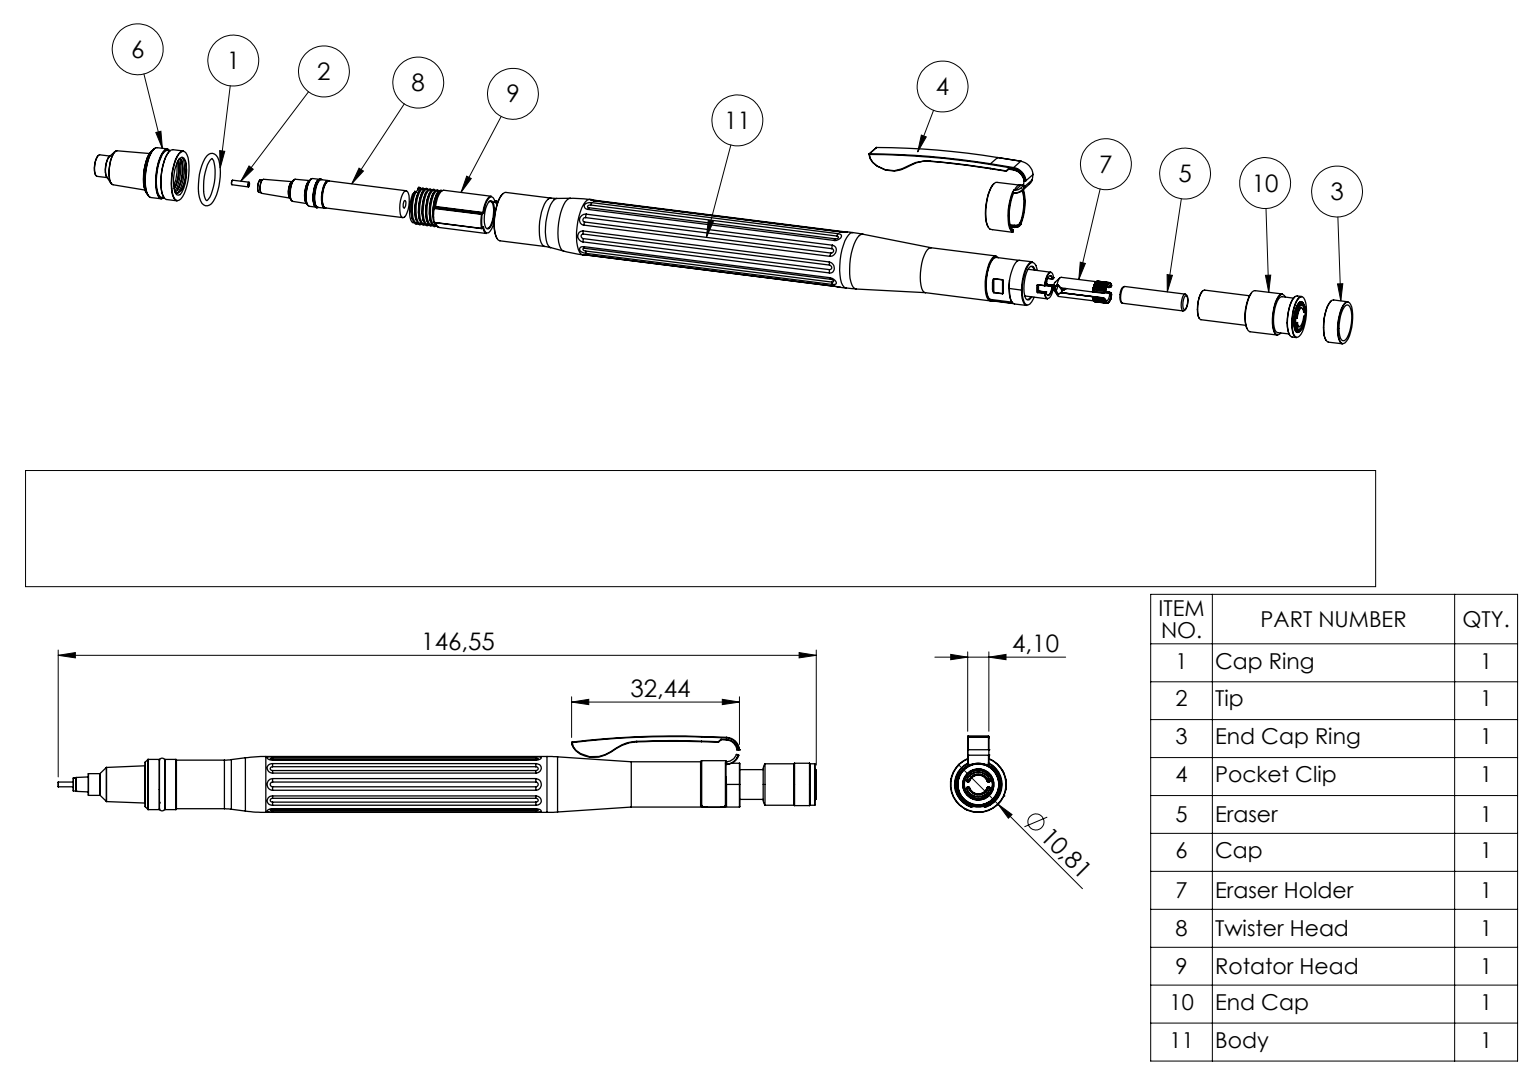
ISO-10303-21;
HEADER;
FILE_DESCRIPTION (('STEP AP214'),
    '1' );
FILE_NAME ('MAS-683',
    '2026-10-06T14:00:01',
    ( '' ),
    ( '' ),
    'SwSTEP 2.0',
    'SolidWorks 2020',
    '' );
FILE_SCHEMA (( 'AUTOMOTIVE_DESIGN' ));
ENDSEC;

DATA;
#1 = ORIENTED_EDGE ( 'NONE', *, *, #26816, .F. ) ;
#2 = CARTESIAN_POINT ( 'NONE',  ( 51.90000000000001279, -4.227689052994015206, -1.125730994152046804 ) ) ;
#3 = CARTESIAN_POINT ( 'NONE',  ( 15.76675455518197388, -3.095036031508637375, 4.435288302043580266 ) ) ;
#4 = CARTESIAN_POINT ( 'NONE',  ( 48.30000000000001847, 0.7900853852131533017, -4.025789903357282817 ) ) ;
#5 = ADVANCED_FACE ( 'NONE', ( #27029 ), #12933, .F. ) ;
#6 = FACE_OUTER_BOUND ( 'NONE', #21820, .T. ) ;
#7 = EDGE_CURVE ( 'NONE', #13124, #5233, #22627, .T. ) ;
#8 = CARTESIAN_POINT ( 'NONE',  ( -62.06147329307218286, -2.678446930503585843, 0.2197408810668839418 ) ) ;
#9 = AXIS2_PLACEMENT_3D ( 'NONE', #6479, #25787, #7416 ) ;
#10 = AXIS2_PLACEMENT_3D ( 'NONE', #12076, #19216, #28858 ) ;
#13 = EDGE_CURVE ( 'NONE', #19424, #10038, #3404, .T. ) ;
#12 = FACE_OUTER_BOUND ( 'NONE', #24808, .T. ) ;
#11 = PLANE ( 'NONE',  #16571 ) ;
#14 = B_SPLINE_CURVE_WITH_KNOTS ( 'NONE', 3,
 ( #5240, #644, #10304, #19973, #29610, #17605, #27249, #12178, #23901, #9510 ),
 .UNSPECIFIED., .F., .F.,
 ( 4, 2, 2, 2, 4 ),
 ( 0.000000000000000000, 0.0003925703575136129699, 0.0007851407150272259397, 0.001177711072540838910, 0.001570281430054451879 ),
 .UNSPECIFIED. ) ;
#15 = CARTESIAN_POINT ( 'NONE',  ( 61.23770293223015670, -0.8897917884444476178, 1.791164585743103999 ) ) ;
#17 = DIRECTION ( 'NONE',  ( 1.000000000000000000, 2.586136946169074517E-16, -0.000000000000000000 ) ) ;
#16 = CARTESIAN_POINT ( 'NONE',  ( -56.67499999999996874, 3.131991715727200307E-15, -1.107867533772800737E-16 ) ) ;
#18 = ORIENTED_EDGE ( 'NONE', *, *, #4179, .T. ) ;
#19 = CARTESIAN_POINT ( 'NONE',  ( 58.72419296898095809, -1.822284191842195256, 0.4419487341019822102 ) ) ;
#20 = FACE_OUTER_BOUND ( 'NONE', #25184, .T. ) ;
#22 = CARTESIAN_POINT ( 'NONE',  ( -35.98994760229849987, 4.804073784580248585, 2.042134692980175803 ) ) ;
#21 = DIRECTION ( 'NONE',  ( 0.000000000000000000, -1.000000000000000000, 0.000000000000000000 ) ) ;
#23 = LINE ( 'NONE', #15037, #26178 ) ;
#24 = ORIENTED_EDGE ( 'NONE', *, *, #28945, .F. ) ;
#25 = ORIENTED_EDGE ( 'NONE', *, *, #30906, .F. ) ;
#26 = FACE_OUTER_BOUND ( 'NONE', #14344, .T. ) ;
#27 = AXIS2_PLACEMENT_3D ( 'NONE', #565, #25255, #22895 ) ;
#28 = ORIENTED_EDGE ( 'NONE', *, *, #15447, .F. ) ;
#29 = CARTESIAN_POINT ( 'NONE',  ( 56.95000000000001705, 0.000000000000000000, 0.000000000000000000 ) ) ;
#30 = CARTESIAN_POINT ( 'NONE',  ( -35.85663232820584057, -3.426725943139554698, -3.937891353488750301 ) ) ;
#31 = ORIENTED_EDGE ( 'NONE', *, *, #27047, .T. ) ;
#32 = CARTESIAN_POINT ( 'NONE',  ( -59.59999999999998721, -2.157671697750204842, 1.538490443495526216 ) ) ;
#33 = ORIENTED_EDGE ( 'NONE', *, *, #2651, .T. ) ;
#34 = CARTESIAN_POINT ( 'NONE',  ( -60.95655989232410121, 1.962990915244748891, -3.400000000000207301 ) ) ;
#35 = ORIENTED_EDGE ( 'NONE', *, *, #5756, .F. ) ;
#36 = VERTEX_POINT ( 'NONE', #5192 ) ;
#37 = PRODUCT_DEFINITION_SHAPE ( 'NONE', 'NONE',  #1193 ) ;
#38 = ORIENTED_EDGE ( 'NONE', *, *, #18350, .T. ) ;
#39 = CIRCLE ( 'NONE', #6115, 0.4576450603546999840 ) ;
#40 = CARTESIAN_POINT ( 'NONE',  ( -59.74999999999995737, 2.023778652682510945E-14, -3.400000000000212186 ) ) ;
#41 = CARTESIAN_POINT ( 'NONE',  ( 53.71392934491857574, 7.814769211952036443, -2.050000000000187228 ) ) ;
#42 = CARTESIAN_POINT ( 'NONE',  ( 60.81599023037216512, -0.4999999999993630651, -1.863080903343643291 ) ) ;
#43 = CARTESIAN_POINT ( 'NONE',  ( -54.49999999999997868, -1.550000000000000044, 3.332135201338624508 ) ) ;
#44 = CARTESIAN_POINT ( 'NONE',  ( -58.09585481156723574, -1.184343223768586473, -3.558065644182725418 ) ) ;
#45 = EDGE_CURVE ( 'NONE', #27818, #13704, #24501, .T. ) ;
#47 = CARTESIAN_POINT ( 'NONE',  ( -35.85663232820581925, -0.4576450603547171925, -5.200000000000000178 ) ) ;
#46 = CARTESIAN_POINT ( 'NONE',  ( -59.69999999999997442, -3.399999999999991473, -2.235080921937235780E-13 ) ) ;
#48 =( NAMED_UNIT ( * ) PLANE_ANGLE_UNIT ( ) SI_UNIT ( $, .RADIAN. ) );
#49 = FACE_OUTER_BOUND ( 'NONE', #3992, .T. ) ;
#51 = DIRECTION ( 'NONE',  ( 0.000000000000000000, 1.224646799147353454E-16, 1.000000000000000000 ) ) ;
#50 = CARTESIAN_POINT ( 'NONE',  ( 54.42253022455169997, -6.265509898922181047E-05, -4.373069084971676013 ) ) ;
#52 = ORIENTED_EDGE ( 'NONE', *, *, #16574, .F. ) ;
#53 = DIRECTION ( 'NONE',  ( -1.000000000000000000, -0.000000000000000000, 3.491481338843133355E-15 ) ) ;
#54 = CARTESIAN_POINT ( 'NONE',  ( -36.00197790576391554, -4.683225679163350641, -2.703237727951247393 ) ) ;
#55 = AXIS2_PLACEMENT_3D ( 'NONE', #1109, #22822, #12810 ) ;
#57 = CARTESIAN_POINT ( 'NONE',  ( 54.19028661868582475, 6.697846887293304796, 2.049999999999810640 ) ) ;
#56 = CARTESIAN_POINT ( 'NONE',  ( 48.48092587705050960, -1.391939743175890420, 3.849999999996903899 ) ) ;
#58 = CARTESIAN_POINT ( 'NONE',  ( 47.10000000920868501, -4.079797993893489405, 2.128382101831542528 ) ) ;
#59 = ORIENTED_EDGE ( 'NONE', *, *, #31217, .T. ) ;
#60 = DIRECTION ( 'NONE',  ( 1.000000000000000000, 1.047444401652940007E-14, -0.000000000000000000 ) ) ;
#61 = AXIS2_PLACEMENT_3D ( 'NONE', #970, #25337, #5708 ) ;
#62 = EDGE_CURVE ( 'NONE', #4204, #12232, #6428, .T. ) ;
#63 = ORIENTED_EDGE ( 'NONE', *, *, #635, .F. ) ;
#64 = CARTESIAN_POINT ( 'NONE',  ( 51.80000000000002558, -3.933368109459642437, 2.186004417992994497 ) ) ;
#65 = CARTESIAN_POINT ( 'NONE',  ( -57.19702994616204705, 4.156921938165313080, -1.880369327726949834E-13 ) ) ;
#66 = VERTEX_POINT ( 'NONE', #447 ) ;
#67 = VERTEX_POINT ( 'NONE', #29413 ) ;
#68 = DIRECTION ( 'NONE',  ( 0.000000000000000000, -1.000000000000000000, 0.000000000000000000 ) ) ;
#69 = EDGE_LOOP ( 'NONE', ( #13659, #24370, #7129, #8608 ) ) ;
#70 = CARTESIAN_POINT ( 'NONE',  ( 48.45334018241207730, -1.329038565861417220, 3.861394075523871816 ) ) ;
#71 = CARTESIAN_POINT ( 'NONE',  ( -55.63452994616205416, 3.117691453623979481, 1.799999999999814415 ) ) ;
#72 = EDGE_LOOP ( 'NONE', ( #23840, #15915, #20433, #20236, #22335, #16297, #17891, #10389 ) ) ;
#73 = CARTESIAN_POINT ( 'NONE',  ( 63.50000000000004263, 0.7500000000000000000, 1.988246715072691018 ) ) ;
#74 = DIRECTION ( 'NONE',  ( -1.000000000000000000, -3.053848253006669023E-16, 2.042510438544995415E-16 ) ) ;
#75 = CARTESIAN_POINT ( 'NONE',  ( 29.99460041311888148, 6.535150002936795488, 2.049999999999441158 ) ) ;
#76 = VERTEX_POINT ( 'NONE', #8197 ) ;
#77 = CIRCLE ( 'NONE', #6150, 4.800000000000000711 ) ;
#78 = CARTESIAN_POINT ( 'NONE',  ( 56.95000000000001705, 0.6999999999999999556, -2.452039967047845437 ) ) ;
#79 = CARTESIAN_POINT ( 'NONE',  ( -54.49999516060625382, -1.549196738101655590, 4.063926895246979143 ) ) ;
#80 = DIRECTION ( 'NONE',  ( -1.000000000000000000, 0.000000000000000000, 1.047444401652940007E-14 ) ) ;
#81 = CARTESIAN_POINT ( 'NONE',  ( -59.60604010435355349, 3.187076279294280390, -1.184290838417780600 ) ) ;
#82 = CARTESIAN_POINT ( 'NONE',  ( 57.03951379057714632, 0.7794871794871794934, 1.732743413496389939 ) ) ;
#83 = EDGE_CURVE ( 'NONE', #616, #4702, #25049, .T. ) ;
#84 = B_SPLINE_CURVE_WITH_KNOTS ( 'NONE', 3,
 ( #27085, #16988, #10017, #5408 ),
 .UNSPECIFIED., .F., .F.,
 ( 4, 4 ),
 ( 0.000000000000000000, 2.862003379465075675E-05 ),
 .UNSPECIFIED. ) ;
#86 = CARTESIAN_POINT ( 'NONE',  ( -59.59999999999997300, -2.337126060168364994, -1.249136413240117038 ) ) ;
#85 =( NAMED_UNIT ( * ) SI_UNIT ( $, .STERADIAN. ) SOLID_ANGLE_UNIT ( ) );
#87 = FACE_OUTER_BOUND ( 'NONE', #20854, .T. ) ;
#88 = CARTESIAN_POINT ( 'NONE',  ( 51.80000000000001847, -3.726179070414208372, 1.041421356237310025 ) ) ;
#89 = AXIS2_PLACEMENT_3D ( 'NONE', #15577, #7805, #3067 ) ;
#90 = CARTESIAN_POINT ( 'NONE',  ( 61.24891880570161362, -0.9671362613607715764, -1.669082548205986116 ) ) ;
#91 = VERTEX_POINT ( 'NONE', #17714 ) ;
#92 = ORIENTED_EDGE ( 'NONE', *, *, #412, .F. ) ;
#93 = VECTOR ( 'NONE', #18197, 1000.000000000000000 ) ;
#94 = ADVANCED_FACE ( 'NONE', ( #17865 ), #19516, .T. ) ;
#95 = DIRECTION ( 'NONE',  ( 0.000000000000000000, -0.9996898646859343485, -0.02490330187381123786 ) ) ;
#96 = ORIENTED_EDGE ( 'NONE', *, *, #12745, .F. ) ;
#97 = CYLINDRICAL_SURFACE ( 'NONE', #25500, 1.000000000000000000 ) ;
#98 = CARTESIAN_POINT ( 'NONE',  ( -55.79792740578360366, 3.330682475591789871, 0.6830477631804102723 ) ) ;
#100 = PLANE ( 'NONE',  #28662 ) ;
#99 = CARTESIAN_POINT ( 'NONE',  ( 16.08093158123428523, 5.047763082740414298, 1.943828653492576608 ) ) ;
#101 = ORIENTED_EDGE ( 'NONE', *, *, #4763, .T. ) ;
#102 = ORIENTED_EDGE ( 'NONE', *, *, #5168, .T. ) ;
#103 = DIRECTION ( 'NONE',  ( 0.000000000000000000, 0.000000000000000000, -1.000000000000000000 ) ) ;
#104 = EDGE_LOOP ( 'NONE', ( #2125, #11645, #5974, #22411, #4642 ) ) ;
#105 = CYLINDRICAL_SURFACE ( 'NONE', #5460, 4.099999999999992539 ) ;
#106 =( BOUNDED_CURVE ( )  B_SPLINE_CURVE ( 2, ( #27982, #6938, #12441, #31145, #14352, #9477, #26546, #29083, #5166 ),
 .UNSPECIFIED., .F., .T. ) 
 B_SPLINE_CURVE_WITH_KNOTS ( ( 3, 2, 2, 2, 3 ),
 ( 0.5833333333333333703, 0.5925925925925925597, 0.6111111111111111605, 0.6296296296296296502, 0.6388888888888889506 ),
 .UNSPECIFIED. ) 
 CURVE ( )  GEOMETRIC_REPRESENTATION_ITEM ( )  RATIONAL_B_SPLINE_CURVE ( ( 0.9330127018922194093, 0.9330127018922197424, 1.000000000000000000, 0.8660254037844387076, 1.000000000000000000, 0.8660254037844387076, 1.000000000000000000, 0.9330127018922189652, 0.9330127018922194093 ) ) 
 REPRESENTATION_ITEM ( '' )  );
#107 = VERTEX_POINT ( 'NONE', #27203 ) ;
#108 = CARTESIAN_POINT ( 'NONE',  ( -36.40878371307408656, 5.360483378448119396, 0.7132926830813313135 ) ) ;
#109 = EDGE_LOOP ( 'NONE', ( #31265, #1632, #31131, #2632 ) ) ;
#110 = FACE_OUTER_BOUND ( 'NONE', #15279, .T. ) ;
#111 = EDGE_CURVE ( 'NONE', #4199, #30552, #22537, .T. ) ;
#112 = DIRECTION ( 'NONE',  ( 0.000000000000000000, 0.000000000000000000, -1.000000000000000000 ) ) ;
#113 = DIRECTION ( 'NONE',  ( -1.000000000000000000, -2.586136946169074517E-16, 0.000000000000000000 ) ) ;
#115 = CIRCLE ( 'NONE', #28430, 0.1000000000000002554 ) ;
#114 = CARTESIAN_POINT ( 'NONE',  ( -56.89405989232413674, -3.920666489018330156E-15, 3.399999999999796962 ) ) ;
#116 = CARTESIAN_POINT ( 'NONE',  ( 52.18319145150645255, 8.687974897284844289, -2.050000000000181455 ) ) ;
#117 = ADVANCED_FACE ( 'NONE', ( #25134 ), #3461, .F. ) ;
#118 = CARTESIAN_POINT ( 'NONE',  ( 58.65817410504259044, 0.5270377936603326541, 1.799623063671935475 ) ) ;
#119 = EDGE_CURVE ( 'NONE', #27144, #25407, #10724, .T. ) ;
#120 = CARTESIAN_POINT ( 'NONE',  ( 50.41422517315185559, 1.132063507975340277, -3.941224428058361262 ) ) ;
#121 = ADVANCED_FACE ( 'NONE', ( #2812 ), #19777, .T. ) ;
#122 = DIRECTION ( 'NONE',  ( 3.002035892788117459E-16, -0.9996898646859343485, -0.02490330187381124480 ) ) ;
#123 = ORIENTED_EDGE ( 'NONE', *, *, #26906, .T. ) ;
#124 = PLANE ( 'NONE',  #26575 ) ;
#125 = VERTEX_POINT ( 'NONE', #18190 ) ;
#126 = CARTESIAN_POINT ( 'NONE',  ( 61.25000000000002132, 6.415596960124259844E-13, 3.111507638930570854E-58 ) ) ;
#128 = CARTESIAN_POINT ( 'NONE',  ( 53.73313364444125995, 5.556159244632989491, 1.667741514041239048 ) ) ;
#127 = CARTESIAN_POINT ( 'NONE',  ( -36.21152527658242803, -3.291455042465435632, -4.036171416105485577 ) ) ;
#129 = CARTESIAN_POINT ( 'NONE',  ( 53.99324657738113586, 6.679477176219531742, 1.975347020395713526 ) ) ;
#130 = ORIENTED_EDGE ( 'NONE', *, *, #8388, .T. ) ;
#131 = EDGE_CURVE ( 'NONE', #11967, #18572, #4827, .T. ) ;
#132 = CARTESIAN_POINT ( 'NONE',  ( -54.45981523601835761, 1.500740478982482973, 4.030402907299741599 ) ) ;
#133 = VERTEX_POINT ( 'NONE', #3916 ) ;
#134 = FACE_OUTER_BOUND ( 'NONE', #215, .T. ) ;
#135 = CARTESIAN_POINT ( 'NONE',  ( 48.39253357792949117, 1.341874354110782486, 3.874311046529112623 ) ) ;
#137 = CARTESIAN_POINT ( 'NONE',  ( 47.44814918337031884, -3.852602532216165887, -1.405026670785768816 ) ) ;
#136 = CARTESIAN_POINT ( 'NONE',  ( 58.75000000000003553, -1.895722432252946010, 0.6373668173470157239 ) ) ;
#138 = ORIENTED_EDGE ( 'NONE', *, *, #14220, .T. ) ;
#139 = DIRECTION ( 'NONE',  ( 0.000000000000000000, 0.000000000000000000, 1.000000000000000000 ) ) ;
#140 = CARTESIAN_POINT ( 'NONE',  ( 15.03925126672133139, -3.817150320980667200, 2.203324261490537062 ) ) ;
#142 = LINE ( 'NONE', #17098, #13523 ) ;
#141 = CARTESIAN_POINT ( 'NONE',  ( 33.47623932017462778, 1.123735532908285650, -5.289358697221546279 ) ) ;
#143 = ORIENTED_EDGE ( 'NONE', *, *, #13652, .F. ) ;
#144 = CARTESIAN_POINT ( 'NONE',  ( -59.81249999999997158, 4.108500314926511798, -1.367561758111406567 ) ) ;
#145 = CARTESIAN_POINT ( 'NONE',  ( 58.65000000000003411, -1.394635017527761311, -1.253243060177727131 ) ) ;
#146 = DIRECTION ( 'NONE',  ( 0.000000000000000000, 0.000000000000000000, -1.000000000000000000 ) ) ;
#147 = EDGE_CURVE ( 'NONE', #30927, #10142, #27583, .T. ) ;
#148 = CARTESIAN_POINT ( 'NONE',  ( -41.12388279035661753, -1.755788972190012401E-14, 0.000000000000000000 ) ) ;
#149 = ITEM_DEFINED_TRANSFORMATION ( 'NONE', 'NONE', #18702,  #9018 ) ;
#150 = CARTESIAN_POINT ( 'NONE',  ( -61.38060080783325390, -2.623833477274086334, -0.6199702340732970995 ) ) ;
#151 = DIRECTION ( 'NONE',  ( 1.000000000000000000, -1.219044193948983948E-29, 3.491481338843133355E-15 ) ) ;
#153 = CARTESIAN_POINT ( 'NONE',  ( 68.00000000000001421, -1.025519176787267142E-28, -7.122621931239990530E-13 ) ) ;
#152 = AXIS2_PLACEMENT_3D ( 'NONE', #25976, #4453, #2803 ) ;
#154 = ORIENTED_EDGE ( 'NONE', *, *, #27235, .T. ) ;
#155 = ADVANCED_FACE ( 'NONE', ( #20723 ), #5995, .F. ) ;
#156 = CARTESIAN_POINT ( 'NONE',  ( 51.70000000000002416, 4.174380580618757719, 1.932497546739255556 ) ) ;
#157 = ADVANCED_FACE ( 'NONE', ( #22927 ), #25441, .T. ) ;
#158 = DIRECTION ( 'NONE',  ( -1.000000000000000000, -3.053848253006669023E-16, 2.042510438544995415E-16 ) ) ;
#159 = EDGE_CURVE ( 'NONE', #28004, #13558, #14466, .T. ) ;
#160 = CARTESIAN_POINT ( 'NONE',  ( -54.49999999999996447, 1.400000000000023670, -3.959797974644871044 ) ) ;
#161 = CARTESIAN_POINT ( 'NONE',  ( -56.62499999999997158, 1.184343223768582254, 3.558065644182727638 ) ) ;
#163 = CARTESIAN_POINT ( 'NONE',  ( 22.04321716858594371, 7.679566743993215816, 1.424999999999923661 ) ) ;
#162 = CARTESIAN_POINT ( 'NONE',  ( 58.75000000000001421, 0.5933779550744251452, 1.867062706146590756 ) ) ;
#164 = ORIENTED_EDGE ( 'NONE', *, *, #3455, .T. ) ;
#165 = CARTESIAN_POINT ( 'NONE',  ( 58.75000018803721247, -1.882836145342761780, 0.4533061784681521322 ) ) ;
#166 = LINE ( 'NONE', #7453, #15603 ) ;
#167 = AXIS2_PLACEMENT_3D ( 'NONE', #14057, #2660, #14363 ) ;
#169 = DIRECTION ( 'NONE',  ( 0.000000000000000000, -0.9996898646859343485, -0.02490330187381124133 ) ) ;
#168 = CARTESIAN_POINT ( 'NONE',  ( 51.64333574538936489, -0.8318165372340011743, -1.569663068107119974 ) ) ;
#170 = FACE_OUTER_BOUND ( 'NONE', #26252, .T. ) ;
#171 = VERTEX_POINT ( 'NONE', #25293 ) ;
#172 = ORIENTED_EDGE ( 'NONE', *, *, #3641, .F. ) ;
#173 = CARTESIAN_POINT ( 'NONE',  ( 51.41326833096621129, -0.9846823677975790057, -1.426744987257088315 ) ) ;
#174 = ORIENTED_EDGE ( 'NONE', *, *, #24601, .T. ) ;
#175 = DIRECTION ( 'NONE',  ( -3.491481338843133355E-15, -3.491481338843133355E-15, 1.000000000000000000 ) ) ;
#176 = CARTESIAN_POINT ( 'NONE',  ( 47.00000000000002132, 2.428612866367529932E-14, -4.100000000000022737 ) ) ;
#177 = ORIENTED_EDGE ( 'NONE', *, *, #3546, .F. ) ;
#178 = ADVANCED_FACE ( 'NONE', ( #15936 ), #13241, .T. ) ;
#179 = CARTESIAN_POINT ( 'NONE',  ( -35.98952425903315344, -5.086913993735696415, -1.171642046065874743 ) ) ;
#180 = ORIENTED_EDGE ( 'NONE', *, *, #3282, .F. ) ;
#181 = CARTESIAN_POINT ( 'NONE',  ( 58.74999999999980815, -1.394635017527639409, -1.253243060177863466 ) ) ;
#182 = EDGE_CURVE ( 'NONE', #17885, #28405, #12945, .T. ) ;
#183 = ORIENTED_EDGE ( 'NONE', *, *, #7527, .F. ) ;
#184 = EDGE_LOOP ( 'NONE', ( #28553, #23035, #27159, #29370 ) ) ;
#185 = CARTESIAN_POINT ( 'NONE',  ( -59.88452994616203995, -3.117691453623976816, 1.799999999999775335 ) ) ;
#186 = CARTESIAN_POINT ( 'NONE',  ( 54.23679421920400756, 6.620234584472831862, -2.050000000000189004 ) ) ;
#187 = FACE_OUTER_BOUND ( 'NONE', #28111, .T. ) ;
#188 = ADVANCED_FACE ( 'NONE', ( #10875 ), #20563, .T. ) ;
#189 = DIRECTION ( 'NONE',  ( 0.000000000000000000, -0.2008964009354148594, 0.9796124928211140670 ) ) ;
#190 = CARTESIAN_POINT ( 'NONE',  ( -61.37597047653181903, -2.565398393854171122, -0.8228970461733545738 ) ) ;
#191 = CARTESIAN_POINT ( 'NONE',  ( 46.99980596162997415, -4.243812330823901746, 1.064491855880303151 ) ) ;
#192 = CARTESIAN_POINT ( 'NONE',  ( 48.40116939571129961, 0.8930800907916158771, -3.925677024646232027 ) ) ;
#194 = CARTESIAN_POINT ( 'NONE',  ( 34.55000000000001847, 3.184081677783118191E-16, -2.600000000000000089 ) ) ;
#193 = DIRECTION ( 'NONE',  ( 0.9994629430332292452, 0.03275911391080331414, 0.0008160631928537054542 ) ) ;
#195 = ORIENTED_EDGE ( 'NONE', *, *, #1967, .T. ) ;
#196 = DIRECTION ( 'NONE',  ( 3.491481338843133750E-15, 0.000000000000000000, 1.000000000000000000 ) ) ;
#197 = CARTESIAN_POINT ( 'NONE',  ( -54.49999999999997868, 8.366749974758489177E-15, -2.216533082070116467E-13 ) ) ;
#199 = CARTESIAN_POINT ( 'NONE',  ( 52.72006341977384380, 4.014035108600657153, -0.8473018902927296203 ) ) ;
#198 = DIRECTION ( 'NONE',  ( 0.000000000000000000, 0.4531102586347437455, 0.8914544820235946743 ) ) ;
#200 = CARTESIAN_POINT ( 'NONE',  ( 48.00000000000002842, -4.387164041431067751, 1.383037119376590462 ) ) ;
#201 = ORIENTED_EDGE ( 'NONE', *, *, #2247, .T. ) ;
#202 = DIRECTION ( 'NONE',  ( 0.000000000000000000, -1.000000000000000000, 0.000000000000000000 ) ) ;
#203 = VERTEX_POINT ( 'NONE', #8511 ) ;
#204 = AXIS2_PLACEMENT_3D ( 'NONE', #12059, #22191, #17129 ) ;
#205 = CARTESIAN_POINT ( 'NONE',  ( 29.29107486424064888, 6.659593085418571867, 1.424999999999898126 ) ) ;
#206 = EDGE_LOOP ( 'NONE', ( #13546, #11977, #21657, #23791 ) ) ;
#207 = VERTEX_POINT ( 'NONE', #28132 ) ;
#208 = EDGE_CURVE ( 'NONE', #30643, #11413, #10315, .T. ) ;
#209 = CARTESIAN_POINT ( 'NONE',  ( 15.41170998834797778, 5.326676561279727551, 0.9978806102897876951 ) ) ;
#210 = ORIENTED_EDGE ( 'NONE', *, *, #23024, .T. ) ;
#211 = EDGE_CURVE ( 'NONE', #19416, #22328, #13432, .T. ) ;
#212 = B_SPLINE_CURVE_WITH_KNOTS ( 'NONE', 3,
 ( #23853, #28760, #23704, #11809, #1994, #9613, #29059, #26699, #21656, #24001, #19271, #11968, #26052 ),
 .UNSPECIFIED., .F., .F.,
 ( 4, 3, 3, 3, 4 ),
 ( 0.000000000000000000, 3.429247765843156239E-05, 6.861252194981137440E-05, 0.0001025118211733701013, 0.0001105094600589245180 ),
 .UNSPECIFIED. ) ;
#213 = CARTESIAN_POINT ( 'NONE',  ( 48.48434962373865886, -1.386108502191528924, 3.851082811767820413 ) ) ;
#214 = CARTESIAN_POINT ( 'NONE',  ( -55.32202994616205416, -4.156921938165296204, -2.115361882398036228E-13 ) ) ;
#215 = EDGE_LOOP ( 'NONE', ( #11588, #9037, #5325, #4414 ) ) ;
#216 = CARTESIAN_POINT ( 'NONE',  ( 54.49969840703174384, -0.002993017367635220170, 4.282759600741086636 ) ) ;
#217 = ADVANCED_FACE ( 'NONE', ( #691 ), #11323, .F. ) ;
#218 = FACE_OUTER_BOUND ( 'NONE', #18883, .T. ) ;
#219 = CIRCLE ( 'NONE', #12340, 2.000000000000000000 ) ;
#220 = CARTESIAN_POINT ( 'NONE',  ( 27.52339381995009049, 5.460762561607864995, 2.049999999999904787 ) ) ;
#221 = ORIENTED_EDGE ( 'NONE', *, *, #12347, .T. ) ;
#222 = CARTESIAN_POINT ( 'NONE',  ( -54.99999999999997868, 2.944486372867092250, 1.699999999999816103 ) ) ;
#223 = PLANE ( 'NONE',  #2312 ) ;
#224 = CARTESIAN_POINT ( 'NONE',  ( 58.75000000000000000, 2.008165151418601191, 0.5380862305919300592 ) ) ;
#225 = CYLINDRICAL_SURFACE ( 'NONE', #7886, 1.000000000000000000 ) ;
#226 = PLANE ( 'NONE',  #873 ) ;
#227 = CIRCLE ( 'NONE', #16912, 5.147405183146873675 ) ;
#228 = EDGE_CURVE ( 'NONE', #8009, #12847, #30638, .T. ) ;
#229 = DIRECTION ( 'NONE',  ( -1.000000000000000000, 0.000000000000000000, 1.047444401652940007E-14 ) ) ;
#230 = VECTOR ( 'NONE', #19201, 1000.000000000000000 ) ;
#231 = CARTESIAN_POINT ( 'NONE',  ( -59.63746166535423043, 3.180335144039268869, -1.202432085119870431 ) ) ;
#232 = CARTESIAN_POINT ( 'NONE',  ( 58.66133336607628479, 1.875011749337246014, -0.03256983989501838900 ) ) ;
#233 = DIRECTION ( 'NONE',  ( 1.000000000000000000, 1.047444401652940007E-14, 0.000000000000000000 ) ) ;
#234 = ORIENTED_EDGE ( 'NONE', *, *, #24307, .F. ) ;
#235 = ORIENTED_EDGE ( 'NONE', *, *, #4200, .F. ) ;
#236 = VERTEX_POINT ( 'NONE', #8450 ) ;
#237 =( BOUNDED_SURFACE ( )  B_SPLINE_SURFACE ( 3, 2, ( 
 ( #18207, #22472, #769 ),
 ( #20118, #8066, #17731 ),
 ( #5683, #3307, #12957 ),
 ( #11840, #21216, #1694 ),
 ( #4235, #13877, #16129 ),
 ( #28318, #30847, #18668 ),
 ( #14053, #11689, #9166 ),
 ( #18827, #11541, #18508 ),
 ( #23571, #16434, #23884 ),
 ( #28471, #4086, #21370 ),
 ( #6773, #6625, #1872 ),
 ( #26091, #21047, #30996 ),
 ( #16288, #9487, #23735 ),
 ( #25616, #2026, #30687 ),
 ( #28630, #2175, #8818 ),
 ( #21517, #4405, #13726 ) ),
 .UNSPECIFIED., .F., .F., .F. ) 
 B_SPLINE_SURFACE_WITH_KNOTS ( ( 4, 2, 2, 2, 2, 2, 2, 4 ),
 ( 3, 3 ),
 ( 0.001780502285214259107, 0.002558945925323788048, 0.002753556835351170500, 0.002948167745378552952, 0.003337389565433317423, 0.003726611385488081893, 0.004115833205542846797, 0.004894276845652375738 ),
 ( 0.000000000000000000, 1.000000000000000000 ),
 .UNSPECIFIED. ) 
 GEOMETRIC_REPRESENTATION_ITEM ( )  RATIONAL_B_SPLINE_SURFACE ( (
 ( 1.000000000000000000, 0.9418517008537233837, 1.000000000000000000),
 ( 1.000000000000000000, 0.9417987965885065149, 1.000000000000000000),
 ( 1.000000000000000000, 0.9418198861734086158, 1.000000000000000000),
 ( 1.000000000000000000, 0.9434060303845573925, 1.000000000000000000),
 ( 1.000000000000000000, 0.9437939819948161224, 1.000000000000000000),
 ( 1.000000000000000000, 0.9445989566712799101, 1.000000000000000000),
 ( 1.000000000000000000, 0.9450169930049959754, 1.000000000000000000),
 ( 1.000000000000000000, 0.9461610507673308135, 1.000000000000000000),
 ( 1.000000000000000000, 0.9467217966427053932, 1.000000000000000000),
 ( 1.000000000000000000, 0.9467345476124492398, 1.000000000000000000),
 ( 1.000000000000000000, 0.9461964028052997078, 1.000000000000000000),
 ( 1.000000000000000000, 0.9446801822473757104, 1.000000000000000000),
 ( 1.000000000000000000, 0.9437582546536171790, 1.000000000000000000),
 ( 1.000000000000000000, 0.9418129560296412128, 1.000000000000000000),
 ( 1.000000000000000000, 0.9418016889776917866, 1.000000000000000000),
 ( 1.000000000000000000, 0.9418517008537223845, 1.000000000000000000) ) ) 
 REPRESENTATION_ITEM ( '' )  SURFACE ( )  );
#238 = FACE_OUTER_BOUND ( 'NONE', #13734, .T. ) ;
#239 = CARTESIAN_POINT ( 'NONE',  ( -54.86042740578361077, -0.7887156198831597465, 3.845940847736172952 ) ) ;
#241 = CARTESIAN_POINT ( 'NONE',  ( -67.99999999999995737, -0.5554785485864222050, 2.708628542650383331 ) ) ;
#240 = CARTESIAN_POINT ( 'NONE',  ( 16.10667815269232150, 5.098435263432238962, 1.807398698456221142 ) ) ;
#242 = ORIENTED_EDGE ( 'NONE', *, *, #16474, .T. ) ;
#243 = AXIS2_PLACEMENT_3D ( 'NONE', #15272, #24917, #10208 ) ;
#244 = ORIENTED_EDGE ( 'NONE', *, *, #10930, .T. ) ;
#245 = AXIS2_PLACEMENT_3D ( 'NONE', #26689, #7358, #17036 ) ;
#246 = CARTESIAN_POINT ( 'NONE',  ( -44.49999999999997868, -1.499999999999998668, 4.029888335921975262 ) ) ;
#247 = VERTEX_POINT ( 'NONE', #25065 ) ;
#248 = EDGE_CURVE ( 'NONE', #1696, #20370, #611, .T. ) ;
#249 = DIRECTION ( 'NONE',  ( 1.000000000000000000, 1.047444401652940007E-14, 0.000000000000000000 ) ) ;
#250 = ORIENTED_EDGE ( 'NONE', *, *, #30955, .F. ) ;
#251 = CARTESIAN_POINT ( 'NONE',  ( 31.90749320720395588, 7.645246318247174599, -2.050000000000176570 ) ) ;
#252 = ADVANCED_FACE ( 'NONE', ( #17489 ), #5461, .T. ) ;
#253 = ORIENTED_EDGE ( 'NONE', *, *, #12134, .F. ) ;
#254 = CIRCLE ( 'NONE', #19476, 1.260000000000000231 ) ;
#255 = DIRECTION ( 'NONE',  ( -1.000000000000000000, -0.000000000000000000, 3.491481338843133355E-15 ) ) ;
#256 = DIRECTION ( 'NONE',  ( -1.000000000000000000, -0.000000000000000000, -0.000000000000000000 ) ) ;
#257 = CARTESIAN_POINT ( 'NONE',  ( 16.07512358269907438, -5.233646053067085191, -1.367284724151294872 ) ) ;
#258 = CIRCLE ( 'NONE', #12381, 0.2999999999999999334 ) ;
#259 = CARTESIAN_POINT ( 'NONE',  ( -54.45655989232412963, -3.925981830489445379, -2.076939516179772989E-13 ) ) ;
#260 = CARTESIAN_POINT ( 'NONE',  ( 53.91678946233204073, 6.821600947619984368, -1.787725782035514355 ) ) ;
#261 = EDGE_CURVE ( 'NONE', #13894, #14026, #10669, .T. ) ;
#262 = PLANE ( 'NONE',  #2851 ) ;
#263 = CARTESIAN_POINT ( 'NONE',  ( -36.39645873810205501, -3.590618801409528160, -4.051716037497291367 ) ) ;
#264 = AXIS2_PLACEMENT_3D ( 'NONE', #11573, #21251, #6807 ) ;
#265 = FILL_AREA_STYLE_COLOUR ( '', #10390 ) ;
#266 = CIRCLE ( 'NONE', #22541, 1.000000000000000000 ) ;
#267 = FACE_OUTER_BOUND ( 'NONE', #20625, .T. ) ;
#268 = ORIENTED_EDGE ( 'NONE', *, *, #4535, .F. ) ;
#269 = CARTESIAN_POINT ( 'NONE',  ( 56.99370871690835116, -0.8156862421929632623, -2.468735699563065378 ) ) ;
#270 = CARTESIAN_POINT ( 'NONE',  ( 51.50435016707359637, -0.9265794315402092751, -1.339215852266876672 ) ) ;
#271 = CARTESIAN_POINT ( 'NONE',  ( 53.91582462592152325, 6.672259099522118930, 0.8960560279709253173 ) ) ;
#272 = VECTOR ( 'NONE', #16238, 1000.000000000000000 ) ;
#273 = EDGE_LOOP ( 'NONE', ( #11335, #9422, #18646, #936 ) ) ;
#274 = CARTESIAN_POINT ( 'NONE',  ( 36.55000000000001847, 0.000000000000000000, -1.899999999999999911 ) ) ;
#275 =( BOUNDED_SURFACE ( )  B_SPLINE_SURFACE ( 3, 2, ( 
 ( #24839, #13578, #27853 ),
 ( #16132, #30851, #18355 ),
 ( #9002, #13880, #21051 ),
 ( #20886, #11544, #16291 ),
 ( #27992, #25934, #28322 ),
 ( #8822, #3767, #18511 ),
 ( #25783, #1876, #23266 ),
 ( #13729, #20588, #1550 ),
 ( #30222, #8528, #28153 ),
 ( #11213, #23111, #18831 ) ),
 .UNSPECIFIED., .F., .F., .T. ) 
 B_SPLINE_SURFACE_WITH_KNOTS ( ( 4, 2, 2, 2, 4 ),
 ( 3, 3 ),
 ( 0.0001706658715693258458, 0.0002229276920778027425, 0.0002751895125862796393, 0.0003274513330947565631, 0.0003797131536032334869 ),
 ( 0.000000000000000000, 1.000000000000000000 ),
 .UNSPECIFIED. ) 
 GEOMETRIC_REPRESENTATION_ITEM ( )  RATIONAL_B_SPLINE_SURFACE ( (
 ( 1.000000000000000000, 0.7071067811865444641, 1.000000000000000000),
 ( 1.000000000000000000, 0.7375607040701035455, 1.000000000000000000),
 ( 1.000000000000000000, 0.7730431127426561355, 1.000000000000000000),
 ( 1.000000000000000000, 0.8321012486983990764, 1.000000000000000000),
 ( 1.000000000000000000, 0.8541932017405543531, 1.000000000000000000),
 ( 1.000000000000000000, 0.8545723906055556762, 1.000000000000000000),
 ( 1.000000000000000000, 0.8327032135045047134, 1.000000000000000000),
 ( 1.000000000000000000, 0.7734559727062164658, 1.000000000000000000),
 ( 1.000000000000000000, 0.7377766653995503354, 1.000000000000000000),
 ( 1.000000000000000000, 0.7071067811865452413, 1.000000000000000000) ) ) 
 REPRESENTATION_ITEM ( '' )  SURFACE ( )  );
#276 = ORIENTED_EDGE ( 'NONE', *, *, #13970, .F. ) ;
#277 = TOROIDAL_SURFACE ( 'NONE', #6855, 3.950000000000000178, 0.05000000000000000278 ) ;
#278 = CARTESIAN_POINT ( 'NONE',  ( 15.22780280894145832, 0.7747498539022198427, -5.363501450340349308 ) ) ;
#279 = CARTESIAN_POINT ( 'NONE',  ( -36.56390771145526486, -5.205077242910963520, 1.471673150993815238 ) ) ;
#281 = DIRECTION ( 'NONE',  ( 0.9993908270190958731, -0.03489949670249358621, 0.000000000000000000 ) ) ;
#280 = CARTESIAN_POINT ( 'NONE',  ( 48.50000000000002132, -1.426739617975173013, -3.843750000000023093 ) ) ;
#282 = ORIENTED_EDGE ( 'NONE', *, *, #8503, .F. ) ;
#283 = DIRECTION ( 'NONE',  ( 0.000000000000000000, 0.9985773570672645816, 0.05332224631949589871 ) ) ;
#284 = ADVANCED_FACE ( 'NONE', ( #30591 ), #18007, .F. ) ;
#286 = CARTESIAN_POINT ( 'NONE',  ( 50.25000000000002132, 5.263408118306026973E-13, 3.111507638930570854E-58 ) ) ;
#285 = CARTESIAN_POINT ( 'NONE',  ( 51.80000048712027905, 3.919471135816211316, 2.045252759501752227 ) ) ;
#287 = EDGE_LOOP ( 'NONE', ( #23710, #1168, #11704, #9445, #24779, #21712, #30444 ) ) ;
#288 = CARTESIAN_POINT ( 'NONE',  ( -57.93749999999997158, -4.108500314926507357, 1.367561758111406567 ) ) ;
#289 = FACE_OUTER_BOUND ( 'NONE', #17501, .T. ) ;
#290 = CARTESIAN_POINT ( 'NONE',  ( 57.04536243881683788, -0.7794871794871796045, 1.732743413496389939 ) ) ;
#291 = AXIS2_PLACEMENT_3D ( 'NONE', #19148, #17077, #12003 ) ;
#292 = DIRECTION ( 'NONE',  ( -1.000000000000000000, -0.000000000000000000, -0.000000000000000000 ) ) ;
#293 = AXIS2_PLACEMENT_3D ( 'NONE', #30543, #21080, #28187 ) ;
#294 = FACE_OUTER_BOUND ( 'NONE', #8468, .T. ) ;
#295 = CARTESIAN_POINT ( 'NONE',  ( 58.75000000000003553, -1.655311165516605509, -1.077297519404007753 ) ) ;
#296 =( GEOMETRIC_REPRESENTATION_CONTEXT ( 3 ) GLOBAL_UNCERTAINTY_ASSIGNED_CONTEXT ( ( #20279 ) ) GLOBAL_UNIT_ASSIGNED_CONTEXT ( ( #24942, #22905, #24798 ) ) REPRESENTATION_CONTEXT ( 'NONE', 'WORKASPACE' ) );
#297 = ORIENTED_EDGE ( 'NONE', *, *, #11149, .T. ) ;
#298 = AXIS2_PLACEMENT_3D ( 'NONE', #23512, #1809, #21167 ) ;
#299 = AXIS2_PLACEMENT_3D ( 'NONE', #16364, #4639, #26010 ) ;
#300 = DIRECTION ( 'NONE',  ( 0.000000000000000000, 1.224646799147353454E-16, 1.000000000000000000 ) ) ;
#301 = CARTESIAN_POINT ( 'NONE',  ( 51.90000000000001279, 1.734723475976807094E-15, 0.000000000000000000 ) ) ;
#302 = CIRCLE ( 'NONE', #5869, 2.625000000001610267 ) ;
#303 = CARTESIAN_POINT ( 'NONE',  ( -54.49999999999996447, -1.499999999999978684, -4.029888335922192866 ) ) ;
#304 = EDGE_CURVE ( 'NONE', #17048, #21964, #18751, .T. ) ;
#305 = CIRCLE ( 'NONE', #30133, 0.05000000000000014849 ) ;
#306 = DIRECTION ( 'NONE',  ( 1.000000000000000000, 3.053848253006669023E-16, -2.042510438544995415E-16 ) ) ;
#308 = CARTESIAN_POINT ( 'NONE',  ( 22.44093457455321783, 6.836382162713700694, 1.424999999999920997 ) ) ;
#307 = CARTESIAN_POINT ( 'NONE',  ( 51.25173832208872682, -3.873874536552759373, 1.343508358799209379 ) ) ;
#309 = ORIENTED_EDGE ( 'NONE', *, *, #15470, .F. ) ;
#310 = CARTESIAN_POINT ( 'NONE',  ( 58.72427158855736451, -1.798991944511769470, 0.5288318043114524913 ) ) ;
#311 = AXIS2_PLACEMENT_3D ( 'NONE', #27449, #5763, #15416 ) ;
#312 = ORIENTED_EDGE ( 'NONE', *, *, #11950, .F. ) ;
#313 = PRODUCT_DEFINITION_CONTEXT ( 'detailed design', #27985, 'design' ) ;
#314 = FACE_OUTER_BOUND ( 'NONE', #22953, .T. ) ;
#316 = CARTESIAN_POINT ( 'NONE',  ( 58.74472430272383150, -0.4999999999993849364, -1.853787220596752272 ) ) ;
#315 = CARTESIAN_POINT ( 'NONE',  ( 57.01990854087920013, 0.7399312420039723115, -2.427820937803477630 ) ) ;
#317 = DIRECTION ( 'NONE',  ( 1.000000000000000000, 3.053848253006669023E-16, -2.042510438544995415E-16 ) ) ;
#318 = AXIS2_PLACEMENT_3D ( 'NONE', #9279, #4194, #20999 ) ;
#319 = ORIENTED_EDGE ( 'NONE', *, *, #23903, .T. ) ;
#320 = VERTEX_POINT ( 'NONE', #1312 ) ;
#321 = CARTESIAN_POINT ( 'NONE',  ( 51.78416995154975666, -0.8999235898776958287, -1.360374659026170718 ) ) ;
#322 = AXIS2_PLACEMENT_3D ( 'NONE', #6296, #16124, #30840 ) ;
#323 = AXIS2_PLACEMENT_3D ( 'NONE', #26001, #1950, #28541 ) ;
#324 = EDGE_CURVE ( 'NONE', #29888, #4483, #21821, .T. ) ;
#325 = DIRECTION ( 'NONE',  ( -1.000000000000000000, -2.586136946169074517E-16, 0.000000000000000000 ) ) ;
#326 = ORIENTED_EDGE ( 'NONE', *, *, #1422, .T. ) ;
#327 = AXIS2_PLACEMENT_3D ( 'NONE', #3583, #20536, #15450 ) ;
#328 = CARTESIAN_POINT ( 'NONE',  ( 51.70000000000001705, -4.179189514726507682, 0.9999999999999997780 ) ) ;
#329 = EDGE_CURVE ( 'NONE', #6782, #11116, #30403, .T. ) ;
#330 = CARTESIAN_POINT ( 'NONE',  ( -55.11042740578361077, 3.725040285533371076, -1.239922660687676315 ) ) ;
#331 = EDGE_CURVE ( 'NONE', #21866, #1670, #17624, .T. ) ;
#332 = CARTESIAN_POINT ( 'NONE',  ( -36.92443669619682112, -5.094475812726876995, -1.819860688632578771 ) ) ;
#333 = VERTEX_POINT ( 'NONE', #21741 ) ;
#334 = DIRECTION ( 'NONE',  ( -3.208218335192195507E-15, 0.9428090415820656878, 0.3333333333333268200 ) ) ;
#335 = CIRCLE ( 'NONE', #10516, 1.875000000000001776 ) ;
#336 = AXIS2_PLACEMENT_3D ( 'NONE', #3654, #22838, #15841 ) ;
#337 = ORIENTED_EDGE ( 'NONE', *, *, #17482, .F. ) ;
#338 = AXIS2_PLACEMENT_3D ( 'NONE', #16361, #30597, #23665 ) ;
#339 = CARTESIAN_POINT ( 'NONE',  ( -58.44702994616205416, -2.078460969082657872, 3.599999999999784261 ) ) ;
#340 = CIRCLE ( 'NONE', #30668, 0.05000000000000007216 ) ;
#341 = CARTESIAN_POINT ( 'NONE',  ( 50.40811050917463376, 1.340787288841451819, 3.874691554877328414 ) ) ;
#342 = PLANE ( 'NONE',  #13632 ) ;
#343 = CARTESIAN_POINT ( 'NONE',  ( -54.47754877553799702, -1.508273929415538506, 3.305418158118663463 ) ) ;
#344 = FACE_OUTER_BOUND ( 'NONE', #13767, .T. ) ;
#345 = CIRCLE ( 'NONE', #29674, 0.1500000000000001887 ) ;
#346 = CARTESIAN_POINT ( 'NONE',  ( 58.66133336607573057, -1.802692578418147118, 0.5167488000325648478 ) ) ;
#347 =( GEOMETRIC_REPRESENTATION_CONTEXT ( 3 ) GLOBAL_UNCERTAINTY_ASSIGNED_CONTEXT ( ( #22477 ) ) GLOBAL_UNIT_ASSIGNED_CONTEXT ( ( #9070, #19057, #4625 ) ) REPRESENTATION_CONTEXT ( 'NONE', 'WORKASPACE' ) );
#349 = CARTESIAN_POINT ( 'NONE',  ( -36.43290890416756866, 0.4851603899458080682, -5.391500295856532787 ) ) ;
#348 = DIRECTION ( 'NONE',  ( -1.000000000000000000, -0.000000000000000000, 3.491481338843133355E-15 ) ) ;
#350 = EDGE_CURVE ( 'NONE', #30188, #2736, #13683, .T. ) ;
#351 = DIRECTION ( 'NONE',  ( 0.000000000000000000, -0.2008964009354143876, 0.9796124928211140670 ) ) ;
#352 = DIRECTION ( 'NONE',  ( -1.000000000000000000, -0.000000000000000000, 1.047444401652940007E-14 ) ) ;
#354 = CARTESIAN_POINT ( 'NONE',  ( 56.95000000000001705, -0.7137254901960784492, 2.500119182087999548 ) ) ;
#353 = CARTESIAN_POINT ( 'NONE',  ( 15.49702763512084047, 4.928592478219022688, -1.658905555082578864 ) ) ;
#355 = VERTEX_POINT ( 'NONE', #14878 ) ;
#356 = DIRECTION ( 'NONE',  ( 1.047444401652940007E-14, 0.000000000000000000, 1.000000000000000000 ) ) ;
#357 = EDGE_CURVE ( 'NONE', #13475, #23396, #17276, .T. ) ;
#358 = CARTESIAN_POINT ( 'NONE',  ( -60.49999999999995737, 1.963826825011730345E-15, 6.704595576490977020E-16 ) ) ;
#359 = CIRCLE ( 'NONE', #3392, 1.975000000000001865 ) ;
#361 = CARTESIAN_POINT ( 'NONE',  ( 52.91788431598524056, 4.099929541424792490, -0.1776868343159781760 ) ) ;
#360 = DIRECTION ( 'NONE',  ( 1.000000000000000000, 1.047444401652940007E-14, 0.000000000000000000 ) ) ;
#362 = CARTESIAN_POINT ( 'NONE',  ( 47.10000000000002984, -4.020776289669855785, 2.234582293948413678 ) ) ;
#363 = VERTEX_POINT ( 'NONE', #7618 ) ;
#364 = CARTESIAN_POINT ( 'NONE',  ( 33.47623932017462778, 1.734723475976807489E-15, 0.000000000000000000 ) ) ;
#365 = AXIS2_PLACEMENT_3D ( 'NONE', #25779, #23413, #7408 ) ;
#366 = ORIENTED_EDGE ( 'NONE', *, *, #22608, .F. ) ;
#367 = DIRECTION ( 'NONE',  ( 1.000000000000000000, 1.047444401652940007E-14, 0.000000000000000000 ) ) ;
#368 = EDGE_LOOP ( 'NONE', ( #14579, #11671, #14342, #26811 ) ) ;
#369 = ORIENTED_EDGE ( 'NONE', *, *, #19982, .T. ) ;
#370 = ADVANCED_FACE ( 'NONE', ( #29150 ), #19356, .F. ) ;
#371 = CARTESIAN_POINT ( 'NONE',  ( 15.56401610563845317, 5.370189181194952255, 0.6649548426264916268 ) ) ;
#372 = ORIENTED_EDGE ( 'NONE', *, *, #29152, .T. ) ;
#373 = CARTESIAN_POINT ( 'NONE',  ( 48.40000000000001990, -0.6304760106459033064, 3.950000000000022826 ) ) ;
#374 = CIRCLE ( 'NONE', #8458, 0.05000000000000012768 ) ;
#375 = CARTESIAN_POINT ( 'NONE',  ( -54.33155989232412253, -1.962990915244706924, -3.400000000000199751 ) ) ;
#376 = ORIENTED_EDGE ( 'NONE', *, *, #28015, .T. ) ;
#377 = CARTESIAN_POINT ( 'NONE',  ( 51.80000000000001847, 0.2793919678926817252, -0.9601771338026217073 ) ) ;
#378 = AXIS2_PLACEMENT_3D ( 'NONE', #1428, #11090, #30545 ) ;
#379 = AXIS2_PLACEMENT_3D ( 'NONE', #22161, #7586, #5825 ) ;
#380 = CARTESIAN_POINT ( 'NONE',  ( -35.85663232820584057, 1.793057972834822156, -4.026191436120376999 ) ) ;
#381 = CARTESIAN_POINT ( 'NONE',  ( 32.30803788440357494, 7.816246120667637243, 2.049999999999888356 ) ) ;
#382 = ORIENTED_EDGE ( 'NONE', *, *, #29422, .T. ) ;
#383 = CARTESIAN_POINT ( 'NONE',  ( 51.89360908398760586, 0.6611756245550776123, -1.497563819580874922 ) ) ;
#384 = CARTESIAN_POINT ( 'NONE',  ( -54.48779575765000516, -1.517266520141195896, 4.041867453639656382 ) ) ;
#385 = CARTESIAN_POINT ( 'NONE',  ( 58.72427158855720819, -0.9764256747734804120, -1.600821037878335185 ) ) ;
#386 = AXIS2_PLACEMENT_3D ( 'NONE', #15477, #25133, #23717 ) ;
#387 = CARTESIAN_POINT ( 'NONE',  ( -59.66183546925923764, -3.174920041538525251, -1.216504307364950854 ) ) ;
#388 = CARTESIAN_POINT ( 'NONE',  ( 51.18802626461298644, 0.9696678249730820154, 1.452003249885708946 ) ) ;
#389 = CIRCLE ( 'NONE', #18100, 0.1000000000000000749 ) ;
#390 = CIRCLE ( 'NONE', #15052, 160.1997717543138720 ) ;
#392 = CARTESIAN_POINT ( 'NONE',  ( 58.75000000000002842, -1.077297519403676906, 1.655311165517035166 ) ) ;
#391 =( NAMED_UNIT ( * ) PLANE_ANGLE_UNIT ( ) SI_UNIT ( $, .RADIAN. ) );
#393 = ADVANCED_FACE ( 'NONE', ( #19503 ), #26715, .T. ) ;
#394 = CARTESIAN_POINT ( 'NONE',  ( 51.17290532404582137, 0.9646187004851747293, 1.462925393634774363 ) ) ;
#395 = EDGE_CURVE ( 'NONE', #29448, #3131, #5108, .T. ) ;
#396 = DIRECTION ( 'NONE',  ( 0.000000000000000000, -1.000000000000000000, -3.491481338843133355E-15 ) ) ;
#397 = CIRCLE ( 'NONE', #4439, 0.1000000000000000472 ) ;
#398 = CARTESIAN_POINT ( 'NONE',  ( 61.24637336955063915, -0.9388313581414567954, -1.688008567904763835 ) ) ;
#399 = EDGE_CURVE ( 'NONE', #24313, #24734, #20298, .T. ) ;
#400 = ORIENTED_EDGE ( 'NONE', *, *, #15115, .F. ) ;
#401 = ORIENTED_EDGE ( 'NONE', *, *, #30815, .F. ) ;
#402 = EDGE_LOOP ( 'NONE', ( #25249, #26786, #6480, #5576 ) ) ;
#403 = DIRECTION ( 'NONE',  ( 2.614375865348240525E-16, -0.2008964009354147762, 0.9796124928211140670 ) ) ;
#404 = CARTESIAN_POINT ( 'NONE',  ( -59.98542740578359656, -3.725040285533365303, 1.239922660687675871 ) ) ;
#406 = DIRECTION ( 'NONE',  ( 1.000000000000000000, 1.047444401652940007E-14, 0.000000000000000000 ) ) ;
#405 = CARTESIAN_POINT ( 'NONE',  ( -54.56249999999997158, -1.962990915244707368, -3.400000000000200640 ) ) ;
#407 = CIRCLE ( 'NONE', #8905, 0.1000000000000003386 ) ;
#408 = ORIENTED_EDGE ( 'NONE', *, *, #18853, .F. ) ;
#409 = ORIENTED_EDGE ( 'NONE', *, *, #20294, .F. ) ;
#410 = CARTESIAN_POINT ( 'NONE',  ( -56.03335481156723574, -4.108500314926509134, 1.367561758111407455 ) ) ;
#411 = ORIENTED_EDGE ( 'NONE', *, *, #1166, .F. ) ;
#412 = EDGE_CURVE ( 'NONE', #3421, #11190, #26852, .T. ) ;
#413 = DIRECTION ( 'NONE',  ( -1.000000000000000000, -0.000000000000000000, 3.491481338843133355E-15 ) ) ;
#414 = CIRCLE ( 'NONE', #1347, 1.875000000000001776 ) ;
#415 = ORIENTED_EDGE ( 'NONE', *, *, #7693, .T. ) ;
#416 = CARTESIAN_POINT ( 'NONE',  ( 33.97298909694990243, 8.288184271123828495, -2.050000000000117506 ) ) ;
#417 = ORIENTED_EDGE ( 'NONE', *, *, #10614, .T. ) ;
#418 = CARTESIAN_POINT ( 'NONE',  ( -73.89999999999997726, 0.4598573377555273400, 0.01145551886195788835 ) ) ;
#419 = CARTESIAN_POINT ( 'NONE',  ( -44.59999999999998721, -1.557046979865776226, 3.273565289174722448 ) ) ;
#420 = CARTESIAN_POINT ( 'NONE',  ( 15.41217651307630376, -4.863043649742736285, -1.860644097022675414 ) ) ;
#421 = CARTESIAN_POINT ( 'NONE',  ( -60.13452994616204705, 3.117691453623979481, 1.799999999999798428 ) ) ;
#422 = CARTESIAN_POINT ( 'NONE',  ( 52.54946733419065197, 4.465216787881845839, -1.565330858589896845 ) ) ;
#423 = CARTESIAN_POINT ( 'NONE',  ( 51.45655683570189609, 0.9591657938401617622, -1.518428463906025705 ) ) ;
#424 = CARTESIAN_POINT ( 'NONE',  ( 50.36059168657180862, 1.279117291415143853, -3.870058441400159754 ) ) ;
#425 = AXIS2_PLACEMENT_3D ( 'NONE', #10899, #22657, #18053 ) ;
#426 = CARTESIAN_POINT ( 'NONE',  ( 15.18463186935387377, -4.683225679163126820, -2.703237727951754543 ) ) ;
#427 = EDGE_CURVE ( 'NONE', #3316, #29448, #13185, .T. ) ;
#428 = DIRECTION ( 'NONE',  ( -1.000000000000000000, -0.000000000000000000, 3.491481338843133750E-15 ) ) ;
#429 =( BOUNDED_CURVE ( )  B_SPLINE_CURVE ( 2, ( #24054, #26755, #4426, #29116, #12032, #9964, #7268, #5054, #28814 ),
 .UNSPECIFIED., .F., .T. ) 
 B_SPLINE_CURVE_WITH_KNOTS ( ( 3, 2, 2, 2, 3 ),
 ( 0.4722222222222222654, 0.4814814814814814548, 0.5000000000000000000, 0.5185185185185184897, 0.5277777777777777901 ),
 .UNSPECIFIED. ) 
 CURVE ( )  GEOMETRIC_REPRESENTATION_ITEM ( )  RATIONAL_B_SPLINE_CURVE ( ( 0.9330127018922194093, 0.9330127018922197424, 1.000000000000000000, 0.8660254037844387076, 1.000000000000000000, 0.8660254037844387076, 1.000000000000000000, 0.9330127018922194093, 0.9330127018922194093 ) ) 
 REPRESENTATION_ITEM ( '' )  );
#430 = ORIENTED_EDGE ( 'NONE', *, *, #6181, .F. ) ;
#431 = LINE ( 'NONE', #17079, #18420 ) ;
#432 = CARTESIAN_POINT ( 'NONE',  ( -36.68133364217528225, -3.736273719777210456, -3.909490113446789206 ) ) ;
#433 = CARTESIAN_POINT ( 'NONE',  ( 53.90733871594494531, 6.075395493854959028, -1.402257306246839752 ) ) ;
#434 = ORIENTED_EDGE ( 'NONE', *, *, #19502, .F. ) ;
#435 = CARTESIAN_POINT ( 'NONE',  ( -44.49999999999999289, 1.399999999999998135, 3.363870538531281262 ) ) ;
#436 = ORIENTED_EDGE ( 'NONE', *, *, #1318, .F. ) ;
#437 =( LENGTH_UNIT ( ) NAMED_UNIT ( * ) SI_UNIT ( .MILLI., .METRE. ) );
#438 = CARTESIAN_POINT ( 'NONE',  ( -36.11692583559979397, -4.683225668089311178, 2.703237747136467473 ) ) ;
#440 = CARTESIAN_POINT ( 'NONE',  ( 56.95000000000001705, 0.000000000000000000, 0.000000000000000000 ) ) ;
#439 = CARTESIAN_POINT ( 'NONE',  ( 69.20000000000005969, -0.7500000000000000000, 1.988246715072633508 ) ) ;
#441 = EDGE_LOOP ( 'NONE', ( #30062, #24496, #16415, #15926 ) ) ;
#442 = CARTESIAN_POINT ( 'NONE',  ( 58.75000000000001421, 0.5380862305905714793, 2.008165151419250449 ) ) ;
#443 = ADVANCED_FACE ( 'NONE', ( #24852 ), #20138, .T. ) ;
#444 = CARTESIAN_POINT ( 'NONE',  ( 50.50000000000002132, 0.6304760106459513791, 3.950000000000021938 ) ) ;
#446 = CARTESIAN_POINT ( 'NONE',  ( -54.44999999999997442, 0.000000000000000000, 4.349999999999997868 ) ) ;
#445 = DIRECTION ( 'NONE',  ( -1.000000000000000000, -1.047444401652940007E-14, -0.000000000000000000 ) ) ;
#447 = CARTESIAN_POINT ( 'NONE',  ( -74.39999999999997726, -0.4598573377555325026, -0.01145551886194846360 ) ) ;
#448 = CARTESIAN_POINT ( 'NONE',  ( -60.81249999999997158, -3.238593381231841040, -2.874284765127020247 ) ) ;
#449 = FACE_OUTER_BOUND ( 'NONE', #30131, .T. ) ;
#450 = CARTESIAN_POINT ( 'NONE',  ( -55.24999999999997868, 3.673546848079180638, 0.7533615035078062849 ) ) ;
#451 = PRESENTATION_LAYER_ASSIGNMENT (  '', '', ( #28252 ) ) ;
#452 = AXIS2_PLACEMENT_3D ( 'NONE', #22650, #10741, #10597 ) ;
#453 = DIRECTION ( 'NONE',  ( -2.095850865446309212E-30, -1.000000000000000000, -2.891205793294679411E-15 ) ) ;
#454 = DIRECTION ( 'NONE',  ( -1.000000000000000000, 0.000000000000000000, 1.047444401652940007E-14 ) ) ;
#455 = DIRECTION ( 'NONE',  ( -1.000000000000000000, -3.054025858079668409E-16, 2.042474015755241579E-16 ) ) ;
#456 = CARTESIAN_POINT ( 'NONE',  ( 51.84831113588977303, -0.6920605891655385866, -1.653603923793142361 ) ) ;
#457 = ORIENTED_EDGE ( 'NONE', *, *, #26462, .T. ) ;
#458 = CIRCLE ( 'NONE', #5023, 0.05000000000000012768 ) ;
#459 = DIRECTION ( 'NONE',  ( 1.000000000000000000, -1.219044193948983948E-29, 3.491481338843133355E-15 ) ) ;
#460 = EDGE_CURVE ( 'NONE', #25198, #24785, #24329, .T. ) ;
#461 = B_SPLINE_CURVE_WITH_KNOTS ( 'NONE', 3,
 ( #4222, #6930, #25918, #30983 ),
 .UNSPECIFIED., .F., .F.,
 ( 4, 4 ),
 ( 0.0002256372043837409917, 0.0002420867138521805458 ),
 .UNSPECIFIED. ) ;
#462 = CARTESIAN_POINT ( 'NONE',  ( -59.37009172985672478, 3.234433134214944161, -1.048065980887175952 ) ) ;
#463 = CARTESIAN_POINT ( 'NONE',  ( 65.04999999999996874, -1.025519176787267142E-28, -4.100000000000681766 ) ) ;
#464 = CARTESIAN_POINT ( 'NONE',  ( 23.09424125814508955, 6.161968159343407692, 1.424999999999919664 ) ) ;
#465 = EDGE_LOOP ( 'NONE', ( #3537, #28913, #30616, #5077 ) ) ;
#466 = CIRCLE ( 'NONE', #9064, 0.1499999999999998557 ) ;
#467 = DIRECTION ( 'NONE',  ( 1.000000000000000000, 3.385297212316258532E-16, -2.459562394685744279E-16 ) ) ;
#468 = VERTEX_POINT ( 'NONE', #17898 ) ;
#469 = DIRECTION ( 'NONE',  ( 0.000000000000000000, 0.000000000000000000, 1.000000000000000000 ) ) ;
#471 = CARTESIAN_POINT ( 'NONE',  ( 47.10000000000000853, -4.020776289669854009, -2.234582293948742748 ) ) ;
#470 = CARTESIAN_POINT ( 'NONE',  ( -54.46975615167505680, -2.293836137973780165, -2.770930891520435146 ) ) ;
#472 = DIRECTION ( 'NONE',  ( 0.6819983600624907050, -0.7313537016191778983, -2.168404344971033323E-15 ) ) ;
#473 = VERTEX_POINT ( 'NONE', #3169 ) ;
#474 = ORIENTED_EDGE ( 'NONE', *, *, #7320, .T. ) ;
#475 = DIRECTION ( 'NONE',  ( -1.000000000000000000, -0.000000000000000000, -0.000000000000000000 ) ) ;
#476 = EDGE_CURVE ( 'NONE', #20395, #3490, #29876, .T. ) ;
#477 = CARTESIAN_POINT ( 'NONE',  ( 58.75000000000002132, 6.153735859711025284E-13, 3.111507638930570854E-58 ) ) ;
#478 = ORIENTED_EDGE ( 'NONE', *, *, #27718, .F. ) ;
#479 = DIRECTION ( 'NONE',  ( 1.000000000000000000, -0.000000000000000000, -1.047444401652940007E-14 ) ) ;
#480 = CARTESIAN_POINT ( 'NONE',  ( 50.39883060428874728, 0.8930800907916158771, 3.925677024646232027 ) ) ;
#481 = CARTESIAN_POINT ( 'NONE',  ( -36.68133364217572989, -5.320649567603509489, -0.9667173501063568430 ) ) ;
#482 = ORIENTED_EDGE ( 'NONE', *, *, #30906, .T. ) ;
#483 =( NAMED_UNIT ( * ) PLANE_ANGLE_UNIT ( ) SI_UNIT ( $, .RADIAN. ) );
#484 = DIRECTION ( 'NONE',  ( 0.000000000000000000, -0.2008964009354147762, 0.9796124928211140670 ) ) ;
#485 = AXIS2_PLACEMENT_3D ( 'NONE', #31169, #14065, #21059 ) ;
#486 = APPLICATION_CONTEXT ( 'automotive_design' ) ;
#487 = EDGE_CURVE ( 'NONE', #25704, #26503, #27864, .T. ) ;
#488 = B_SPLINE_CURVE_WITH_KNOTS ( 'NONE', 3,
 ( #12965, #29908, #15508, #8530, #3628, #17581, #20429, #20126, #6019, #10443, #30224, #18216, #25166, #5538, #13122, #20591 ),
 .UNSPECIFIED., .F., .F.,
 ( 4, 3, 3, 3, 3, 4 ),
 ( -2.161317903555403524E-06, 0.000000000000000000, 3.447636036923519868E-05, 7.048537632665564262E-05, 0.0001024680845135426304, 0.0001336460163216753082 ),
 .UNSPECIFIED. ) ;
#489 = VERTEX_POINT ( 'NONE', #20441 ) ;
#490 = CIRCLE ( 'NONE', #22257, 2.000000000000000000 ) ;
#491 = TOROIDAL_SURFACE ( 'NONE', #10107, 2.674999999999998934, 0.05000000000000000278 ) ;
#492 = CARTESIAN_POINT ( 'NONE',  ( -58.50952994616205416, -4.643455692769885398E-15, 3.599999999999791367 ) ) ;
#493 = DIRECTION ( 'NONE',  ( 1.000000000000000000, 1.047444401652940007E-14, 0.000000000000000000 ) ) ;
#494 = CARTESIAN_POINT ( 'NONE',  ( 48.37881665787880081, -1.311095223031167656, -3.884869838566831657 ) ) ;
#495 = CARTESIAN_POINT ( 'NONE',  ( -59.69999999999998153, -2.279157448682842091, 1.538811659727345349 ) ) ;
#496 = CARTESIAN_POINT ( 'NONE',  ( 51.80019403837007275, -4.243812330823898193, -1.064491855880295157 ) ) ;
#497 = AXIS2_PLACEMENT_3D ( 'NONE', #10217, #15753, #20048 ) ;
#498 = CARTESIAN_POINT ( 'NONE',  ( -77.28999999999996362, -3.470778894058966809E-15, 5.300300110251643219E-15 ) ) ;
#500 = CARTESIAN_POINT ( 'NONE',  ( -61.38648119981476015, -2.567347173575106556, -0.8311979704516511136 ) ) ;
#499 = CARTESIAN_POINT ( 'NONE',  ( 47.10000000000002274, 2.428612866367529932E-14, -1.644487710595116631E-13 ) ) ;
#501 = EDGE_CURVE ( 'NONE', #21780, #20962, #6621, .T. ) ;
#502 = EDGE_CURVE ( 'NONE', #31046, #17227, #27711, .T. ) ;
#503 = CARTESIAN_POINT ( 'NONE',  ( -62.09267578295094125, -2.518691627519130449, 0.1783745650731504706 ) ) ;
#504 = CARTESIAN_POINT ( 'NONE',  ( 64.99999999999997158, -1.025519176787267142E-28, -3.500000000000680345 ) ) ;
#506 = DIRECTION ( 'NONE',  ( 0.000000000000000000, -0.3529411764705882026, -0.9356455129756979794 ) ) ;
#505 = CARTESIAN_POINT ( 'NONE',  ( 15.17256654081408307, 4.804073784580281448, -2.042134692980007937 ) ) ;
#507 = VERTEX_POINT ( 'NONE', #5861 ) ;
#508 = LINE ( 'NONE', #19531, #10386 ) ;
#509 = CARTESIAN_POINT ( 'NONE',  ( 47.19811728011942620, -4.191430714671217750, -1.624095931900840117 ) ) ;
#511 = CARTESIAN_POINT ( 'NONE',  ( 50.25000000000002842, -0.6373668173474561494, 1.895722432253304168 ) ) ;
#510 = CARTESIAN_POINT ( 'NONE',  ( 15.29449157529453984, 2.734387802834222558, -4.440904455451668120 ) ) ;
#512 = PLANE ( 'NONE',  #27168 ) ;
#513 = ORIENTED_EDGE ( 'NONE', *, *, #6499, .F. ) ;
#514 = CARTESIAN_POINT ( 'NONE',  ( -61.35318038805866081, -2.627373316876406850, 0.4646149771581839505 ) ) ;
#515 = EDGE_CURVE ( 'NONE', #6742, #24689, #10204, .T. ) ;
#516 = ORIENTED_EDGE ( 'NONE', *, *, #10698, .T. ) ;
#517 = CARTESIAN_POINT ( 'NONE',  ( -67.32861504302871936, -2.100022785575387463, -0.05231372570481371970 ) ) ;
#518 = VERTEX_POINT ( 'NONE', #3495 ) ;
#519 = ORIENTED_EDGE ( 'NONE', *, *, #15693, .T. ) ;
#520 = CARTESIAN_POINT ( 'NONE',  ( 15.03925126672132784, 5.377732432866634937, 0.5657657256216264141 ) ) ;
#521 = ORIENTED_EDGE ( 'NONE', *, *, #12297, .F. ) ;
#522 = SURFACE_STYLE_USAGE ( .BOTH. , #27114 ) ;
#523 = AXIS2_PLACEMENT_3D ( 'NONE', #6717, #4335, #11637 ) ;
#524 = DIRECTION ( 'NONE',  ( -4.117859380279907901E-15, -0.9495137264943731559, -0.3137254901960768172 ) ) ;
#525 = CARTESIAN_POINT ( 'NONE',  ( -58.94702994616203284, -2.078460969082631227, -3.600000000000215472 ) ) ;
#526 = ORIENTED_EDGE ( 'NONE', *, *, #3756, .F. ) ;
#527 = CARTESIAN_POINT ( 'NONE',  ( -56.49999999999997868, 2.944486372867090029, 1.699999999999814548 ) ) ;
#528 = DIRECTION ( 'NONE',  ( 0.000000000000000000, 0.000000000000000000, 1.000000000000000000 ) ) ;
#529 = EDGE_CURVE ( 'NONE', #10936, #30188, #15204, .T. ) ;
#530 = CARTESIAN_POINT ( 'NONE',  ( 22.41225425283438355, 6.886225701514022468, 2.050000000000119726 ) ) ;
#531 = ORIENTED_EDGE ( 'NONE', *, *, #17069, .T. ) ;
#532 = CARTESIAN_POINT ( 'NONE',  ( -44.59999999999999432, -1.400000000000006795, 3.959797974644484242 ) ) ;
#533 = EDGE_CURVE ( 'NONE', #27746, #12623, #23876, .T. ) ;
#534 = CARTESIAN_POINT ( 'NONE',  ( -54.49608498031047787, -1.530604779201329091, 4.051096982736678953 ) ) ;
#535 = CARTESIAN_POINT ( 'NONE',  ( 61.25000000000004263, -1.960427193528290424, -0.3958853607747112036 ) ) ;
#536 = DIRECTION ( 'NONE',  ( 0.000000000000000000, 0.000000000000000000, 1.000000000000000000 ) ) ;
#537 = DIRECTION ( 'NONE',  ( 0.000000000000000000, 0.000000000000000000, -1.000000000000000000 ) ) ;
#539 = DIRECTION ( 'NONE',  ( 1.000000000000000000, 0.000000000000000000, 0.000000000000000000 ) ) ;
#538 = FACE_OUTER_BOUND ( 'NONE', #16964, .T. ) ;
#540 = EDGE_CURVE ( 'NONE', #20985, #4962, #20292, .T. ) ;
#541 = EDGE_CURVE ( 'NONE', #13128, #21850, #16800, .T. ) ;
#542 = AXIS2_PLACEMENT_3D ( 'NONE', #25219, #6797, #30869 ) ;
#543 = DIRECTION ( 'NONE',  ( 1.000000000000000000, 1.047444401652940007E-14, 0.000000000000000000 ) ) ;
#544 = FACE_BOUND ( 'NONE', #24096, .T. ) ;
#545 = CARTESIAN_POINT ( 'NONE',  ( 58.72427158855708029, 1.293556822995456823, -1.357477749119827104 ) ) ;
#546 = FACE_OUTER_BOUND ( 'NONE', #69, .T. ) ;
#547 = ORIENTED_EDGE ( 'NONE', *, *, #28384, .F. ) ;
#548 = ORIENTED_EDGE ( 'NONE', *, *, #30878, .F. ) ;
#549 = SHAPE_REPRESENTATION ( 'Pocket Clip', ( #9018 ), #22713 ) ;
#550 = ORIENTED_EDGE ( 'NONE', *, *, #4785, .F. ) ;
#551 = DIRECTION ( 'NONE',  ( 1.000000000000000000, 3.054025858079668409E-16, -2.042474015755241579E-16 ) ) ;
#552 = CARTESIAN_POINT ( 'NONE',  ( -60.67292740578359656, -3.330682475591783653, -0.6830477631804101613 ) ) ;
#554 = FACE_OUTER_BOUND ( 'NONE', #22689, .T. ) ;
#553 = FACE_OUTER_BOUND ( 'NONE', #21182, .T. ) ;
#555 = EDGE_LOOP ( 'NONE', ( #4647, #4798, #8077, #13774 ) ) ;
#556 = VERTEX_POINT ( 'NONE', #12979 ) ;
#557 = CARTESIAN_POINT ( 'NONE',  ( 51.30885344615025190, -4.380199991373268986, -1.408811060053339226 ) ) ;
#558 = EDGE_LOOP ( 'NONE', ( #6600, #18904, #20461, #4910 ) ) ;
#559 = DIRECTION ( 'NONE',  ( 1.000000000000000000, -1.219044193948983948E-29, 3.491481338843133355E-15 ) ) ;
#560 = VERTEX_POINT ( 'NONE', #22668 ) ;
#561 = CARTESIAN_POINT ( 'NONE',  ( 26.91641317417821000, 5.349067879199080444, -2.050000000000093969 ) ) ;
#562 = ORIENTED_EDGE ( 'NONE', *, *, #8648, .F. ) ;
#563 = CARTESIAN_POINT ( 'NONE',  ( -58.43749999999997158, 0.7533615035078148336, -3.673546848079175309 ) ) ;
#564 = ADVANCED_FACE ( 'NONE', ( #964, #8232 ), #9016, .T. ) ;
#565 = CARTESIAN_POINT ( 'NONE',  ( -71.49999999999998579, -1.395601618875910821E-15, 2.917180974979867506E-15 ) ) ;
#566 = EDGE_CURVE ( 'NONE', #9993, #18673, #27716, .T. ) ;
#567 = CARTESIAN_POINT ( 'NONE',  ( 15.22780280894113325, -4.861582133260076155, -2.394243994562784916 ) ) ;
#568 = EDGE_CURVE ( 'NONE', #19552, #25905, #3138, .T. ) ;
#569 = CARTESIAN_POINT ( 'NONE',  ( -59.94702994616205416, -2.078460969082657872, 3.599999999999778932 ) ) ;
#570 = CARTESIAN_POINT ( 'NONE',  ( 54.21471704787896329, 5.862036637490151136, -2.050000000000189004 ) ) ;
#571 = CARTESIAN_POINT ( 'NONE',  ( 47.49336422635084887, -3.991980709735058142, -1.294710393269184134 ) ) ;
#572 = DIRECTION ( 'NONE',  ( 0.000000000000000000, -1.000000000000000000, -4.336808689942015369E-15 ) ) ;
#573 = CARTESIAN_POINT ( 'NONE',  ( -44.49999999999997868, -1.500000000000000000, 3.300094695611020867 ) ) ;
#574 = DIRECTION ( 'NONE',  ( 0.000000000000000000, -1.154631945610163433E-14, 1.000000000000000000 ) ) ;
#575 = DIRECTION ( 'NONE',  ( 1.000000000000000000, 1.047444401652940007E-14, 0.000000000000000000 ) ) ;
#576 = CARTESIAN_POINT ( 'NONE',  ( -59.67987798884427519, 2.349476376206463879, -1.226921160904890451 ) ) ;
#577 = CIRCLE ( 'NONE', #19806, 3.624999999999996447 ) ;
#578 = DIRECTION ( 'NONE',  ( 3.491481338843133355E-15, -0.000000000000000000, 1.000000000000000000 ) ) ;
#579 = ORIENTED_EDGE ( 'NONE', *, *, #7, .T. ) ;
#580 = CARTESIAN_POINT ( 'NONE',  ( -61.34999999999997300, -2.577403337407089712, -0.5873456857003641618 ) ) ;
#581 = CARTESIAN_POINT ( 'NONE',  ( -36.30347965937272647, -3.148602930107041065, -4.139959549308994902 ) ) ;
#582 = CARTESIAN_POINT ( 'NONE',  ( 54.19695643086576808, 6.698469119960920537, 2.049999999999810640 ) ) ;
#583 = EDGE_LOOP ( 'NONE', ( #2042, #21747, #12985, #11896, #10364, #14795, #4740, #15981, #29108, #15326 ) ) ;
#584 = CARTESIAN_POINT ( 'NONE',  ( 65.00000000000001421, -1.025519176787267142E-28, -6.808388610744108654E-13 ) ) ;
#585 = VERTEX_POINT ( 'NONE', #11859 ) ;
#586 = CARTESIAN_POINT ( 'NONE',  ( 52.61915120152465875, 4.492597126270361230, 1.565330858589529806 ) ) ;
#587 = CARTESIAN_POINT ( 'NONE',  ( -54.97085481156724285, 2.489203624310592833, -2.804704140674919799 ) ) ;
#589 = CARTESIAN_POINT ( 'NONE',  ( 51.23644008536124517, -1.080112125195908490, -1.214076932077872817 ) ) ;
#588 = CARTESIAN_POINT ( 'NONE',  ( 51.25960411873057154, -4.349885043120370831, 1.496908008647323207 ) ) ;
#590 = VERTEX_POINT ( 'NONE', #30867 ) ;
#591 = LINE ( 'NONE', #5506, #15902 ) ;
#592 = DIRECTION ( 'NONE',  ( 1.000000000000000000, -0.000000000000000000, -1.047444401652940007E-14 ) ) ;
#593 = CIRCLE ( 'NONE', #14742, 0.09999999999999990841 ) ;
#595 = CARTESIAN_POINT ( 'NONE',  ( 58.75000000000002132, 6.153735859711025284E-13, 3.111507638930570854E-58 ) ) ;
#594 = CARTESIAN_POINT ( 'NONE',  ( 52.84329436925435886, 4.147588588921422570, 2.046816584343155387 ) ) ;
#596 = VERTEX_POINT ( 'NONE', #23754 ) ;
#597 = CARTESIAN_POINT ( 'NONE',  ( -57.81249999999997158, -3.238593381231840596, -2.874284765127020691 ) ) ;
#598 = CARTESIAN_POINT ( 'NONE',  ( 56.95000000000001705, -0.6820512820512819596, 1.773360101234998210 ) ) ;
#599 = ADVANCED_FACE ( 'NONE', ( #18369 ), #26110, .T. ) ;
#600 = CARTESIAN_POINT ( 'NONE',  ( 58.50000000000001421, 0.000000000000000000, 0.000000000000000000 ) ) ;
#601 = AXIS2_PLACEMENT_3D ( 'NONE', #25474, #29769, #15523 ) ;
#602 = EDGE_CURVE ( 'NONE', #9917, #10580, #19823, .T. ) ;
#603 = CIRCLE ( 'NONE', #61, 4.700000000000000178 ) ;
#604 = LINE ( 'NONE', #19783, #5091 ) ;
#605 = CARTESIAN_POINT ( 'NONE',  ( 48.40000000000001990, 2.428612866367529932E-14, 0.000000000000000000 ) ) ;
#606 = CARTESIAN_POINT ( 'NONE',  ( 52.06628335902946247, -0.5434431642975662280, -1.718465885608440713 ) ) ;
#607 = ORIENTED_EDGE ( 'NONE', *, *, #22678, .F. ) ;
#608 = CARTESIAN_POINT ( 'NONE',  ( 16.07279755198631932, 2.910597594660116805, 4.559461819278099348 ) ) ;
#609 = DIRECTION ( 'NONE',  ( 1.000000000000000000, 0.000000000000000000, -3.491481338843133750E-15 ) ) ;
#610 = EDGE_CURVE ( 'NONE', #737, #19244, #24862, .T. ) ;
#611 = B_SPLINE_CURVE_WITH_KNOTS ( 'NONE', 3,
 ( #22873, #22726, #25234, #10817, #1022, #20026, #10673, #13190, #29668, #29978, #1162, #27768, #14940, #12569, #5615, #22258, #19870, #29499, #7815 ),
 .UNSPECIFIED., .F., .F.,
 ( 4, 3, 3, 3, 3, 3, 4 ),
 ( 0.000000000000000000, 1.485152479261659526E-05, 2.963899638137937738E-05, 4.531421101975830796E-05, 6.339282692920775891E-05, 8.412900350910317146E-05, 8.561427748423838346E-05 ),
 .UNSPECIFIED. ) ;
#612 = LINE ( 'NONE', #20579, #31143 ) ;
#613 = CARTESIAN_POINT ( 'NONE',  ( -36.38012252111234091, 4.735538777079434603, -2.618062770414225859 ) ) ;
#614 = CARTESIAN_POINT ( 'NONE',  ( -57.77499999999997016, 2.796048871338436190E-15, 1.138853883557972617E-16 ) ) ;
#615 = CARTESIAN_POINT ( 'NONE',  ( 25.07992259980452943, 5.430687345545501366, 2.049999999999912781 ) ) ;
#616 = VERTEX_POINT ( 'NONE', #13744 ) ;
#617 = FACE_OUTER_BOUND ( 'NONE', #26372, .T. ) ;
#618 = VERTEX_POINT ( 'NONE', #31015 ) ;
#619 = UNCERTAINTY_MEASURE_WITH_UNIT (LENGTH_MEASURE( 1.000000000000000082E-05 ), #17870, 'distance_accuracy_value', 'NONE');
#620 = CARTESIAN_POINT ( 'NONE',  ( 58.75000000000002132, 6.153735859711025284E-13, 3.111507638930570854E-58 ) ) ;
#621 = PRODUCT_RELATED_PRODUCT_CATEGORY ( 'part', '', ( #20207 ) ) ;
#623 = DIRECTION ( 'NONE',  ( -1.000000000000000000, -2.586136946169074517E-16, 0.000000000000000000 ) ) ;
#622 = DIRECTION ( 'NONE',  ( 0.000000000000000000, 0.2745098039215694841, -0.9615843008030765526 ) ) ;
#624 = VERTEX_POINT ( 'NONE', #28172 ) ;
#625 = ORIENTED_EDGE ( 'NONE', *, *, #7840, .T. ) ;
#626 = CARTESIAN_POINT ( 'NONE',  ( -73.89999999999997726, 0.03361945752964275169, -1.349581317326006946 ) ) ;
#627 = CYLINDRICAL_SURFACE ( 'NONE', #1476, 2.000000000000000000 ) ;
#628 = ORIENTED_EDGE ( 'NONE', *, *, #25092, .T. ) ;
#630 = LINE ( 'NONE', #9997, #12984 ) ;
#629 = CARTESIAN_POINT ( 'NONE',  ( -59.07202994616203995, -4.156921938165296204, -2.246292432604653256E-13 ) ) ;
#631 = DIRECTION ( 'NONE',  ( 0.000000000000000000, 0.000000000000000000, 1.000000000000000000 ) ) ;
#632 = AXIS2_PLACEMENT_3D ( 'NONE', #9663, #16780, #24048 ) ;
#633 = CARTESIAN_POINT ( 'NONE',  ( -36.56390771145526486, -5.076023720898236391, -1.868859051106839475 ) ) ;
#634 = PRODUCT_CONTEXT ( 'NONE', #15616, 'mechanical' ) ;
#635 = EDGE_CURVE ( 'NONE', #25117, #29888, #25505, .T. ) ;
#636 = CARTESIAN_POINT ( 'NONE',  ( -61.34999999999997300, -2.603451079269508917, 0.4582852780074869736 ) ) ;
#637 = SHAPE_REPRESENTATION_RELATIONSHIP ( 'NONE' , 'NONE' ,  #27890, #14241 ) ;
#638 = B_SPLINE_CURVE_WITH_KNOTS ( 'NONE', 3,
 ( #156, #24228, #5203, #14564 ),
 .UNSPECIFIED., .F., .F.,
 ( 4, 4 ),
 ( 0.000000000000000000, 0.0001000467755295619533 ),
 .UNSPECIFIED. ) ;
#639 = ORIENTED_EDGE ( 'NONE', *, *, #7228, .F. ) ;
#640 = CARTESIAN_POINT ( 'NONE',  ( -59.07202994616203995, -4.156921938165296204, -2.246292432604653256E-13 ) ) ;
#641 = DIRECTION ( 'NONE',  ( 0.000000000000000000, 1.000000000000000000, 0.000000000000000000 ) ) ;
#642 = CARTESIAN_POINT ( 'NONE',  ( -56.58155989232411542, -1.962990915244702483, -3.400000000000209077 ) ) ;
#643 = CARTESIAN_POINT ( 'NONE',  ( 15.45522337368519850, -0.1928884786867813006, 5.200000000471195705 ) ) ;
#644 = CARTESIAN_POINT ( 'NONE',  ( 50.93273774044249791, -4.031600731908414836, 1.173113608511496153 ) ) ;
#645 = CARTESIAN_POINT ( 'NONE',  ( -56.89405989232413674, -6.418945959278930492E-15, 3.399999999999796962 ) ) ;
#646 = EDGE_CURVE ( 'NONE', #4290, #26664, #11219, .T. ) ;
#648 = CARTESIAN_POINT ( 'NONE',  ( -61.34999999999997300, -2.533482711517546893, -0.7936709607354018869 ) ) ;
#647 = CARTESIAN_POINT ( 'NONE',  ( 23.27131915274573615, 6.595123925190214287, -1.425000000000080869 ) ) ;
#649 = CIRCLE ( 'NONE', #30477, 4.300000000000019362 ) ;
#650 = DIRECTION ( 'NONE',  ( 0.000000000000000000, -0.000000000000000000, -1.000000000000000000 ) ) ;
#651 = CARTESIAN_POINT ( 'NONE',  ( 15.97944027357901753, -3.614202567155989421, 4.024415706308047014 ) ) ;
#653 = FACE_OUTER_BOUND ( 'NONE', #21981, .T. ) ;
#652 = CARTESIAN_POINT ( 'NONE',  ( 15.76675455518219238, 5.110933801299809787, -1.769007076671054390 ) ) ;
#654 = EDGE_LOOP ( 'NONE', ( #9080, #23435, #20814, #9552 ) ) ;
#655 = CARTESIAN_POINT ( 'NONE',  ( 50.42106458229518751, -0.9199776782966014865, -3.998258245321812510 ) ) ;
#656 = CARTESIAN_POINT ( 'NONE',  ( -35.85663232820583346, -4.683225679163351529, -2.703237727951242952 ) ) ;
#658 = CARTESIAN_POINT ( 'NONE',  ( 51.70000000000001705, 3.851905453475298113, -1.404572667215154835 ) ) ;
#657 = CARTESIAN_POINT ( 'NONE',  ( 15.44631504820162426, 2.881190829692330979, -4.334245811858005837 ) ) ;
#659 = CARTESIAN_POINT ( 'NONE',  ( 47.86824454757851299, -4.417905783403702991, 1.285520530454691057 ) ) ;
#660 = ORIENTED_EDGE ( 'NONE', *, *, #4616, .F. ) ;
#661 = CARTESIAN_POINT ( 'NONE',  ( -61.39708522154533199, -2.653109165506343903, 0.5005920380465845865 ) ) ;
#662 = DIRECTION ( 'NONE',  ( -1.000000000000000000, 0.000000000000000000, 1.047444401652940007E-14 ) ) ;
#663 = ORIENTED_EDGE ( 'NONE', *, *, #21235, .F. ) ;
#664 = DIRECTION ( 'NONE',  ( 1.000000000000000000, -1.219044193948983948E-29, 3.491481338843133355E-15 ) ) ;
#665 = ORIENTED_EDGE ( 'NONE', *, *, #19945, .T. ) ;
#666 = ORIENTED_EDGE ( 'NONE', *, *, #5798, .T. ) ;
#667 = CARTESIAN_POINT ( 'NONE',  ( 67.95000000000005969, -1.025519176787267142E-28, 4.049999999999288391 ) ) ;
#668 = ORIENTED_EDGE ( 'NONE', *, *, #22922, .F. ) ;
#669 = CARTESIAN_POINT ( 'NONE',  ( 34.41826917700200994, 8.206708519135760938, 1.949999999999880274 ) ) ;
#670 = EDGE_CURVE ( 'NONE', #23530, #30383, #28927, .T. ) ;
#671 = CARTESIAN_POINT ( 'NONE',  ( -59.69702994616202574, -2.078460969082631227, -3.600000000000218137 ) ) ;
#672 = ORIENTED_EDGE ( 'NONE', *, *, #29291, .F. ) ;
#673 = DIRECTION ( 'NONE',  ( 1.000000000000000000, 0.000000000000000000, -3.491481338843133355E-15 ) ) ;
#674 = ORIENTED_EDGE ( 'NONE', *, *, #25991, .F. ) ;
#675 = VECTOR ( 'NONE', #28976, 1000.000000000000000 ) ;
#676 = DIRECTION ( 'NONE',  ( 3.491481338843133355E-15, 3.491481338843133355E-15, -1.000000000000000000 ) ) ;
#677 = EDGE_CURVE ( 'NONE', #30092, #3236, #13549, .T. ) ;
#678 = CIRCLE ( 'NONE', #10773, 1.850000000000000089 ) ;
#679 = DIRECTION ( 'NONE',  ( 1.000000000000000000, 0.000000000000000000, -1.047444401652940007E-14 ) ) ;
#680 = ORIENTED_EDGE ( 'NONE', *, *, #27825, .F. ) ;
#681 = PLANE ( 'NONE',  #3139 ) ;
#682 = DIRECTION ( 'NONE',  ( 3.491481338843133355E-15, 3.491481338843133355E-15, -1.000000000000000000 ) ) ;
#683 = CARTESIAN_POINT ( 'NONE',  ( -54.39999999999996305, 1.500000000000021538, -3.363870538531680054 ) ) ;
#684 = FACE_OUTER_BOUND ( 'NONE', #441, .T. ) ;
#685 = CARTESIAN_POINT ( 'NONE',  ( -67.32861504302871936, -4.287230892216076523E-16, 3.265676834553754426E-15 ) ) ;
#686 = EDGE_CURVE ( 'NONE', #24297, #29070, #5670, .T. ) ;
#688 = CARTESIAN_POINT ( 'NONE',  ( 15.03925126672133139, -4.945493884734801782, 1.606888370749709027 ) ) ;
#687 = CARTESIAN_POINT ( 'NONE',  ( -36.48821680285185209, -3.495540671458102988, 4.131527132740904662 ) ) ;
#689 = CARTESIAN_POINT ( 'NONE',  ( 50.40000000000001990, 2.428612866367529932E-14, 0.000000000000000000 ) ) ;
#690 = DIRECTION ( 'NONE',  ( -1.000000000000000000, 0.000000000000000000, 1.047444401652940007E-14 ) ) ;
#691 = FACE_OUTER_BOUND ( 'NONE', #7612, .T. ) ;
#692 = CARTESIAN_POINT ( 'NONE',  ( -60.54999999999995453, 1.948556695721332102E-15, 6.806719277278738347E-16 ) ) ;
#693 = AXIS2_PLACEMENT_3D ( 'NONE', #28518, #6823, #16487 ) ;
#694 = EDGE_LOOP ( 'NONE', ( #11145, #17669, #9882, #6922 ) ) ;
#695 = CARTESIAN_POINT ( 'NONE',  ( 52.20711756518983293, 0.5000000000005468959, 1.807104036850122109 ) ) ;
#696 = ADVANCED_FACE ( 'NONE', ( #29416 ), #18309, .T. ) ;
#697 = ORIENTED_EDGE ( 'NONE', *, *, #22187, .T. ) ;
#698 = ORIENTED_EDGE ( 'NONE', *, *, #22851, .F. ) ;
#699 = CARTESIAN_POINT ( 'NONE',  ( -54.44999999999997442, 1.499999999999999556, -4.029888335921975262 ) ) ;
#700 = CARTESIAN_POINT ( 'NONE',  ( -60.79792740578359656, -2.256877952708263635, 2.542931754211925188 ) ) ;
#702 = CARTESIAN_POINT ( 'NONE',  ( -61.38483210406819524, -2.605333280927485173, 0.7010916910920483858 ) ) ;
#701 = CARTESIAN_POINT ( 'NONE',  ( 15.59140265158955074, 4.755985070912251977, 2.573747172434746933 ) ) ;
#703 = ORIENTED_EDGE ( 'NONE', *, *, #18963, .T. ) ;
#704 = VERTEX_POINT ( 'NONE', #19468 ) ;
#705 = CARTESIAN_POINT ( 'NONE',  ( 53.91566580141704890, 6.672244292255800069, -1.816235364411796116 ) ) ;
#706 = ORIENTED_EDGE ( 'NONE', *, *, #12889, .T. ) ;
#707 = DIRECTION ( 'NONE',  ( 3.002035892788117952E-16, -0.9996898646859344595, -0.02490330187381124133 ) ) ;
#708 = EDGE_CURVE ( 'NONE', #25469, #23625, #14965, .T. ) ;
#709 = VERTEX_POINT ( 'NONE', #15006 ) ;
#710 = CARTESIAN_POINT ( 'NONE',  ( 25.99900894223747017, 5.212247164669804533, -2.050000000000091305 ) ) ;
#711 = EDGE_CURVE ( 'NONE', #13242, #19150, #227, .T. ) ;
#712 = DIRECTION ( 'NONE',  ( 1.000000000000000000, -0.000000000000000000, -3.491481338843133355E-15 ) ) ;
#713 = EDGE_CURVE ( 'NONE', #19668, #15709, #16819, .T. ) ;
#714 = CARTESIAN_POINT ( 'NONE',  ( 47.53097527630302466, -3.881932310064107217, 1.329369065054880394 ) ) ;
#715 = CARTESIAN_POINT ( 'NONE',  ( 15.44259799936802047, -4.878092280899799071, -1.814329181850236727 ) ) ;
#717 = CARTESIAN_POINT ( 'NONE',  ( -60.20655989232410832, 1.962990915244748891, -3.400000000000205969 ) ) ;
#716 = AXIS2_PLACEMENT_3D ( 'NONE', #28481, #23120, #1884 ) ;
#718 = CARTESIAN_POINT ( 'NONE',  ( 54.12895949791516159, 5.523355893849346110, -2.050000000000188560 ) ) ;
#719 = B_SPLINE_CURVE_WITH_KNOTS ( 'NONE', 3,
 ( #22326, #2999, #17256, #24068, #2383, #12047, #21722, #16951, #26898, #14858, #7446, #7736, #15 ),
 .UNSPECIFIED., .F., .F.,
 ( 4, 3, 3, 3, 4 ),
 ( 0.000000000000000000, 4.969793434219683530E-05, 9.932084631989379544E-05, 0.0001499488332825447262, 0.0001857305951747128983 ),
 .UNSPECIFIED. ) ;
#720 = CARTESIAN_POINT ( 'NONE',  ( 47.38545878925128818, -3.877603133524967660, -1.337216932410631554 ) ) ;
#721 = DIRECTION ( 'NONE',  ( 0.000000000000000000, -1.000000000000000000, -3.491481338843137694E-15 ) ) ;
#722 = DIRECTION ( 'NONE',  ( -1.000000000000000000, -0.000000000000000000, -0.000000000000000000 ) ) ;
#723 = LINE ( 'NONE', #10382, #22147 ) ;
#724 = AXIS2_PLACEMENT_3D ( 'NONE', #17106, #455, #19785 ) ;
#725 = CARTESIAN_POINT ( 'NONE',  ( -59.13207863537445519, -2.357771006092566513, 1.210922106982256663 ) ) ;
#726 = LINE ( 'NONE', #12044, #17578 ) ;
#727 =( BOUNDED_SURFACE ( )  B_SPLINE_SURFACE ( 3, 2, ( 
 ( #12834, #20466, #5581 ),
 ( #10487, #25026, #12537 ),
 ( #20162, #17300, #5726 ),
 ( #27562, #24567, #15231 ),
 ( #22842, #24876, #22516 ),
 ( #10317, #17450, #27263 ),
 ( #26944, #29627, #819 ),
 ( #5891, #1131, #29792 ),
 ( #7953, #13008, #10783 ),
 ( #3357, #17618, #24731 ),
 ( #2886, #5252, #13156 ),
 ( #3192, #8255, #657 ),
 ( #8106, #3044, #22692 ),
 ( #5419, #22223, #510 ),
 ( #12687, #17775, #987 ),
 ( #10167, #27416, #17922 ) ),
 .UNSPECIFIED., .F., .F., .F. ) 
 B_SPLINE_SURFACE_WITH_KNOTS ( ( 4, 2, 2, 2, 2, 2, 2, 4 ),
 ( 3, 3 ),
 ( 0.001780502285214198826, 0.002558945925323778507, 0.002753556835351173536, 0.002948167745378568131, 0.003337389565433357755, 0.003726611385488147379, 0.004115833205542937002, 0.004894276845652516250 ),
 ( 0.000000000000000000, 1.000000000000000000 ),
 .UNSPECIFIED. ) 
 GEOMETRIC_REPRESENTATION_ITEM ( )  RATIONAL_B_SPLINE_SURFACE ( (
 ( 1.000000000000000000, 0.9418517008537241608, 1.000000000000000000),
 ( 1.000000000000000000, 0.9417987965884988544, 1.000000000000000000),
 ( 1.000000000000000000, 0.9418198861734230487, 1.000000000000000000),
 ( 1.000000000000000000, 0.9434060303845539508, 1.000000000000000000),
 ( 1.000000000000000000, 0.9437939819948095721, 1.000000000000000000),
 ( 1.000000000000000000, 0.9445989566712880148, 1.000000000000000000),
 ( 1.000000000000000000, 0.9450169930049983069, 1.000000000000000000),
 ( 1.000000000000000000, 0.9461610507673332560, 1.000000000000000000),
 ( 1.000000000000000000, 0.9467217966427213804, 1.000000000000000000),
 ( 1.000000000000000000, 0.9467345476124363612, 1.000000000000000000),
 ( 1.000000000000000000, 0.9461964028052722853, 1.000000000000000000),
 ( 1.000000000000000000, 0.9446801822474062416, 1.000000000000000000),
 ( 1.000000000000000000, 0.9437582546536901207, 1.000000000000000000),
 ( 1.000000000000000000, 0.9418129560294949965, 1.000000000000000000),
 ( 1.000000000000000000, 0.9418016889778024758, 1.000000000000000000),
 ( 1.000000000000000000, 0.9418517008537236057, 1.000000000000000000) ) ) 
 REPRESENTATION_ITEM ( '' )  SURFACE ( )  );
#728 = CARTESIAN_POINT ( 'NONE',  ( 50.87477060347373481, 8.633605004118187765, -2.050000000000176570 ) ) ;
#729 = ORIENTED_EDGE ( 'NONE', *, *, #12353, .T. ) ;
#730 = VECTOR ( 'NONE', #6705, 1000.000000000000000 ) ;
#731 = ADVANCED_FACE ( 'NONE', ( #7124 ), #21860, .F. ) ;
#732 = CARTESIAN_POINT ( 'NONE',  ( -59.29999999999995453, 0.8061685447651361081, 3.512174729956796249 ) ) ;
#733 = CARTESIAN_POINT ( 'NONE',  ( -36.26369610968621515, -2.881190829692320321, -4.334245811858070674 ) ) ;
#734 = CARTESIAN_POINT ( 'NONE',  ( 54.37322678328315106, 5.989334493575450225, 2.026383240762962057 ) ) ;
#735 = ORIENTED_EDGE ( 'NONE', *, *, #357, .T. ) ;
#736 = DIRECTION ( 'NONE',  ( 0.000000000000000000, -0.9119702176296791141, -0.4102564102564098536 ) ) ;
#737 = VERTEX_POINT ( 'NONE', #5196 ) ;
#738 = EDGE_CURVE ( 'NONE', #5843, #8754, #4762, .T. ) ;
#739 = CARTESIAN_POINT ( 'NONE',  ( 15.30042582489635095, -1.123735543663344938, -5.289358694936611371 ) ) ;
#740 = AXIS2_PLACEMENT_3D ( 'NONE', #8039, #24813, #27350 ) ;
#741 = CARTESIAN_POINT ( 'NONE',  ( -55.09585481156724285, -1.184343223768585807, -3.558065644182726306 ) ) ;
#743 = CARTESIAN_POINT ( 'NONE',  ( 51.58885679141839375, -3.753732476607584800, -1.652583012570544074 ) ) ;
#742 = CARTESIAN_POINT ( 'NONE',  ( 51.59056972799722018, -4.226153977860459321, 1.819915812912550335 ) ) ;
#744 = EDGE_LOOP ( 'NONE', ( #9293, #4130, #2550, #9244, #30717, #18089, #30568, #28296 ) ) ;
#745 = DIRECTION ( 'NONE',  ( 0.000000000000000000, 0.000000000000000000, -1.000000000000000000 ) ) ;
#746 = DIRECTION ( 'NONE',  ( 0.000000000000000000, 0.000000000000000000, -1.000000000000000000 ) ) ;
#747 = ORIENTED_EDGE ( 'NONE', *, *, #9238, .F. ) ;
#749 = DIRECTION ( 'NONE',  ( -1.000000000000000000, -2.586136946169074517E-16, 0.000000000000000000 ) ) ;
#748 = CARTESIAN_POINT ( 'NONE',  ( 52.07305031865988809, 3.932152079777906817, 2.045338552409953881 ) ) ;
#750 = AXIS2_PLACEMENT_3D ( 'NONE', #11893, #21738, #11742 ) ;
#751 = CARTESIAN_POINT ( 'NONE',  ( -44.49999999999997868, 0.000000000000000000, 0.000000000000000000 ) ) ;
#752 = ORIENTED_EDGE ( 'NONE', *, *, #11276, .F. ) ;
#753 = CARTESIAN_POINT ( 'NONE',  ( -58.56249999999997158, -3.238593381231840596, -2.874284765127020691 ) ) ;
#754 = CARTESIAN_POINT ( 'NONE',  ( 56.97512559646294505, -0.7466375667864569854, 1.747149777169433094 ) ) ;
#755 = CARTESIAN_POINT ( 'NONE',  ( 58.74999981404332061, 1.649595783783479375, -1.050697058760609037 ) ) ;
#756 = DIRECTION ( 'NONE',  ( -0.000000000000000000, -0.000000000000000000, 1.000000000000000000 ) ) ;
#757 = CARTESIAN_POINT ( 'NONE',  ( 68.00000000000001421, 1.401298464324817071E-42, -7.122621931239992550E-13 ) ) ;
#758 = CARTESIAN_POINT ( 'NONE',  ( -55.19702994616203284, -2.078460969082631227, -3.600000000000202593 ) ) ;
#759 = CARTESIAN_POINT ( 'NONE',  ( 15.59055531549694074, 0.9785522574022036402, 5.318456145981286909 ) ) ;
#761 = ORIENTED_EDGE ( 'NONE', *, *, #2889, .F. ) ;
#760 = AXIS2_PLACEMENT_3D ( 'NONE', #23917, #2210, #11875 ) ;
#762 = CARTESIAN_POINT ( 'NONE',  ( -61.34999999999997300, -2.456456838093036055, -0.5843327841101846332 ) ) ;
#763 = VECTOR ( 'NONE', #13667, 1000.000000000000114 ) ;
#764 = CARTESIAN_POINT ( 'NONE',  ( 50.25000000000001421, 0.5380862305914526633, -2.008165151417984351 ) ) ;
#765 = AXIS2_PLACEMENT_3D ( 'NONE', #16455, #26113, #4724 ) ;
#766 = DIRECTION ( 'NONE',  ( 0.7071067811865440200, -0.7068874824028898995, -0.01760929362890773994 ) ) ;
#767 = EDGE_CURVE ( 'NONE', #15338, #3096, #24468, .T. ) ;
#768 = CARTESIAN_POINT ( 'NONE',  ( -35.85663232820582635, 4.861582140531628404, -2.394243978978282783 ) ) ;
#769 = CARTESIAN_POINT ( 'NONE',  ( -35.85663232820581925, 0.4576450603546987073, 5.200000000000000178 ) ) ;
#770 = CARTESIAN_POINT ( 'NONE',  ( 48.44629147628577215, 1.309359793766484925, -3.864871860988134955 ) ) ;
#771 = EDGE_CURVE ( 'NONE', #11615, #8275, #12629, .T. ) ;
#772 = ORIENTED_EDGE ( 'NONE', *, *, #1502, .T. ) ;
#773 = DIRECTION ( 'NONE',  ( 0.000000000000000000, 0.000000000000000000, 1.000000000000000000 ) ) ;
#774 = ORIENTED_EDGE ( 'NONE', *, *, #19717, .T. ) ;
#775 = EDGE_CURVE ( 'NONE', #13383, #3831, #22467, .T. ) ;
#776 = DIRECTION ( 'NONE',  ( 1.000000000000000000, -0.000000000000000000, -1.047444401652940007E-14 ) ) ;
#778 = DIRECTION ( 'NONE',  ( -1.000000000000000000, -0.000000000000000000, -0.000000000000000000 ) ) ;
#777 = CARTESIAN_POINT ( 'NONE',  ( 15.03925126672133139, -4.018128179617529661, -3.618665901676669350 ) ) ;
#779 = VERTEX_POINT ( 'NONE', #24051 ) ;
#780 = CIRCLE ( 'NONE', #17971, 0.2000000000000000944 ) ;
#781 = ORIENTED_EDGE ( 'NONE', *, *, #15945, .F. ) ;
#782 = FACE_OUTER_BOUND ( 'NONE', #5822, .T. ) ;
#783 = VECTOR ( 'NONE', #2254, 1000.000000000000000 ) ;
#784 = CARTESIAN_POINT ( 'NONE',  ( -61.39999999999998437, 1.381785979968628826E-15, 2.054751023403646402E-15 ) ) ;
#785 = ORIENTED_EDGE ( 'NONE', *, *, #10926, .F. ) ;
#787 = CARTESIAN_POINT ( 'NONE',  ( 51.79804399563283823, -4.143014423056512463, 1.077153443819862000 ) ) ;
#786 = CARTESIAN_POINT ( 'NONE',  ( -59.63452994616203284, 2.093608279459373297E-14, -3.600000000000211475 ) ) ;
#788 = CARTESIAN_POINT ( 'NONE',  ( -54.73542740578361077, -3.725040285533364859, 1.239922660687674760 ) ) ;
#789 = CIRCLE ( 'NONE', #15973, 4.200000000000016165 ) ;
#790 = DIRECTION ( 'NONE',  ( 1.000000000000000000, 3.053848253006669023E-16, -2.042510438544995415E-16 ) ) ;
#791 = DIRECTION ( 'NONE',  ( 1.000000000000000000, 0.000000000000000000, 0.000000000000000000 ) ) ;
#792 = CIRCLE ( 'NONE', #10394, 0.05000000000000012768 ) ;
#794 = EDGE_CURVE ( 'NONE', #2131, #1323, #2362, .T. ) ;
#793 = B_SPLINE_CURVE_WITH_KNOTS ( 'NONE', 3,
 ( #2578, #2877, #7631, #19681 ),
 .UNSPECIFIED., .F., .F.,
 ( 4, 4 ),
 ( 0.0001543670095910078732, 0.0003084486524517373977 ),
 .UNSPECIFIED. ) ;
#795 = CARTESIAN_POINT ( 'NONE',  ( -59.29999999999999005, -2.918520965380715371, 1.872283793155697706 ) ) ;
#796 = AXIS2_PLACEMENT_3D ( 'NONE', #14846, #19782, #453 ) ;
#797 = B_SPLINE_CURVE_WITH_KNOTS ( 'NONE', 3,
 ( #20697, #30322, #12903, #18305 ),
 .UNSPECIFIED., .F., .F.,
 ( 4, 4 ),
 ( 0.000000000000000000, 0.0003819718307412704175 ),
 .UNSPECIFIED. ) ;
#798 = ORIENTED_EDGE ( 'NONE', *, *, #29211, .T. ) ;
#799 = DIRECTION ( 'NONE',  ( 1.000000000000000000, 0.000000000000000000, -1.047444401652940007E-14 ) ) ;
#800 = CARTESIAN_POINT ( 'NONE',  ( 53.90177594311669651, 7.547472342232321552, -2.050000000000187672 ) ) ;
#801 = DIRECTION ( 'NONE',  ( 1.000000000000000000, -1.219044193948983948E-29, 3.491481338843133355E-15 ) ) ;
#802 = AXIS2_PLACEMENT_3D ( 'NONE', #29576, #17728, #17572 ) ;
#803 = CIRCLE ( 'NONE', #9900, 0.1500000000000001887 ) ;
#804 = CARTESIAN_POINT ( 'NONE',  ( -67.32861504302871936, 2.100022785575386575, 0.05231372570482049900 ) ) ;
#806 = DIRECTION ( 'NONE',  ( 0.000000000000000000, 0.000000000000000000, 1.000000000000000000 ) ) ;
#805 = DIRECTION ( 'NONE',  ( 0.000000000000000000, 1.000000000000000000, 0.000000000000000000 ) ) ;
#807 = AXIS2_PLACEMENT_3D ( 'NONE', #26000, #20498, #30125 ) ;
#808 = DIRECTION ( 'NONE',  ( 1.000000000000000000, -0.000000000000000000, -1.047444401652940007E-14 ) ) ;
#809 = CARTESIAN_POINT ( 'NONE',  ( 58.50000000000001421, -0.8156862745098042433, 2.468735688885369317 ) ) ;
#810 = CIRCLE ( 'NONE', #6376, 1.975000000000001865 ) ;
#812 = CARTESIAN_POINT ( 'NONE',  ( -35.85663232820584057, 3.426725943139577790, -3.937891353488711221 ) ) ;
#811 = CARTESIAN_POINT ( 'NONE',  ( 51.87765138016309407, 8.698644590117595499, 2.049999999999819522 ) ) ;
#813 = EDGE_CURVE ( 'NONE', #21791, #9481, #23476, .T. ) ;
#814 = ORIENTED_EDGE ( 'NONE', *, *, #5611, .F. ) ;
#815 = CIRCLE ( 'NONE', #18531, 0.2999999999999999334 ) ;
#816 = CARTESIAN_POINT ( 'NONE',  ( 58.45000000000001705, 0.8000000000000002665, 2.421260002560650104 ) ) ;
#817 = EDGE_CURVE ( 'NONE', #4631, #20056, #25479, .T. ) ;
#818 = CARTESIAN_POINT ( 'NONE',  ( 19.23646557533807666, -5.338914163118011480, 0.000000000000000000 ) ) ;
#820 = CARTESIAN_POINT ( 'NONE',  ( 15.03925126672132961, -0.4576450603546909912, -5.200000000000000178 ) ) ;
#819 = CARTESIAN_POINT ( 'NONE',  ( 15.45522337368517007, 3.212533369474642075, -4.093511368021645502 ) ) ;
#821 = DIRECTION ( 'NONE',  ( 0.000000000000000000, 0.2008964009354147762, -0.9796124928211140670 ) ) ;
#822 = ORIENTED_EDGE ( 'NONE', *, *, #25663, .T. ) ;
#823 = CARTESIAN_POINT ( 'NONE',  ( 51.25000000000000711, 1.487500000000537836, 3.111507638930570854E-58 ) ) ;
#824 = DIRECTION ( 'NONE',  ( -1.000000000000000000, 0.000000000000000000, 1.047444401652940007E-14 ) ) ;
#825 = TOROIDAL_SURFACE ( 'NONE', #18539, 4.275000000000000355, 0.1000000000000000056 ) ;
#826 = VERTEX_POINT ( 'NONE', #15796 ) ;
#827 = CYLINDRICAL_SURFACE ( 'NONE', #3289, 4.300000000000016698 ) ;
#828 = ORIENTED_EDGE ( 'NONE', *, *, #31168, .F. ) ;
#829 = ORIENTED_EDGE ( 'NONE', *, *, #540, .T. ) ;
#830 = AXIS2_PLACEMENT_3D ( 'NONE', #10089, #14821, #7562 ) ;
#831 = CARTESIAN_POINT ( 'NONE',  ( 16.10660252424456118, 5.053896291911992300, -1.944420249220595087 ) ) ;
#832 = FACE_OUTER_BOUND ( 'NONE', #30522, .T. ) ;
#833 = VERTEX_POINT ( 'NONE', #5999 ) ;
#834 = CARTESIAN_POINT ( 'NONE',  ( 26.52792526470753387, 5.214288841967440469, 1.949999999999907585 ) ) ;
#835 = ADVANCED_FACE ( 'NONE', ( #6144 ), #29926, .F. ) ;
#836 = CARTESIAN_POINT ( 'NONE',  ( -59.25952994616205416, -4.643455692769875931E-15, 3.599999999999788702 ) ) ;
#837 = EDGE_LOOP ( 'NONE', ( #6700, #8690, #2350, #12267, #14721 ) ) ;
#838 = CIRCLE ( 'NONE', #28645, 0.05000000000000002359 ) ;
#839 = DIRECTION ( 'NONE',  ( 0.000000000000000000, 0.000000000000000000, 1.000000000000000000 ) ) ;
#840 = ORIENTED_EDGE ( 'NONE', *, *, #14681, .F. ) ;
#841 = CYLINDRICAL_SURFACE ( 'NONE', #1547, 0.1000000000000000472 ) ;
#842 = AXIS2_PLACEMENT_3D ( 'NONE', #30434, #23332, #18747 ) ;
#843 = CARTESIAN_POINT ( 'NONE',  ( 23.07431837327364832, 6.199584068344338839, 2.049999999999582379 ) ) ;
#844 = ORIENTED_EDGE ( 'NONE', *, *, #5546, .F. ) ;
#845 = CIRCLE ( 'NONE', #15996, 4.500000000000037303 ) ;
#846 = CARTESIAN_POINT ( 'NONE',  ( -54.68749999999998579, -3.925981830489445379, -2.085002746943179415E-13 ) ) ;
#847 = CIRCLE ( 'NONE', #15519, 0.1499999999999999667 ) ;
#848 = CARTESIAN_POINT ( 'NONE',  ( 58.75000000000001421, 0.5811678240991637878, -1.782657835994492013 ) ) ;
#849 = CYLINDRICAL_SURFACE ( 'NONE', #29409, 0.1499999999999999667 ) ;
#850 = CARTESIAN_POINT ( 'NONE',  ( 57.02888841125436414, -0.7778303923484506388, -1.733491207451775207 ) ) ;
#851 = EDGE_CURVE ( 'NONE', #22580, #19955, #11332, .T. ) ;
#852 = DIRECTION ( 'NONE',  ( 1.000000000000000000, 1.047444401652940007E-14, 0.000000000000000000 ) ) ;
#854 = CYLINDRICAL_SURFACE ( 'NONE', #8814, 0.09999999999999886757 ) ;
#853 = CARTESIAN_POINT ( 'NONE',  ( 50.50000000000002132, 2.478823385132571406E-14, 4.100000000000022737 ) ) ;
#855 = TOROIDAL_SURFACE ( 'NONE', #7439, 14.70000000000000995, 10.00000000000000000 ) ;
#856 = CIRCLE ( 'NONE', #8940, 4.849999999999999645 ) ;
#857 = CARTESIAN_POINT ( 'NONE',  ( 50.30000000000001847, -1.426739617975173013, -3.843750000000023093 ) ) ;
#858 = DIRECTION ( 'NONE',  ( 0.000000000000000000, 0.000000000000000000, 1.000000000000000000 ) ) ;
#859 = EDGE_CURVE ( 'NONE', #27662, #23750, #12840, .T. ) ;
#860 = B_SPLINE_CURVE_WITH_KNOTS ( 'NONE', 3,
 ( #900, #8173, #17841, #27478, #25267, #5795, #1051, #10702, #11800, #2291 ),
 .UNSPECIFIED., .F., .F.,
 ( 4, 3, 3, 4 ),
 ( 1.063942921725272085E-15, 0.0001291030634103491155, 0.0002330573485935334081, 0.0003370282537953245587 ),
 .UNSPECIFIED. ) ;
#861 = CARTESIAN_POINT ( 'NONE',  ( 58.75000000000000711, 1.469015551797813846, -1.320082690053157037 ) ) ;
#863 = CARTESIAN_POINT ( 'NONE',  ( 54.16616206058712635, 6.839261630856932506, -2.050000000000188560 ) ) ;
#862 = AXIS2_PLACEMENT_3D ( 'NONE', #23773, #6339, #16472 ) ;
#864 = EDGE_CURVE ( 'NONE', #2131, #12851, #29047, .T. ) ;
#865 = VERTEX_POINT ( 'NONE', #10878 ) ;
#866 = ADVANCED_FACE ( 'NONE', ( #1077 ), #1719, .T. ) ;
#867 = CARTESIAN_POINT ( 'NONE',  ( -54.49999999999997868, 1.549999999999999600, -4.064480286580312907 ) ) ;
#868 = CLOSED_SHELL ( 'NONE', ( #3607, #31285, #19814, #2896, #11313, #1933, #16606, #2566, #11194, #9119, #8437, #4942, #20881, #10226, #9824, #19849, #13450, #13335, #9869, #14567, #23249, #23818, #19671, #16010, #18689, #8050, #28313, #23742, #25301, #4603, #23913, #2405, #3250, #16375, #22683, #11024, #14689, #29311, #10151, #2320, #31083, #28868, #9802, #29845, #22522, #28501, #27572, #16956, #21743, #3102, #20819, #24145, #21081, #696, #22329, #7299, #2322, #17235, #15972, #26956, #25336, #8923, #24762, #17568 ) ) ;
#869 = CIRCLE ( 'NONE', #6936, 0.1500000000000001887 ) ;
#870 = ORIENTED_EDGE ( 'NONE', *, *, #20028, .T. ) ;
#871 = ORIENTED_EDGE ( 'NONE', *, *, #6348, .T. ) ;
#872 = CIRCLE ( 'NONE', #8460, 1.975000000000001865 ) ;
#873 = AXIS2_PLACEMENT_3D ( 'NONE', #4818, #30956, #16389 ) ;
#874 = CARTESIAN_POINT ( 'NONE',  ( -59.10095151589816709, 2.309095926083573502, 1.300228524717358836 ) ) ;
#875 = CARTESIAN_POINT ( 'NONE',  ( -59.04792740578360366, -1.073804522883517132, -3.225979517392335350 ) ) ;
#877 = LINE ( 'NONE', #29989, #14989 ) ;
#876 = CARTESIAN_POINT ( 'NONE',  ( -58.81249999999996447, 3.925981830489463142, -1.945260624050196617E-13 ) ) ;
#878 = ORIENTED_EDGE ( 'NONE', *, *, #12811, .F. ) ;
#879 = ORIENTED_EDGE ( 'NONE', *, *, #28610, .F. ) ;
#880 = CARTESIAN_POINT ( 'NONE',  ( 53.90436476239020180, 5.768992244161037952, -1.948923759896386665 ) ) ;
#881 = ORIENTED_EDGE ( 'NONE', *, *, #9302, .T. ) ;
#882 = CARTESIAN_POINT ( 'NONE',  ( 51.59739104186226655, 1.010292945603182391, -1.272765950230260179 ) ) ;
#883 = ADVANCED_FACE ( 'NONE', ( #20259, #26238, #4545, #26073, #16117, #21027 ), #30830, .T. ) ;
#884 = ORIENTED_EDGE ( 'NONE', *, *, #22321, .T. ) ;
#885 = CARTESIAN_POINT ( 'NONE',  ( 30.73039769179424141, 7.037486595895787289, -2.049999999999975842 ) ) ;
#886 = AXIS2_PLACEMENT_3D ( 'NONE', #30658, #14191, #19131 ) ;
#887 = CARTESIAN_POINT ( 'NONE',  ( -59.06249999999995737, -1.962990915244687828, -3.400000000000226841 ) ) ;
#888 = ORIENTED_EDGE ( 'NONE', *, *, #6577, .T. ) ;
#889 = AXIS2_PLACEMENT_3D ( 'NONE', #16006, #20779, #20468 ) ;
#890 = CARTESIAN_POINT ( 'NONE',  ( 15.03925126672133139, -5.086913985776139846, -1.171642053949128126 ) ) ;
#891 = CARTESIAN_POINT ( 'NONE',  ( -57.08155989232412963, 3.925981830489463142, -1.884825173204143128E-13 ) ) ;
#892 = ADVANCED_FACE ( 'NONE', ( #25917 ), #30664, .F. ) ;
#893 = CARTESIAN_POINT ( 'NONE',  ( 47.02489528704867894, -3.758556366959797668, 1.867213167016393394 ) ) ;
#894 = CARTESIAN_POINT ( 'NONE',  ( 47.20291695880406735, -3.814011388176768769, -1.508225752246980633 ) ) ;
#895 = CIRCLE ( 'NONE', #25653, 0.7500000000000186517 ) ;
#896 = CARTESIAN_POINT ( 'NONE',  ( -59.19976204860608959, -2.440481952758566830, 1.249999143831215687 ) ) ;
#897 = AXIS2_PLACEMENT_3D ( 'NONE', #25108, #28108, #8177 ) ;
#899 = TOROIDAL_SURFACE ( 'NONE', #1389, 1.824999999999999956, 0.05000000000000000278 ) ;
#898 = FACE_OUTER_BOUND ( 'NONE', #17661, .T. ) ;
#901 = FACE_OUTER_BOUND ( 'NONE', #12065, .T. ) ;
#900 = CARTESIAN_POINT ( 'NONE',  ( -59.41132486539680713, 3.361433066165957051, 1.250136525132557574 ) ) ;
#902 = FACE_OUTER_BOUND ( 'NONE', #1457, .T. ) ;
#903 = CARTESIAN_POINT ( 'NONE',  ( -35.85663232820583346, -4.383220986679503994, -0.4611378927914501769 ) ) ;
#904 = ADVANCED_FACE ( 'NONE', ( #16596 ), #23720, .F. ) ;
#905 = CARTESIAN_POINT ( 'NONE',  ( 58.45000000000001705, 0.8000000000000000444, -2.421260002560649660 ) ) ;
#906 = ADVANCED_FACE ( 'NONE', ( #23399 ), #24657, .F. ) ;
#907 = ORIENTED_EDGE ( 'NONE', *, *, #18125, .T. ) ;
#908 = AXIS2_PLACEMENT_3D ( 'NONE', #25148, #17875, #20268 ) ;
#909 = EDGE_CURVE ( 'NONE', #14419, #20284, #9225, .T. ) ;
#910 = CIRCLE ( 'NONE', #6467, 30.00000000000000000 ) ;
#911 = CARTESIAN_POINT ( 'NONE',  ( 50.56925576102500486, 0.1015751161705248512, 0.8011113709441619601 ) ) ;
#912 = CARTESIAN_POINT ( 'NONE',  ( 54.18857573620737611, 5.673640356790727424, 2.049999999999811529 ) ) ;
#913 = EDGE_LOOP ( 'NONE', ( #29372, #10833, #15778, #13748, #18804, #24361, #21663, #28963, #6278, #30255, #1776, #13627, #28648, #7508, #21353, #15239 ) ) ;
#914 = DIRECTION ( 'NONE',  ( -1.000000000000000000, 0.000000000000000000, 1.047444401652940007E-14 ) ) ;
#915 = ORIENTED_EDGE ( 'NONE', *, *, #13224, .F. ) ;
#916 = CARTESIAN_POINT ( 'NONE',  ( -54.49999999999999289, 1.399999999999998135, 3.363870538531246179 ) ) ;
#917 = CARTESIAN_POINT ( 'NONE',  ( 58.75000000000001421, 0.5380862305905714793, 2.008165151419250449 ) ) ;
#919 = CARTESIAN_POINT ( 'NONE',  ( 58.65000000000001990, 6.143261415694495821E-13, 3.111507638930570854E-58 ) ) ;
#918 = FACE_OUTER_BOUND ( 'NONE', #25241, .T. ) ;
#920 = ORIENTED_EDGE ( 'NONE', *, *, #8697, .T. ) ;
#921 = CARTESIAN_POINT ( 'NONE',  ( -44.59999999999998721, 1.399999999999995914, 3.959797974644454488 ) ) ;
#922 = LINE ( 'NONE', #27667, #8950 ) ;
#923 = ADVANCED_FACE ( 'NONE', ( #2011 ), #8804, .F. ) ;
#924 = EDGE_LOOP ( 'NONE', ( #13849, #2269, #25709, #4752 ) ) ;
#926 = DIRECTION ( 'NONE',  ( 0.000000000000000000, 0.000000000000000000, 1.000000000000000000 ) ) ;
#925 = CARTESIAN_POINT ( 'NONE',  ( 58.65000000000001990, 6.143261415694495821E-13, 3.111507638930570854E-58 ) ) ;
#927 = CARTESIAN_POINT ( 'NONE',  ( 34.55000000000001847, 0.000000000000000000, -2.649999999999999911 ) ) ;
#928 = EDGE_LOOP ( 'NONE', ( #6714, #5334, #16373 ) ) ;
#929 = CARTESIAN_POINT ( 'NONE',  ( -69.18535533905931345, -0.4248245016402720786, 2.071532327734953327 ) ) ;
#930 = DIRECTION ( 'NONE',  ( 0.000000000000000000, -0.2008964009354147484, 0.9796124928211139560 ) ) ;
#931 = DIRECTION ( 'NONE',  ( 0.000000000000000000, 1.000000000000000000, 4.336808689942015369E-15 ) ) ;
#932 = PRESENTATION_STYLE_ASSIGNMENT (( #20729 ) ) ;
#933 = CARTESIAN_POINT ( 'NONE',  ( 51.70000000000001705, -4.179189514726506793, -1.000000000000000000 ) ) ;
#934 = CARTESIAN_POINT ( 'NONE',  ( 51.64281244548085681, -0.8321733326261643304, 1.569379851958366601 ) ) ;
#935 = EDGE_CURVE ( 'NONE', #17628, #18608, #7028, .T. ) ;
#936 = ORIENTED_EDGE ( 'NONE', *, *, #23568, .F. ) ;
#937 = TOROIDAL_SURFACE ( 'NONE', #5490, 3.950000000000000178, 0.05000000000000000278 ) ;
#938 =( BOUNDED_SURFACE ( )  B_SPLINE_SURFACE ( 3, 2, ( 
 ( #19024, #11734, #2554 ),
 ( #30892, #16809, #26139 ),
 ( #9821, #23778, #2069 ),
 ( #9208, #19488, #24077 ),
 ( #6815, #12054, #9683 ),
 ( #7455, #26771, #5074 ),
 ( #14726, #24387, #18869 ),
 ( #21408, #28682, #26299 ),
 ( #4600, #23927, #17739 ),
 ( #27380, #15509, #24528 ),
 ( #12649, #29433, #19952 ),
 ( #15193, #29585, #12336 ),
 ( #12966, #5373, #3313 ),
 ( #7745, #5690, #17411 ),
 ( #24842, #10282, #22184 ),
 ( #777, #24694, #20281 ) ),
 .UNSPECIFIED., .F., .F., .F. ) 
 B_SPLINE_SURFACE_WITH_KNOTS ( ( 4, 2, 2, 2, 2, 2, 2, 4 ),
 ( 3, 3 ),
 ( 0.001780502285214210318, 0.002558945925323797589, 0.002753556835351194353, 0.002948167745378591116, 0.003337389565433385077, 0.003726611385488179037, 0.004115833205542972564, 0.004894276845652559618 ),
 ( 0.000000000000000000, 1.000000000000000000 ),
 .UNSPECIFIED. ) 
 GEOMETRIC_REPRESENTATION_ITEM ( )  RATIONAL_B_SPLINE_SURFACE ( (
 ( 1.000000000000000000, 0.9418517008537219404, 1.000000000000000000),
 ( 1.000000000000000000, 0.9417987965885504797, 1.000000000000000000),
 ( 1.000000000000000000, 0.9418198861733489968, 1.000000000000000000),
 ( 1.000000000000000000, 0.9434060303845699380, 1.000000000000000000),
 ( 1.000000000000000000, 0.9437939819948041320, 1.000000000000000000),
 ( 1.000000000000000000, 0.9445989566712896801, 1.000000000000000000),
 ( 1.000000000000000000, 0.9450169930049926448, 1.000000000000000000),
 ( 1.000000000000000000, 0.9461610507673384740, 1.000000000000000000),
 ( 1.000000000000000000, 0.9467217966427268205, 1.000000000000000000),
 ( 1.000000000000000000, 0.9467345476124273684, 1.000000000000000000),
 ( 1.000000000000000000, 0.9461964028052701758, 1.000000000000000000),
 ( 1.000000000000000000, 0.9446801822474041321, 1.000000000000000000),
 ( 1.000000000000000000, 0.9437582546536517070, 1.000000000000000000),
 ( 1.000000000000000000, 0.9418129560295660507, 1.000000000000000000),
 ( 1.000000000000000000, 0.9418016889777457434, 1.000000000000000000),
 ( 1.000000000000000000, 0.9418517008537213853, 1.000000000000000000) ) ) 
 REPRESENTATION_ITEM ( '' )  SURFACE ( )  );
#939 = ADVANCED_FACE ( 'NONE', ( #28303 ), #31138, .F. ) ;
#940 = CARTESIAN_POINT ( 'NONE',  ( -62.06710100716626499, -2.504070139480777613, -0.3244344873171103316 ) ) ;
#941 = CARTESIAN_POINT ( 'NONE',  ( 58.45000000000001705, -0.8000000000000000444, -2.421260002560650104 ) ) ;
#942 = FACE_OUTER_BOUND ( 'NONE', #27423, .T. ) ;
#943 = EDGE_CURVE ( 'NONE', #26590, #11900, #22875, .T. ) ;
#944 = EDGE_CURVE ( 'NONE', #1060, #23376, #21759, .T. ) ;
#945 = CARTESIAN_POINT ( 'NONE',  ( -58.94702994616202574, -2.078460969082611243, -3.600000000000227018 ) ) ;
#946 = LINE ( 'NONE', #17881, #20702 ) ;
#947 = CARTESIAN_POINT ( 'NONE',  ( 30.91780351980854746, 7.261267790723114679, 2.049999999999891465 ) ) ;
#948 = ORIENTED_EDGE ( 'NONE', *, *, #23612, .F. ) ;
#949 = FACE_OUTER_BOUND ( 'NONE', #15304, .T. ) ;
#950 = VERTEX_POINT ( 'NONE', #419 ) ;
#951 = CARTESIAN_POINT ( 'NONE',  ( 51.12687253673781385, -0.9194130538815391551, 1.491219977510798600 ) ) ;
#953 = DIRECTION ( 'NONE',  ( -1.000000000000000000, -0.000000000000000000, 3.491481338843133355E-15 ) ) ;
#952 = CARTESIAN_POINT ( 'NONE',  ( -54.49305485193549003, -2.337873507123006345, -2.687031364304292680 ) ) ;
#954 = ORIENTED_EDGE ( 'NONE', *, *, #13577, .T. ) ;
#955 = ORIENTED_EDGE ( 'NONE', *, *, #22566, .T. ) ;
#956 = CARTESIAN_POINT ( 'NONE',  ( 58.50000000000001421, 0.8000000000000000444, -2.421260002560650104 ) ) ;
#957 = MECHANICAL_DESIGN_GEOMETRIC_PRESENTATION_REPRESENTATION (  '', ( #11070 ), #9033 ) ;
#958 = VECTOR ( 'NONE', #6160, 1000.000000000000000 ) ;
#959 = CARTESIAN_POINT ( 'NONE',  ( 29.69543387591359362, 6.938696499881336521, 1.424999999999895683 ) ) ;
#960 = ORIENTED_EDGE ( 'NONE', *, *, #7724, .T. ) ;
#962 = DIRECTION ( 'NONE',  ( 2.581436205204234006E-16, -0.9796124928211140670, -0.2008964009354148872 ) ) ;
#961 = CARTESIAN_POINT ( 'NONE',  ( -56.19702994616206837, -2.078460969082657872, 3.599999999999791811 ) ) ;
#963 = CARTESIAN_POINT ( 'NONE',  ( -56.86042740578360366, -2.936324665650200672, -2.606018187048497747 ) ) ;
#964 = FACE_BOUND ( 'NONE', #10267, .T. ) ;
#965 = DIRECTION ( 'NONE',  ( 0.000000000000000000, 0.000000000000000000, 1.000000000000000000 ) ) ;
#966 = CARTESIAN_POINT ( 'NONE',  ( -61.34999999999997300, -2.606726380931868370, 0.4585432435923214589 ) ) ;
#967 = EDGE_CURVE ( 'NONE', #12164, #18852, #27400, .T. ) ;
#968 = ORIENTED_EDGE ( 'NONE', *, *, #28279, .T. ) ;
#969 = EDGE_CURVE ( 'NONE', #29917, #14986, #115, .T. ) ;
#970 = CARTESIAN_POINT ( 'NONE',  ( -45.15971931043468146, 0.000000000000000000, 0.000000000000000000 ) ) ;
#971 = ADVANCED_FACE ( 'NONE', ( #9768 ), #9919, .T. ) ;
#972 = CARTESIAN_POINT ( 'NONE',  ( 52.88620718028469980, 4.625382794676526466, -1.578939844535521386 ) ) ;
#973 = LINE ( 'NONE', #29606, #20741 ) ;
#974 = CARTESIAN_POINT ( 'NONE',  ( 15.03925126672132961, 0.4576450603546987073, 5.200000000000000178 ) ) ;
#975 = PRESENTATION_LAYER_ASSIGNMENT (  '', '', ( #2521 ) ) ;
#976 = CARTESIAN_POINT ( 'NONE',  ( 57.05000000000001847, -0.7500000000000000000, -2.421260002560649660 ) ) ;
#978 = CARTESIAN_POINT ( 'NONE',  ( 58.74999999305998699, -1.869977652031123094, -0.4744892162740728669 ) ) ;
#977 = CARTESIAN_POINT ( 'NONE',  ( -56.68749999999996447, 1.962990915244759771, -3.400000000000186873 ) ) ;
#979 = DIRECTION ( 'NONE',  ( -2.581436205204234499E-16, 0.9796124928211140670, 0.2008964009354147762 ) ) ;
#980 = CARTESIAN_POINT ( 'NONE',  ( 52.86869685578782452, 4.158893372528646104, -2.046892089072104959 ) ) ;
#982 = CARTESIAN_POINT ( 'NONE',  ( -54.49999999999997868, 0.7936213912637685164, -3.348412945455685907 ) ) ;
#981 = CARTESIAN_POINT ( 'NONE',  ( -59.24236485150797904, -3.064388189877631063, 1.492323961017689493 ) ) ;
#983 = ORIENTED_EDGE ( 'NONE', *, *, #25197, .F. ) ;
#984 = CARTESIAN_POINT ( 'NONE',  ( 50.29999999999740368, -1.409901620923685206, -3.849999999997240518 ) ) ;
#985 = FACE_OUTER_BOUND ( 'NONE', #19485, .T. ) ;
#986 = AXIS2_PLACEMENT_3D ( 'NONE', #6730, #26038, #21171 ) ;
#988 = CARTESIAN_POINT ( 'NONE',  ( -59.60127941732039147, -2.337454683938988698, -1.248534441610049450 ) ) ;
#987 = CARTESIAN_POINT ( 'NONE',  ( 15.17256654081427492, 2.686240678227970413, -4.475885392925021300 ) ) ;
#989 = CARTESIAN_POINT ( 'NONE',  ( 58.75000000000000711, 1.039502773797200019, -1.800471618823823450 ) ) ;
#990 = EDGE_LOOP ( 'NONE', ( #18643, #27738, #24622, #5621, #14527, #4921 ) ) ;
#991 = CARTESIAN_POINT ( 'NONE',  ( 54.17703590114060574, 6.867671797591380134, 2.049999999999811084 ) ) ;
#992 = CARTESIAN_POINT ( 'NONE',  ( 47.10000000000002274, -4.179189514726507682, 0.9999999999999997780 ) ) ;
#993 = CIRCLE ( 'NONE', #14134, 0.1000000000000000611 ) ;
#994 = ORIENTED_EDGE ( 'NONE', *, *, #9268, .T. ) ;
#995 = CARTESIAN_POINT ( 'NONE',  ( -54.49999999999997868, 8.366749974758391359E-15, -1.938977325913827332E-13 ) ) ;
#996 = EDGE_LOOP ( 'NONE', ( #25581, #2177, #9610, #14667, #5663, #17467 ) ) ;
#997 = CARTESIAN_POINT ( 'NONE',  ( 58.75000000000000711, 1.039502773796331159, 1.800471618825331355 ) ) ;
#998 = CARTESIAN_POINT ( 'NONE',  ( 51.36308620441097617, 1.097739233406260118, -1.198394850649635357 ) ) ;
#999 = AXIS2_PLACEMENT_3D ( 'NONE', #17424, #965, #5390 ) ;
#1000 = ORIENTED_EDGE ( 'NONE', *, *, #568, .F. ) ;
#1001 = DIRECTION ( 'NONE',  ( 1.000000000000000000, 8.626663965456006092E-17, 1.494526870159786164E-16 ) ) ;
#1002 = CARTESIAN_POINT ( 'NONE',  ( -58.63452994616204705, 3.117691453623979481, 1.799999999999803757 ) ) ;
#1003 = CIRCLE ( 'NONE', #9086, 4.600000000000036948 ) ;
#1004 = ORIENTED_EDGE ( 'NONE', *, *, #24904, .T. ) ;
#1005 = DIRECTION ( 'NONE',  ( 0.000000000000000000, -0.2008964009354147484, 0.9796124928211139560 ) ) ;
#1006 = CARTESIAN_POINT ( 'NONE',  ( 23.93127868632236144, 5.811091648295740875, 2.049999999999915445 ) ) ;
#1007 = ORIENTED_EDGE ( 'NONE', *, *, #19113, .F. ) ;
#1008 = CIRCLE ( 'NONE', #25269, 0.05000000000000014155 ) ;
#1009 = ADVANCED_FACE ( 'NONE', ( #29077 ), #17212, .F. ) ;
#1010 = CARTESIAN_POINT ( 'NONE',  ( -58.87499999999996447, 2.944486372867106905, -1.700000000000196465 ) ) ;
#1011 = DIRECTION ( 'NONE',  ( -1.000000000000000000, 0.000000000000000000, 0.000000000000000000 ) ) ;
#1012 = DIRECTION ( 'NONE',  ( 0.000000000000000000, 0.000000000000000000, 1.000000000000000000 ) ) ;
#1013 = FACE_OUTER_BOUND ( 'NONE', #20174, .T. ) ;
#1014 = CARTESIAN_POINT ( 'NONE',  ( 50.25000000000000000, 1.800471618824854181, -1.039502773795712987 ) ) ;
#1016 = CARTESIAN_POINT ( 'NONE',  ( 51.25000000000001421, 5.368152558471320595E-13, 3.111507638930570854E-58 ) ) ;
#1015 = DIRECTION ( 'NONE',  ( 1.000000000000000000, 1.047444401652940007E-14, 0.000000000000000000 ) ) ;
#1017 = DIRECTION ( 'NONE',  ( 0.000000000000000000, -0.9996898646859344595, -0.02490330187381124133 ) ) ;
#1018 = DIRECTION ( 'NONE',  ( -0.5633368246414943714, -0.8262273428075581627, 0.000000000000000000 ) ) ;
#1019 = DIRECTION ( 'NONE',  ( 1.000000000000000000, 4.939082069373669245E-17, -1.520093157366878429E-16 ) ) ;
#1020 = CIRCLE ( 'NONE', #14671, 4.100000000000022737 ) ;
#1021 = EDGE_CURVE ( 'NONE', #10599, #1198, #21966, .T. ) ;
#1022 = CARTESIAN_POINT ( 'NONE',  ( -54.46926330052497178, 1.503605180550108944, -3.302415457191590242 ) ) ;
#1023 = CARTESIAN_POINT ( 'NONE',  ( 52.14998464476281725, 8.689016205149746597, -2.050000000000180567 ) ) ;
#1024 = AXIS2_PLACEMENT_3D ( 'NONE', #23682, #18298, #6253 ) ;
#1025 = ORIENTED_EDGE ( 'NONE', *, *, #13535, .T. ) ;
#1026 = CARTESIAN_POINT ( 'NONE',  ( 53.61896909490565832, 5.359691232772922476, 1.649479992712508336 ) ) ;
#1027 = CIRCLE ( 'NONE', #6586, 0.2999999999999999334 ) ;
#1028 = ORIENTED_EDGE ( 'NONE', *, *, #14158, .T. ) ;
#1029 = ORIENTED_EDGE ( 'NONE', *, *, #3047, .F. ) ;
#1030 = CARTESIAN_POINT ( 'NONE',  ( 61.00000000000002132, 6.389410850082937196E-13, 3.111507638930570854E-58 ) ) ;
#1031 = CARTESIAN_POINT ( 'NONE',  ( -57.29792740578360366, 3.330682475591789871, 0.6830477631804107164 ) ) ;
#1033 = CARTESIAN_POINT ( 'NONE',  ( 47.49423211416725366, -4.280519502657941899, 1.378181460053769625 ) ) ;
#1032 = CARTESIAN_POINT ( 'NONE',  ( -57.62499999999996447, -2.944486372867076707, -1.700000000000215117 ) ) ;
#1034 = ORIENTED_EDGE ( 'NONE', *, *, #1460, .T. ) ;
#1035 = ORIENTED_EDGE ( 'NONE', *, *, #13354, .T. ) ;
#1036 = CARTESIAN_POINT ( 'NONE',  ( 50.80000000000001137, -4.387164041431065087, -1.383037119376935298 ) ) ;
#1037 = VERTEX_POINT ( 'NONE', #24332 ) ;
#1038 = CARTESIAN_POINT ( 'NONE',  ( 51.74168341169266938, 3.850633047928920139, -1.433002550189482083 ) ) ;
#1039 = EDGE_LOOP ( 'NONE', ( #4960, #20256, #26777, #6675, #14995 ) ) ;
#1040 = DIRECTION ( 'NONE',  ( -1.000000000000000000, 1.219044193948983948E-29, -3.491481338843133355E-15 ) ) ;
#1041 = DIRECTION ( 'NONE',  ( 0.000000000000000000, -1.000000000000000000, -5.267838178243386187E-15 ) ) ;
#1042 = DIRECTION ( 'NONE',  ( -2.581436205204234499E-16, 0.9796124928211140670, 0.2008964009354147762 ) ) ;
#1043 = EDGE_CURVE ( 'NONE', #13704, #26101, #4146, .T. ) ;
#1044 = CARTESIAN_POINT ( 'NONE',  ( 47.07331232995326786, -4.179189507151050087, -1.000000000000000000 ) ) ;
#1045 = CARTESIAN_POINT ( 'NONE',  ( -57.95655989232411542, 1.962990915244748891, -3.400000000000197087 ) ) ;
#1046 = CARTESIAN_POINT ( 'NONE',  ( 22.04321716858593661, 7.679566743993218481, -1.550000000000076206 ) ) ;
#1047 = CARTESIAN_POINT ( 'NONE',  ( 47.00300903693474908, -3.614067288483654661, -1.940243272268905361 ) ) ;
#1048 = AXIS2_PLACEMENT_3D ( 'NONE', #10585, #8052, #2989 ) ;
#1049 = CARTESIAN_POINT ( 'NONE',  ( 48.47377487419020525, 1.373801017329653762, 3.853344662332955473 ) ) ;
#1050 = DIRECTION ( 'NONE',  ( 1.000000000000000000, 1.047444401652940007E-14, 0.000000000000000000 ) ) ;
#1052 = CARTESIAN_POINT ( 'NONE',  ( 50.91890276716776498, -4.387164036186654847, 1.383037136012494672 ) ) ;
#1051 = CARTESIAN_POINT ( 'NONE',  ( -59.48031779539610397, 3.173620585043683384, 1.369635785239876169 ) ) ;
#1053 = CARTESIAN_POINT ( 'NONE',  ( -54.39999999999996305, -1.599999999999981215, -3.363870538531692045 ) ) ;
#1054 = CARTESIAN_POINT ( 'NONE',  ( 51.25000000000001421, 5.368152558471320595E-13, 3.111507638930570854E-58 ) ) ;
#1055 = ADVANCED_FACE ( 'NONE', ( #26855 ), #20353, .F. ) ;
#1056 = CARTESIAN_POINT ( 'NONE',  ( 51.80000000000001137, 6.475000000000062705, -1.950000000000180256 ) ) ;
#1057 = ORIENTED_EDGE ( 'NONE', *, *, #12567, .T. ) ;
#1058 = CARTESIAN_POINT ( 'NONE',  ( 58.65000000000000568, 1.571497941946485177, 1.022750809562084306 ) ) ;
#1059 = CARTESIAN_POINT ( 'NONE',  ( 54.30613021257498474, 6.708647431342469325, 2.049999999999810196 ) ) ;
#1060 = VERTEX_POINT ( 'NONE', #31298 ) ;
#1061 = FACE_OUTER_BOUND ( 'NONE', #19043, .T. ) ;
#1062 = ORIENTED_EDGE ( 'NONE', *, *, #27891, .F. ) ;
#1063 = CARTESIAN_POINT ( 'NONE',  ( 58.75000000000000711, 1.932246131438033920, -0.4087173687832938995 ) ) ;
#1064 = CARTESIAN_POINT ( 'NONE',  ( 65.00000000000005684, 4.286263797014729811E-16, 3.499999999999318767 ) ) ;
#1065 = AXIS2_PLACEMENT_3D ( 'NONE', #15106, #7993, #24766 ) ;
#1067 = DIRECTION ( 'NONE',  ( 0.000000000000000000, 0.000000000000000000, 1.000000000000000000 ) ) ;
#1066 = DIRECTION ( 'NONE',  ( -1.018631342913014973E-14, 1.000000000000000000, 0.000000000000000000 ) ) ;
#1068 = ORIENTED_EDGE ( 'NONE', *, *, #20852, .T. ) ;
#1069 = CARTESIAN_POINT ( 'NONE',  ( -64.28602961791190751, 5.004363292900432036E-16, 2.644225585457161048E-15 ) ) ;
#1070 = CARTESIAN_POINT ( 'NONE',  ( -57.22499999999997300, 2.964020293532818446E-15, 1.549317489258324336E-18 ) ) ;
#1072 = CARTESIAN_POINT ( 'NONE',  ( 51.31572262954152563, 0.7526089581382734428, -1.996089927833914146 ) ) ;
#1071 = FACE_OUTER_BOUND ( 'NONE', #23504, .T. ) ;
#1073 = DIRECTION ( 'NONE',  ( 0.000000000000000000, -1.000000000000000000, -1.532429380227459806E-15 ) ) ;
#1074 = VERTEX_POINT ( 'NONE', #7387 ) ;
#1075 = DIRECTION ( 'NONE',  ( -0.8262273428075537218, 0.5633368246415009217, 0.000000000000000000 ) ) ;
#1076 = CARTESIAN_POINT ( 'NONE',  ( -36.77443515226919857, 5.298557911012499844, -1.088945631943488701 ) ) ;
#1077 = FACE_OUTER_BOUND ( 'NONE', #10203, .T. ) ;
#1078 = EDGE_CURVE ( 'NONE', #25198, #6138, #25891, .T. ) ;
#1079 = FACE_OUTER_BOUND ( 'NONE', #31118, .T. ) ;
#1080 = EDGE_CURVE ( 'NONE', #7967, #2662, #20471, .T. ) ;
#1081 = CARTESIAN_POINT ( 'NONE',  ( 51.84831113588978724, -0.6920605891655307040, 1.653603923793091068 ) ) ;
#1082 = EDGE_CURVE ( 'NONE', #13576, #11503, #6680, .T. ) ;
#1083 = VERTEX_POINT ( 'NONE', #20221 ) ;
#1084 = STYLED_ITEM ( 'NONE', ( #12456 ), #4756 ) ;
#1085 = CARTESIAN_POINT ( 'NONE',  ( 15.61033468494287213, 2.777216423307958593, 4.646230875016923889 ) ) ;
#1086 = DIRECTION ( 'NONE',  ( 1.000000000000000000, 0.000000000000000000, 0.000000000000000000 ) ) ;
#1087 = EDGE_CURVE ( 'NONE', #6214, #21890, #26505, .T. ) ;
#1088 = CYLINDRICAL_SURFACE ( 'NONE', #11933, 0.7500000000000002220 ) ;
#1089 = DIRECTION ( 'NONE',  ( -0.9993908270190953180, 0.03489949670251091263, 4.336808689942080056E-15 ) ) ;
#1090 = CARTESIAN_POINT ( 'NONE',  ( -59.25952994616205416, -2.272369910876824241E-14, 3.599999999999788702 ) ) ;
#1091 = CARTESIAN_POINT ( 'NONE',  ( 58.75000000000002132, -0.4999999999991334154, 1.863080903344709549 ) ) ;
#1092 = CARTESIAN_POINT ( 'NONE',  ( 32.25145567989078188, 7.901888653700006593, 2.049999999999887468 ) ) ;
#1093 = VERTEX_POINT ( 'NONE', #17980 ) ;
#1094 = AXIS2_PLACEMENT_3D ( 'NONE', #17029, #80, #10049 ) ;
#1095 = CARTESIAN_POINT ( 'NONE',  ( -54.62499999999997158, -2.944486372867076707, -1.700000000000204903 ) ) ;
#1096 = ORIENTED_EDGE ( 'NONE', *, *, #14201, .T. ) ;
#1098 = CARTESIAN_POINT ( 'NONE',  ( 33.47623932017462778, -4.374999999999999112, 0.000000000000000000 ) ) ;
#1097 = CARTESIAN_POINT ( 'NONE',  ( 48.41523095594689607, 1.115727354199254950, 3.895947837398489266 ) ) ;
#1099 = EDGE_CURVE ( 'NONE', #23396, #4604, #14785, .T. ) ;
#1100 = EDGE_LOOP ( 'NONE', ( #28602, #8868, #21545 ) ) ;
#1101 = VERTEX_POINT ( 'NONE', #24789 ) ;
#1102 = CARTESIAN_POINT ( 'NONE',  ( 67.99999999999998579, 1.401298464324817071E-42, -2.375000000000710543 ) ) ;
#1103 = CIRCLE ( 'NONE', #12224, 0.05000000000000009298 ) ;
#1104 = CYLINDRICAL_SURFACE ( 'NONE', #22252, 2.700000000000000178 ) ;
#1105 = ORIENTED_EDGE ( 'NONE', *, *, #20548, .F. ) ;
#1107 = CARTESIAN_POINT ( 'NONE',  ( 58.74160516400056053, 1.017053542743361794, 1.575205926126844513 ) ) ;
#1106 = CARTESIAN_POINT ( 'NONE',  ( -58.57202994616204705, 2.078460969082646770, 3.599999999999799805 ) ) ;
#1108 = CARTESIAN_POINT ( 'NONE',  ( -57.04792740578359656, -2.256877952708263635, 2.542931754211924300 ) ) ;
#1109 = CARTESIAN_POINT ( 'NONE',  ( -73.90999999999998238, 1.259609229504275341, 0.03137816036100692790 ) ) ;
#1110 = EDGE_CURVE ( 'NONE', #3021, #6673, #8594, .T. ) ;
#1111 = FACE_OUTER_BOUND ( 'NONE', #18843, .T. ) ;
#1112 =( BOUNDED_CURVE ( )  B_SPLINE_CURVE ( 2, ( #81, #29045, #4984, #14637, #24302 ),
 .UNSPECIFIED., .F., .T. ) 
 B_SPLINE_CURVE_WITH_KNOTS ( ( 3, 2, 3 ),
 ( 0.7562128299816163191, 0.7592592592592593004, 0.7702506610550023947 ),
 .UNSPECIFIED. ) 
 CURVE ( )  GEOMETRIC_REPRESENTATION_ITEM ( )  RATIONAL_B_SPLINE_CURVE ( ( 0.9631718388946364229, 0.9779602168519400118, 1.000000000000000000, 0.9204812946589053801, 0.9353569697113883752 ) ) 
 REPRESENTATION_ITEM ( '' )  );
#1113 = EDGE_CURVE ( 'NONE', #9750, #11521, #19253, .T. ) ;
#1114 = ADVANCED_FACE ( 'NONE', ( #10373 ), #27630, .F. ) ;
#1115 = EDGE_LOOP ( 'NONE', ( #13305, #18253, #30377, #417 ) ) ;
#1116 = CARTESIAN_POINT ( 'NONE',  ( -61.07202994616202574, 2.078460969082674747, -3.600000000000208367 ) ) ;
#1117 = CARTESIAN_POINT ( 'NONE',  ( 51.38935952926939876, 3.882318105937780928, -2.050000000000178790 ) ) ;
#1118 = CARTESIAN_POINT ( 'NONE',  ( 48.40000000000002700, -0.6304760106459031954, -3.950000000000022826 ) ) ;
#1119 = AXIS2_PLACEMENT_3D ( 'NONE', #13564, #20726, #23248 ) ;
#1120 = CARTESIAN_POINT ( 'NONE',  ( 15.87128154250933321, 0.7269167730138683670, 5.359285300587708356 ) ) ;
#1121 = DIRECTION ( 'NONE',  ( 1.000000000000000000, 1.047444401652940007E-14, 0.000000000000000000 ) ) ;
#1123 = CARTESIAN_POINT ( 'NONE',  ( -36.04581030752770232, 0.7747498452705172678, -5.363501451416294863 ) ) ;
#1122 = CARTESIAN_POINT ( 'NONE',  ( 29.69543387591358652, 6.938696499881336521, -1.425000000000103517 ) ) ;
#1124 = CARTESIAN_POINT ( 'NONE',  ( 58.75000000000003553, -1.760622601995984304, -0.8948927608036236769 ) ) ;
#1125 = DIRECTION ( 'NONE',  ( 1.000000000000000000, 0.000000000000000000, 0.000000000000000000 ) ) ;
#1126 = LINE ( 'NONE', #8249, #22099 ) ;
#1127 = EDGE_LOOP ( 'NONE', ( #21119, #3709, #15108, #26941 ) ) ;
#1128 = CARTESIAN_POINT ( 'NONE',  ( -35.85663232820584057, -1.123735532908306523, -5.289358697221545391 ) ) ;
#1129 = CARTESIAN_POINT ( 'NONE',  ( -36.81959771849334828, 3.629052419422239328, -4.014440194077178781 ) ) ;
#1130 = CIRCLE ( 'NONE', #30969, 0.09999999999999856226 ) ;
#1132 = CARTESIAN_POINT ( 'NONE',  ( -59.60063969940316042, -2.337287690019610231, -1.248834004845451373 ) ) ;
#1131 = CARTESIAN_POINT ( 'NONE',  ( 15.74504787372188730, 3.350344226587782082, -4.246692235171858343 ) ) ;
#1133 = LINE ( 'NONE', #10641, #23637 ) ;
#1134 = EDGE_CURVE ( 'NONE', #8004, #2659, #17833, .T. ) ;
#1135 = ORIENTED_EDGE ( 'NONE', *, *, #4031, .F. ) ;
#1136 = CARTESIAN_POINT ( 'NONE',  ( 54.18071634157382022, 6.868323337799980166, 2.049999999999812861 ) ) ;
#1137 = CARTESIAN_POINT ( 'NONE',  ( 47.05702803641548826, -4.175266387598157714, 1.009028806847064974 ) ) ;
#1138 = ORIENTED_EDGE ( 'NONE', *, *, #28214, .F. ) ;
#1139 = EDGE_CURVE ( 'NONE', #17756, #7548, #15178, .T. ) ;
#1140 = CARTESIAN_POINT ( 'NONE',  ( 47.04142135623732202, -3.767600426651517509, -1.000000000000000000 ) ) ;
#1141 = VERTEX_POINT ( 'NONE', #8013 ) ;
#1142 = DIRECTION ( 'NONE',  ( 1.000000000000000000, 2.586136946169074517E-16, -0.000000000000000000 ) ) ;
#1143 = CARTESIAN_POINT ( 'NONE',  ( 58.64999999999999858, 1.671477153795419390, -0.8495817349390374362 ) ) ;
#1144 = EDGE_LOOP ( 'NONE', ( #6591, #9871, #26617, #31163 ) ) ;
#1145 = CARTESIAN_POINT ( 'NONE',  ( 32.25672990471646528, 7.797045638327628758, 1.949999999999888267 ) ) ;
#1146 = CARTESIAN_POINT ( 'NONE',  ( -56.20655989232413674, 1.962990915244722245, 3.399999999999807621 ) ) ;
#1147 = ORIENTED_EDGE ( 'NONE', *, *, #8319, .F. ) ;
#1148 = CARTESIAN_POINT ( 'NONE',  ( 56.96065904101961763, 0.7273651001630837554, -1.755300599839360265 ) ) ;
#1149 = EDGE_LOOP ( 'NONE', ( #1743, #772, #703, #19736 ) ) ;
#1150 = EDGE_CURVE ( 'NONE', #24563, #7611, #31047, .T. ) ;
#1151 = CARTESIAN_POINT ( 'NONE',  ( -56.43749999999998579, 1.962990915244722689, 3.399999999999807621 ) ) ;
#1152 = CARTESIAN_POINT ( 'NONE',  ( 61.20598745287978915, 0.7563774268569909420, 1.657497327209963345 ) ) ;
#1153 = DIRECTION ( 'NONE',  ( 1.000000000000000000, 3.054025858079668409E-16, -2.042474015755241579E-16 ) ) ;
#1154 = AXIS2_PLACEMENT_3D ( 'NONE', #9213, #7572, #17089 ) ;
#1155 = CARTESIAN_POINT ( 'NONE',  ( 57.01898512823798626, -0.7746824256175574019, -1.734896867090173211 ) ) ;
#1156 = CARTESIAN_POINT ( 'NONE',  ( -67.99999999999997158, -0.3264566515200493790, 1.591870300834312690 ) ) ;
#1158 = CARTESIAN_POINT ( 'NONE',  ( -54.56249999999997868, 4.108500314926512686, -1.367561758111408121 ) ) ;
#1157 = CARTESIAN_POINT ( 'NONE',  ( -57.03335481156722864, 3.238593381231848145, 2.874284765127023356 ) ) ;
#1159 = DIRECTION ( 'NONE',  ( 0.000000000000000000, 1.000000000000000000, 3.491481338843130594E-15 ) ) ;
#1160 = DIRECTION ( 'NONE',  ( 0.000000000000000000, -0.2008964009354147484, 0.9796124928211139560 ) ) ;
#1161 = CARTESIAN_POINT ( 'NONE',  ( -59.69999999999997442, 3.400000000000007905, -2.001823990013003858E-13 ) ) ;
#1162 = CARTESIAN_POINT ( 'NONE',  ( -54.49181037333889321, 1.522049374736507144, -3.314263409011526385 ) ) ;
#1163 = DIRECTION ( 'NONE',  ( 0.9480661539417378769, -0.3180732113053867383, -3.310155284476359054E-15 ) ) ;
#1164 = ORIENTED_EDGE ( 'NONE', *, *, #8587, .T. ) ;
#1165 = CARTESIAN_POINT ( 'NONE',  ( 51.98855675296391610, 0.7791495708613138671, -1.432971607104406520 ) ) ;
#1166 = EDGE_CURVE ( 'NONE', #10094, #30563, #15180, .T. ) ;
#1167 = ADVANCED_FACE ( 'NONE', ( #2948, #22279 ), #15613, .T. ) ;
#1168 = ORIENTED_EDGE ( 'NONE', *, *, #3930, .F. ) ;
#1169 = ORIENTED_EDGE ( 'NONE', *, *, #28931, .F. ) ;
#1170 = EDGE_CURVE ( 'NONE', #7259, #9698, #12636, .T. ) ;
#1171 = CARTESIAN_POINT ( 'NONE',  ( -59.09999999999998010, 2.308634493194285486, 1.301040651491358169 ) ) ;
#1172 = CIRCLE ( 'NONE', #8246, 2.700000000000000178 ) ;
#1173 = CARTESIAN_POINT ( 'NONE',  ( 68.00000000000000000, -0.6617647058823529216, -1.754335336830145975 ) ) ;
#1175 = CARTESIAN_POINT ( 'NONE',  ( -61.39062294604998016, -2.605675279217121165, 0.7053491114958538866 ) ) ;
#1174 = CARTESIAN_POINT ( 'NONE',  ( -57.68749999999996447, -3.925981830489445379, -2.189747187108473037E-13 ) ) ;
#1176 = EDGE_LOOP ( 'NONE', ( #16382, #26534, #25910, #24778 ) ) ;
#1177 = EDGE_LOOP ( 'NONE', ( #22526, #8657, #22619, #30488 ) ) ;
#1178 = CARTESIAN_POINT ( 'NONE',  ( -44.59999999999998010, 8.366749974758271452E-15, -1.593320673368357319E-13 ) ) ;
#1179 = ORIENTED_EDGE ( 'NONE', *, *, #26385, .F. ) ;
#1180 = FACE_OUTER_BOUND ( 'NONE', #3898, .T. ) ;
#1181 = ORIENTED_EDGE ( 'NONE', *, *, #20952, .T. ) ;
#1182 = FACE_OUTER_BOUND ( 'NONE', #8330, .T. ) ;
#1183 = DIRECTION ( 'NONE',  ( -1.000000000000000000, 0.000000000000000000, 3.491481338843133750E-15 ) ) ;
#1184 = ADVANCED_FACE ( 'NONE', ( #30156 ), #18158, .F. ) ;
#1185 = DIRECTION ( 'NONE',  ( 1.000000000000000000, 2.586136946169074517E-16, -0.000000000000000000 ) ) ;
#1186 = CARTESIAN_POINT ( 'NONE',  ( -59.26905989232412253, 2.944486372867092250, 1.699999999999800782 ) ) ;
#1187 = DIRECTION ( 'NONE',  ( 0.000000000000000000, -1.000000000000000000, -4.336808689942015369E-15 ) ) ;
#1188 = CARTESIAN_POINT ( 'NONE',  ( -54.44999999999997442, 0.000000000000000000, 4.650000000000000355 ) ) ;
#1189 = DIRECTION ( 'NONE',  ( -1.000000000000000000, 1.219044193948983948E-29, -3.491481338843133355E-15 ) ) ;
#1190 = CARTESIAN_POINT ( 'NONE',  ( 58.45000000000001705, -0.8000000000000000444, 1.778341924377873751 ) ) ;
#1192 = FACE_OUTER_BOUND ( 'NONE', #13084, .T. ) ;
#1191 = DIRECTION ( 'NONE',  ( 0.000000000000000000, -1.000000000000000000, 0.000000000000000000 ) ) ;
#1193 = PRODUCT_DEFINITION ( 'UNKNOWN', '', #11600, #13260 ) ;
#1194 = AXIS2_PLACEMENT_3D ( 'NONE', #4886, #26749, #24363 ) ;
#1195 = DIRECTION ( 'NONE',  ( -1.000000000000000000, -3.054025858079668409E-16, 2.042474015755241579E-16 ) ) ;
#1196 = DIRECTION ( 'NONE',  ( 1.000000000000000000, 1.047444401652940007E-14, 0.000000000000000000 ) ) ;
#1197 = PLANE ( 'NONE',  #14485 ) ;
#1198 = VERTEX_POINT ( 'NONE', #9264 ) ;
#1199 = CARTESIAN_POINT ( 'NONE',  ( 54.16745733320535550, 5.680725514543202515, 2.049999999999808420 ) ) ;
#1200 = EDGE_LOOP ( 'NONE', ( #2742, #18519, #13836, #1367 ) ) ;
#1201 = ADVANCED_FACE ( 'NONE', ( #11638 ), #13817, .T. ) ;
#1202 = CARTESIAN_POINT ( 'NONE',  ( -59.58155989232410832, -1.962990915244687384, -3.400000000000229061 ) ) ;
#1203 = ORIENTED_EDGE ( 'NONE', *, *, #21381, .T. ) ;
#1204 = CARTESIAN_POINT ( 'NONE',  ( 51.46757676178953034, 4.376162276235350035, 1.549999999999820410 ) ) ;
#1205 = CARTESIAN_POINT ( 'NONE',  ( -54.90835481156723574, 4.108500314926515351, -1.367561758111408565 ) ) ;
#1207 = CARTESIAN_POINT ( 'NONE',  ( 51.79700381482543747, -3.613796805335215190, -1.940711795749421986 ) ) ;
#1206 = FACE_BOUND ( 'NONE', #14694, .T. ) ;
#1208 = ORIENTED_EDGE ( 'NONE', *, *, #19680, .T. ) ;
#1209 = DIRECTION ( 'NONE',  ( -2.581436205204234499E-16, 0.9796124928211140670, 0.2008964009354147762 ) ) ;
#1210 = CARTESIAN_POINT ( 'NONE',  ( 57.01262970566578758, -0.7335977677777304473, -1.792760110902297921 ) ) ;
#1211 = DIRECTION ( 'NONE',  ( 0.000000000000000000, 0.000000000000000000, -1.000000000000000000 ) ) ;
#1212 = DIRECTION ( 'NONE',  ( 1.000000000000000000, 2.586136946169074517E-16, -0.000000000000000000 ) ) ;
#1213 = ORIENTED_EDGE ( 'NONE', *, *, #1304, .T. ) ;
#1214 = AXIS2_PLACEMENT_3D ( 'NONE', #1245, #29438, #7751 ) ;
#1215 = CARTESIAN_POINT ( 'NONE',  ( -36.31414349454750123, 4.927920137446164972, -1.660974799722044093 ) ) ;
#1216 = CARTESIAN_POINT ( 'NONE',  ( 58.73371041428912065, 1.662559130999850865, -0.8671977075788435130 ) ) ;
#1217 = ADVANCED_FACE ( 'NONE', ( #3874 ), #26027, .F. ) ;
#1218 = CARTESIAN_POINT ( 'NONE',  ( -36.14490256869205353, -3.997744010329726816, 3.641645661657106903 ) ) ;
#1219 = DIRECTION ( 'NONE',  ( 0.000000000000000000, -1.000000000000000000, -1.532429380227459806E-15 ) ) ;
#1220 = PRODUCT_DEFINITION_SHAPE ( 'NONE', 'NONE',  #31331 ) ;
#1221 = DIRECTION ( 'NONE',  ( 0.000000000000000000, -1.000000000000000000, 0.000000000000000000 ) ) ;
#1222 = CIRCLE ( 'NONE', #28022, 4.000000000000022204 ) ;
#1224 = EDGE_LOOP ( 'NONE', ( #5036, #21057, #27990, #17078 ) ) ;
#1223 = AXIS2_PLACEMENT_3D ( 'NONE', #16763, #29089, #9936 ) ;
#1225 = CARTESIAN_POINT ( 'NONE',  ( 15.94709373951304698, 2.670851142931325306, 4.702170608191319268 ) ) ;
#1226 = ADVANCED_FACE ( 'NONE', ( #16230 ), #21317, .T. ) ;
#1227 = CARTESIAN_POINT ( 'NONE',  ( -54.49999999999997868, 0.2900967345938421649, -3.387601494358211340 ) ) ;
#1228 = FACE_OUTER_BOUND ( 'NONE', #23026, .T. ) ;
#1229 = AXIS2_PLACEMENT_3D ( 'NONE', #9760, #16741, #26063 ) ;
#1230 = CARTESIAN_POINT ( 'NONE',  ( -35.85663232820579793, 4.683225679163358635, -2.703237727951174119 ) ) ;
#1231 = CARTESIAN_POINT ( 'NONE',  ( 47.00000000000001421, -3.933368109459638884, -2.186004417993339111 ) ) ;
#1232 = CARTESIAN_POINT ( 'NONE',  ( 26.60100329382704487, 5.318777344783313765, 2.049999999999906564 ) ) ;
#1233 = ORIENTED_EDGE ( 'NONE', *, *, #11080, .T. ) ;
#1234 = ADVANCED_FACE ( 'NONE', ( #1498, #8931 ), #11007, .F. ) ;
#1235 = B_SPLINE_CURVE_WITH_KNOTS ( 'NONE', 3,
 ( #13102, #18341, #1218, #3609, #27837, #5829, #29892, #25767, #8204, #1386, #13391, #10879, #23090, #13717, #20411, #20568 ),
 .UNSPECIFIED., .F., .F.,
 ( 4, 2, 2, 2, 2, 2, 2, 4 ),
 ( 0.000000000000000000, 0.0004351083927046433489, 0.0008702167854092866979, 0.001740433570818574263, 0.002175541963523217829, 0.002610650356227860527, 0.003045758748932504093, 0.003480867141637147659 ),
 .UNSPECIFIED. ) ;
#1236 = FACE_OUTER_BOUND ( 'NONE', #6825, .T. ) ;
#1237 = ORIENTED_EDGE ( 'NONE', *, *, #12586, .T. ) ;
#1239 = VECTOR ( 'NONE', #17750, 1000.000000000000000 ) ;
#1238 = PRODUCT_DEFINITION_CONTEXT ( 'detailed design', #4728, 'design' ) ;
#1240 = CARTESIAN_POINT ( 'NONE',  ( 50.42181344116571751, -1.309616516426922006, 3.885368734293527471 ) ) ;
#1242 = DIRECTION ( 'NONE',  ( -0.9993908270190957621, 0.03489949670250098307, 3.491481338843133355E-15 ) ) ;
#1241 = CARTESIAN_POINT ( 'NONE',  ( 48.41306782696076993, 1.296871156637316114, 3.889656364559859192 ) ) ;
#1243 = EDGE_LOOP ( 'NONE', ( #30408, #28047, #15789, #9686 ) ) ;
#1244 = EDGE_LOOP ( 'NONE', ( #29227, #20470, #20678, #22948 ) ) ;
#1245 = CARTESIAN_POINT ( 'NONE',  ( 57.05000000000001847, 0.8000000000000001554, 1.778341924377873973 ) ) ;
#1246 = PLANE ( 'NONE',  #19210 ) ;
#1248 = CARTESIAN_POINT ( 'NONE',  ( -55.53335481156722864, 3.238593381231848145, 2.874284765127022467 ) ) ;
#1247 = CARTESIAN_POINT ( 'NONE',  ( 50.93264724376069097, -4.319730106884872356, -1.256953381662414770 ) ) ;
#1249 =( BOUNDED_CURVE ( )  B_SPLINE_CURVE ( 3, ( #3855, #13504, #1165, #10822 ),
 .UNSPECIFIED., .F., .T. ) 
 B_SPLINE_CURVE_WITH_KNOTS ( ( 4, 4 ),
 ( 4.041453792691655167, 4.300872134317202722 ),
 .UNSPECIFIED. ) 
 CURVE ( )  GEOMETRIC_REPRESENTATION_ITEM ( )  RATIONAL_B_SPLINE_CURVE ( ( 1.000000000000000000, 0.9943997021150918769, 0.9943997021150918769, 1.000000000000000000 ) ) 
 REPRESENTATION_ITEM ( '' )  );
#1250 = CARTESIAN_POINT ( 'NONE',  ( -56.42292740578360366, 1.073804522883522239, 3.225979517392336238 ) ) ;
#1251 = CIRCLE ( 'NONE', #7827, 0.05000000000000143219 ) ;
#1252 = CARTESIAN_POINT ( 'NONE',  ( -54.39999999999999147, -1.600000000000004530, 3.363870538531237742 ) ) ;
#1253 = EDGE_CURVE ( 'NONE', #13929, #13516, #22274, .T. ) ;
#1254 = CARTESIAN_POINT ( 'NONE',  ( 68.05000000000006821, 4.898587196589419731E-16, 3.999999999999287237 ) ) ;
#1255 = CIRCLE ( 'NONE', #22008, 0.1000000000000000472 ) ;
#1256 = VERTEX_POINT ( 'NONE', #25406 ) ;
#1257 = CARTESIAN_POINT ( 'NONE',  ( 47.00195600436720866, -4.143014423056512463, -1.077153443819862222 ) ) ;
#1258 = CARTESIAN_POINT ( 'NONE',  ( 51.75611399313424243, 4.330462468336024884, -1.550000000000180123 ) ) ;
#1259 = CARTESIAN_POINT ( 'NONE',  ( 58.45000000000001705, 0.7500000000000000000, 1.778341924377873751 ) ) ;
#1260 = CARTESIAN_POINT ( 'NONE',  ( 15.44631504820158874, 0.2166734227622383879, 5.199999998325004924 ) ) ;
#1261 = EDGE_CURVE ( 'NONE', #7998, #29251, #5577, .T. ) ;
#1262 = DIRECTION ( 'NONE',  ( 0.000000000000000000, 0.9996898646859343485, 0.02490330187381130031 ) ) ;
#1264 = DIRECTION ( 'NONE',  ( 1.000000000000000000, -1.219044193948983948E-29, 3.491481338843133355E-15 ) ) ;
#1263 = CARTESIAN_POINT ( 'NONE',  ( 22.72662675107778796, 7.272876594663846284, -1.425000000000078870 ) ) ;
#1265 = CARTESIAN_POINT ( 'NONE',  ( 52.99757510872610311, 4.225639836365437496, -2.047297191224516144 ) ) ;
#1267 = CARTESIAN_POINT ( 'NONE',  ( -54.49999999999996447, 3.524671047264929857, -0.9892662586404576963 ) ) ;
#1266 = CARTESIAN_POINT ( 'NONE',  ( 58.64999999999999147, 1.827485639843792864, -0.4207625006677218060 ) ) ;
#1268 = AXIS2_PLACEMENT_3D ( 'NONE', #6662, #6195, #11578 ) ;
#1269 = ORIENTED_EDGE ( 'NONE', *, *, #8234, .T. ) ;
#1270 = EDGE_CURVE ( 'NONE', #13515, #9408, #13646, .T. ) ;
#1271 = CARTESIAN_POINT ( 'NONE',  ( -62.06272861537543406, -2.661683864372939468, -0.3480657431877479668 ) ) ;
#1272 = EDGE_CURVE ( 'NONE', #16489, #14828, #18956, .T. ) ;
#1273 = DIRECTION ( 'NONE',  ( 0.000000000000000000, 0.000000000000000000, 1.000000000000000000 ) ) ;
#1275 = CARTESIAN_POINT ( 'NONE',  ( -59.64819772016205235, -2.360117159334204739, -1.232121303804351919 ) ) ;
#1274 = DIRECTION ( 'NONE',  ( -1.000000000000000000, 1.219044193948983948E-29, -3.491481338843133355E-15 ) ) ;
#1277 = EDGE_CURVE ( 'NONE', #13977, #31086, #23503, .T. ) ;
#1276 = CARTESIAN_POINT ( 'NONE',  ( 61.25000000000000711, 1.499837071477986505, 1.323060376182421782 ) ) ;
#1278 = EDGE_LOOP ( 'NONE', ( #7304, #6677, #15002, #25727 ) ) ;
#1279 = CARTESIAN_POINT ( 'NONE',  ( 51.65293807187810415, 3.825852911387368493, 2.049999999999816414 ) ) ;
#1280 = CARTESIAN_POINT ( 'NONE',  ( -60.64999999999998437, -2.458515422985869670, -1.116110171506649040 ) ) ;
#1281 = AXIS2_PLACEMENT_3D ( 'NONE', #11954, #1983, #11794 ) ;
#1282 =( BOUNDED_SURFACE ( )  B_SPLINE_SURFACE ( 3, 2, ( 
 ( #8208, #18200, #22466 ),
 ( #20109, #29743, #12950 ),
 ( #27367, #5676, #20577 ),
 ( #27684, #15329, #13108 ),
 ( #13250, #1085, #8356 ),
 ( #1225, #5355, #15018 ),
 ( #22640, #27510, #24976 ),
 ( #608, #10734, #24681 ),
 ( #7890, #10269, #20417 ),
 ( #18036, #6005, #30209 ),
 ( #3616, #19938, #29569 ),
 ( #5525, #15179, #3147 ),
 ( #24831, #12787, #27842 ),
 ( #15946, #20732, #11529 ),
 ( #3926, #13721, #13571 ),
 ( #25773, #23099, #30676 ) ),
 .UNSPECIFIED., .F., .F., .F. ) 
 B_SPLINE_SURFACE_WITH_KNOTS ( ( 4, 2, 2, 2, 2, 2, 2, 4 ),
 ( 3, 3 ),
 ( 0.001780502285214191020, 0.002558945925323769834, 0.002753556835351164429, 0.002948167745378559024, 0.003337389565433348214, 0.003726611385488137838, 0.004115833205542927462, 0.004894276845652505842 ),
 ( 0.000000000000000000, 1.000000000000000000 ),
 .UNSPECIFIED. ) 
 GEOMETRIC_REPRESENTATION_ITEM ( )  RATIONAL_B_SPLINE_SURFACE ( (
 ( 1.000000000000000000, 0.9418517008537246049, 1.000000000000000000),
 ( 1.000000000000000000, 0.9417987965884757617, 1.000000000000000000),
 ( 1.000000000000000000, 0.9418198861734519145, 1.000000000000000000),
 ( 1.000000000000000000, 0.9434060303845467343, 1.000000000000000000),
 ( 1.000000000000000000, 0.9437939819948202302, 1.000000000000000000),
 ( 1.000000000000000000, 0.9445989566712769125, 1.000000000000000000),
 ( 1.000000000000000000, 0.9450169930049800993, 1.000000000000000000),
 ( 1.000000000000000000, 0.9461610507673693382, 1.000000000000000000),
 ( 1.000000000000000000, 0.9467217966427217135, 1.000000000000000000),
 ( 1.000000000000000000, 0.9467345476124366943, 1.000000000000000000),
 ( 1.000000000000000000, 0.9461964028052434195, 1.000000000000000000),
 ( 1.000000000000000000, 0.9446801822474353294, 1.000000000000000000),
 ( 1.000000000000000000, 0.9437582546536613659, 1.000000000000000000),
 ( 1.000000000000000000, 0.9418129560295538383, 1.000000000000000000),
 ( 1.000000000000000000, 0.9418016889777609535, 1.000000000000000000),
 ( 1.000000000000000000, 0.9418517008537241608, 1.000000000000000000) ) ) 
 REPRESENTATION_ITEM ( '' )  SURFACE ( )  );
#1283 = ORIENTED_EDGE ( 'NONE', *, *, #4003, .T. ) ;
#1284 = CIRCLE ( 'NONE', #13906, 4.300000000000019362 ) ;
#1285 = CARTESIAN_POINT ( 'NONE',  ( 47.10000000000002274, -3.826179070414207573, -1.000000000000000000 ) ) ;
#1286 = ORIENTED_EDGE ( 'NONE', *, *, #5679, .F. ) ;
#1287 = CARTESIAN_POINT ( 'NONE',  ( 15.18463186935387554, 4.018128179617989737, -3.618665901676263896 ) ) ;
#1288 = CARTESIAN_POINT ( 'NONE',  ( 51.23644008536124517, -1.080112125195908490, -1.214076932077872817 ) ) ;
#1289 = ORIENTED_EDGE ( 'NONE', *, *, #1134, .T. ) ;
#1290 = PRESENTATION_STYLE_ASSIGNMENT (( #20643 ) ) ;
#1291 = CARTESIAN_POINT ( 'NONE',  ( 22.57514569326381348, 6.661564121306509101, 1.949999999999920908 ) ) ;
#1292 = CARTESIAN_POINT ( 'NONE',  ( -59.33155989232412253, 3.925981830489463142, -1.963383503328113345E-13 ) ) ;
#1293 = ORIENTED_EDGE ( 'NONE', *, *, #6756, .F. ) ;
#1294 =( LENGTH_UNIT ( ) NAMED_UNIT ( * ) SI_UNIT ( .MILLI., .METRE. ) );
#1295 = ORIENTED_EDGE ( 'NONE', *, *, #23328, .F. ) ;
#1296 = AXIS2_PLACEMENT_3D ( 'NONE', #22942, #10594, #8211 ) ;
#1297 = VERTEX_POINT ( 'NONE', #9102 ) ;
#1298 = AXIS2_PLACEMENT_3D ( 'NONE', #4590, #28822, #21869 ) ;
#1299 = CARTESIAN_POINT ( 'NONE',  ( -55.49999999999997868, -2.944486372867089141, 1.699999999999791678 ) ) ;
#1300 = CARTESIAN_POINT ( 'NONE',  ( 58.75000002382379449, 0.5510104498278126650, -1.849358057801673505 ) ) ;
#1301 = CARTESIAN_POINT ( 'NONE',  ( 58.64999999999999147, 1.589751505945893095, 0.9947034709630272475 ) ) ;
#1302 = CARTESIAN_POINT ( 'NONE',  ( 56.95000000000001705, -0.6820512820512819596, -1.773360101234998210 ) ) ;
#1304 = EDGE_CURVE ( 'NONE', #2662, #9911, #23210, .T. ) ;
#1303 = AXIS2_PLACEMENT_3D ( 'NONE', #19478, #1396, #29899 ) ;
#1305 = DIRECTION ( 'NONE',  ( -0.000000000000000000, -5.942513678379226626E-16, -1.000000000000000000 ) ) ;
#1306 = EDGE_CURVE ( 'NONE', #30092, #16115, #28416, .T. ) ;
#1308 = FACE_OUTER_BOUND ( 'NONE', #31128, .T. ) ;
#1307 = CARTESIAN_POINT ( 'NONE',  ( -64.31974649313019654, 2.248654970328750835, 0.05601630617085266717 ) ) ;
#1309 = DIRECTION ( 'NONE',  ( 0.000000000000000000, 0.9996898646859344595, 0.02490330187381124133 ) ) ;
#1310 = FACE_OUTER_BOUND ( 'NONE', #11555, .T. ) ;
#1311 = CARTESIAN_POINT ( 'NONE',  ( -59.69464122902330416, 2.086944863889884871, 1.740854861534822273 ) ) ;
#1312 = CARTESIAN_POINT ( 'NONE',  ( 51.89161117884413699, 9.098400920926795976, -1.950000000000180256 ) ) ;
#1313 = CIRCLE ( 'NONE', #15983, 0.1000000000000000611 ) ;
#1314 = CARTESIAN_POINT ( 'NONE',  ( 48.48125827213484484, -1.426739617975169905, 3.843750000000023537 ) ) ;
#1315 = DIRECTION ( 'NONE',  ( 1.000000000000000000, 3.053848253006669023E-16, -2.042510438544995415E-16 ) ) ;
#1316 = ORIENTED_EDGE ( 'NONE', *, *, #1533, .F. ) ;
#1317 = DIRECTION ( 'NONE',  ( 0.000000000000000000, 0.2008964009354147484, -0.9796124928211139560 ) ) ;
#1318 = EDGE_CURVE ( 'NONE', #3662, #19841, #3554, .T. ) ;
#1319 = CIRCLE ( 'NONE', #830, 0.09999999999999986677 ) ;
#1320 = FACE_OUTER_BOUND ( 'NONE', #25481, .T. ) ;
#1321 = B_SPLINE_CURVE_WITH_KNOTS ( 'NONE', 3,
 ( #22697, #3197, #20473, #20634, #27889, #13161, #20322, #22847, #29952, #13300, #30264, #17780, #15236, #22372, #3664, #6059, #15711, #30094, #1280 ),
 .UNSPECIFIED., .F., .F.,
 ( 4, 3, 3, 3, 3, 3, 4 ),
 ( 0.000000000000000000, 1.471960608404959728E-05, 2.936908138775533325E-05, 4.497395798386097826E-05, 6.315917083330272743E-05, 8.519491945895639831E-05, 8.667572485204743640E-05 ),
 .UNSPECIFIED. ) ;
#1322 = VECTOR ( 'NONE', #690, 1000.000000000000000 ) ;
#1323 = VERTEX_POINT ( 'NONE', #6412 ) ;
#1324 = CARTESIAN_POINT ( 'NONE',  ( -59.19999999999997442, 4.156921938165309527, 1.250136525132554910 ) ) ;
#1325 = CARTESIAN_POINT ( 'NONE',  ( -67.92156587216960872, -6.098012745906804249E-16, 3.386787660360170602E-15 ) ) ;
#1327 = CARTESIAN_POINT ( 'NONE',  ( 51.80000000000001847, -3.726179070414207040, -1.041421356237309581 ) ) ;
#1326 = CARTESIAN_POINT ( 'NONE',  ( -58.37499999999996447, -2.944486372867076707, -1.700000000000217781 ) ) ;
#1328 = ORIENTED_EDGE ( 'NONE', *, *, #18494, .T. ) ;
#1329 = CIRCLE ( 'NONE', #6904, 3.399999999999999911 ) ;
#1330 = ORIENTED_EDGE ( 'NONE', *, *, #14511, .F. ) ;
#1331 = CARTESIAN_POINT ( 'NONE',  ( 58.50000000000001421, 0.8000000000000000444, -1.778341924377873751 ) ) ;
#1332 = ORIENTED_EDGE ( 'NONE', *, *, #26822, .F. ) ;
#1333 = AXIS2_PLACEMENT_3D ( 'NONE', #25103, #29529, #2954 ) ;
#1335 = DIRECTION ( 'NONE',  ( 0.000000000000000000, 0.000000000000000000, 1.000000000000000000 ) ) ;
#1334 = AXIS2_PLACEMENT_3D ( 'NONE', #23771, #1731, #18861 ) ;
#1336 = VERTEX_POINT ( 'NONE', #15758 ) ;
#1337 = CARTESIAN_POINT ( 'NONE',  ( 61.09423418603945777, 0.6373668173466511266, 1.895722432253563516 ) ) ;
#1338 = CARTESIAN_POINT ( 'NONE',  ( 51.80000000000002558, -4.003661535119149129, 1.269131321891737274 ) ) ;
#1339 = ORIENTED_EDGE ( 'NONE', *, *, #18345, .T. ) ;
#1340 = CARTESIAN_POINT ( 'NONE',  ( 60.67929986713514978, 1.401298464324817071E-42, -6.355819294205068152E-13 ) ) ;
#1341 = CARTESIAN_POINT ( 'NONE',  ( 51.89360908398611372, -0.6611756245528535025, -1.497563819582787614 ) ) ;
#1342 = CARTESIAN_POINT ( 'NONE',  ( -58.58155989232412253, 3.925981830489463142, -1.937197393286790192E-13 ) ) ;
#1343 = CARTESIAN_POINT ( 'NONE',  ( 47.76154518333414956, -3.901365292554825892, 1.261477279111806515 ) ) ;
#1344 = ADVANCED_FACE ( 'NONE', ( #13352 ), #18735, .T. ) ;
#1345 = AXIS2_PLACEMENT_3D ( 'NONE', #1733, #16321, #25967 ) ;
#1346 = CARTESIAN_POINT ( 'NONE',  ( 15.90468948301721674, 2.602043737612613317, 4.741394629686831230 ) ) ;
#1347 = AXIS2_PLACEMENT_3D ( 'NONE', #24122, #26652, #2730 ) ;
#1348 = EDGE_CURVE ( 'NONE', #31043, #14710, #13675, .T. ) ;
#1349 = CARTESIAN_POINT ( 'NONE',  ( 61.25000000000004263, -1.996089927834276301, 0.1250000000000018041 ) ) ;
#1350 = CIRCLE ( 'NONE', #6931, 1.000000000000000000 ) ;
#1351 = EDGE_CURVE ( 'NONE', #1564, #30058, #17023, .T. ) ;
#1352 = CARTESIAN_POINT ( 'NONE',  ( 58.65000090395038512, -0.5493607500713694192, 1.793027323413614038 ) ) ;
#1354 = CARTESIAN_POINT ( 'NONE',  ( 51.60802515543293367, -4.291220349889137253, 1.660930850246465695 ) ) ;
#1353 = CARTESIAN_POINT ( 'NONE',  ( 57.05000000000001847, -0.7500000000000000000, 2.421260002560649660 ) ) ;
#1355 = CIRCLE ( 'NONE', #16537, 4.099999999999992539 ) ;
#1356 = AXIS2_PLACEMENT_3D ( 'NONE', #5359, #7596, #14714 ) ;
#1357 = CARTESIAN_POINT ( 'NONE',  ( 51.87416143049283335, 8.598705507415685290, -2.050000000000180123 ) ) ;
#1358 = DIRECTION ( 'NONE',  ( 0.000000000000000000, 0.000000000000000000, -1.000000000000000000 ) ) ;
#1359 = AXIS2_PLACEMENT_3D ( 'NONE', #25228, #8134, #15260 ) ;
#1360 = DIRECTION ( 'NONE',  ( -3.489354422748178582E-15, 1.218509414717996338E-16, -1.000000000000000000 ) ) ;
#1361 = TOROIDAL_SURFACE ( 'NONE', #10968, 0.3000000000000000444, 0.05000000000000000278 ) ;
#1362 = ORIENTED_EDGE ( 'NONE', *, *, #12297, .T. ) ;
#1363 = CARTESIAN_POINT ( 'NONE',  ( -59.06249999999997158, 4.108500314926519792, -1.367561758111384140 ) ) ;
#1364 = EDGE_LOOP ( 'NONE', ( #23271, #3401, #8925, #4713 ) ) ;
#1365 = EDGE_CURVE ( 'NONE', #18736, #6720, #22787, .T. ) ;
#1366 = CARTESIAN_POINT ( 'NONE',  ( 51.35619921172967395, -3.851485842263135506, 1.408112718337741764 ) ) ;
#1367 = ORIENTED_EDGE ( 'NONE', *, *, #7484, .F. ) ;
#1368 = CARTESIAN_POINT ( 'NONE',  ( 51.38935952926941297, 3.882318105937780928, 2.049999999999820410 ) ) ;
#1369 = CARTESIAN_POINT ( 'NONE',  ( -58.84585481156723574, -1.184343223768586473, -3.558065644182725418 ) ) ;
#1371 = DIRECTION ( 'NONE',  ( 0.000000000000000000, 0.000000000000000000, -1.000000000000000000 ) ) ;
#1370 = CARTESIAN_POINT ( 'NONE',  ( 60.87284881435256523, -0.5000000998561487942, 1.554802432719775362 ) ) ;
#1372 = CIRCLE ( 'NONE', #30683, 0.1500000000000001887 ) ;
#1373 = ORIENTED_EDGE ( 'NONE', *, *, #24338, .T. ) ;
#1374 = CARTESIAN_POINT ( 'NONE',  ( 29.19131116422931527, 6.114831865242810416, -2.050000000000101963 ) ) ;
#1375 = AXIS2_PLACEMENT_3D ( 'NONE', #7074, #21188, #4680 ) ;
#1376 = DIRECTION ( 'NONE',  ( 1.000000000000000000, -1.219044193948983948E-29, 3.491481338843133355E-15 ) ) ;
#1377 = AXIS2_PLACEMENT_3D ( 'NONE', #1548, #23572, #11690 ) ;
#1378 = ORIENTED_EDGE ( 'NONE', *, *, #3383, .T. ) ;
#1380 = FACE_OUTER_BOUND ( 'NONE', #4096, .T. ) ;
#1379 = DIRECTION ( 'NONE',  ( 1.000000000000000000, 0.000000000000000000, 0.000000000000000000 ) ) ;
#1381 = DIRECTION ( 'NONE',  ( -1.000000000000000000, -3.054025858079668409E-16, 2.042474015755241579E-16 ) ) ;
#1382 = VERTEX_POINT ( 'NONE', #16713 ) ;
#1383 = CARTESIAN_POINT ( 'NONE',  ( -36.27260443516981780, 4.885888067249658739, -1.790336215468594894 ) ) ;
#1384 = CARTESIAN_POINT ( 'NONE',  ( 58.75000000000000000, 1.871971993775707555, -0.6020210199447628696 ) ) ;
#1385 = VECTOR ( 'NONE', #24043, 1000.000000000000000 ) ;
#1386 = CARTESIAN_POINT ( 'NONE',  ( -36.79682133506353381, -2.710596767400086371, 4.680923748383016836 ) ) ;
#1387 = DIRECTION ( 'NONE',  ( 0.9993908270190956511, -0.03489949670250089980, -3.469446951951485842E-15 ) ) ;
#1388 = VECTOR ( 'NONE', #20619, 1000.000000000000000 ) ;
#1389 = AXIS2_PLACEMENT_3D ( 'NONE', #19677, #29454, #22353 ) ;
#1390 = CARTESIAN_POINT ( 'NONE',  ( -59.19999999999996732, -3.264622394567714192, -0.9498634748674711359 ) ) ;
#1391 = B_SPLINE_CURVE_WITH_KNOTS ( 'NONE', 3,
 ( #3206, #10503, #669, #27577, #2902, #5597, #22237, #3533, #29478, #7793, #1145, #10330, #17463, #24747, #10797, #5435, #3058, #12700, #22380, #20001, #29643, #7969, #24890, #22531, #834, #18109, #9057, #3826, #25366, #3986, #6360, #30417, #18406, #1291, #1599, #25682, #28045, #1754, #20792, #13629 ),
 .UNSPECIFIED., .F., .F.,
 ( 4, 2, 2, 2, 2, 2, 2, 2, 2, 2, 2, 2, 2, 2, 2, 2, 2, 2, 2, 4 ),
 ( -6.000000000463940585E-08, 0.0002197707893516534494, 0.0004396015787033115299, 0.0008792631574066276908, 0.001758586314813259145, 0.002637909472219890274, 0.003077571050923215163, 0.003517232629626540052, 0.004396555787033208477, 0.005275878944439876470, 0.007034525259253204647, 0.007913848416659874374, 0.008793171574066544968, 0.009672494731473213828, 0.01055181788887988442, 0.01143114104628655328, 0.01231046420369322388, 0.01318978736109989273, 0.01362944893980322890, 0.01406911051850656159 ),
 .UNSPECIFIED. ) ;
#1392 = ADVANCED_FACE ( 'NONE', ( #28889 ), #8285, .T. ) ;
#1393 = CARTESIAN_POINT ( 'NONE',  ( 33.47623932017462778, 1.734723475976807094E-15, -4.375000000000000000 ) ) ;
#1394 = AXIS2_PLACEMENT_3D ( 'NONE', #286, #17550, #5511 ) ;
#1395 = CIRCLE ( 'NONE', #10003, 0.1500000000000001887 ) ;
#1396 = DIRECTION ( 'NONE',  ( 0.000000000000000000, -0.9119702176296791141, -0.4102564102564098536 ) ) ;
#1397 = CARTESIAN_POINT ( 'NONE',  ( 61.09423418603945777, 0.6373668173466511266, 1.895722432253563516 ) ) ;
#1398 = DIRECTION ( 'NONE',  ( 1.000000000000000000, 3.054025858079668409E-16, -2.042474015755241579E-16 ) ) ;
#1399 = CARTESIAN_POINT ( 'NONE',  ( 58.66118217212479635, -1.874997884618849753, 0.01689491344058241529 ) ) ;
#1400 = CARTESIAN_POINT ( 'NONE',  ( 48.29999997184167881, 0.7900353715961344614, -4.025797886239747214 ) ) ;
#1401 = ORIENTED_EDGE ( 'NONE', *, *, #26434, .T. ) ;
#1402 = EDGE_CURVE ( 'NONE', #22270, #22436, #30762, .T. ) ;
#1403 = DIRECTION ( 'NONE',  ( -1.000000000000000000, 0.000000000000000000, 3.491481338843133355E-15 ) ) ;
#1404 = ORIENTED_EDGE ( 'NONE', *, *, #14756, .T. ) ;
#1405 = CARTESIAN_POINT ( 'NONE',  ( 51.64837794009022076, -0.8283786772106969121, 1.688958810662479104 ) ) ;
#1407 = CARTESIAN_POINT ( 'NONE',  ( 58.65000000000001990, 6.143261415694495821E-13, 3.111507638930570854E-58 ) ) ;
#1406 = CARTESIAN_POINT ( 'NONE',  ( 48.43940831342823117, 1.279117291415143853, 3.870058441400159754 ) ) ;
#1408 = ORIENTED_EDGE ( 'NONE', *, *, #21117, .T. ) ;
#1409 = ORIENTED_EDGE ( 'NONE', *, *, #26244, .T. ) ;
#1410 = DIRECTION ( 'NONE',  ( -0.000000000000000000, -1.000000000000000000, 0.000000000000000000 ) ) ;
#1411 = CARTESIAN_POINT ( 'NONE',  ( 30.89639353480225026, 7.705332860780324644, 1.424999999999891687 ) ) ;
#1413 = DIRECTION ( 'NONE',  ( 1.000000000000000000, 0.000000000000000000, 0.000000000000000000 ) ) ;
#1412 = DIRECTION ( 'NONE',  ( -1.000000000000000000, -0.000000000000000000, 3.491481338843133355E-15 ) ) ;
#1414 = ORIENTED_EDGE ( 'NONE', *, *, #7933, .F. ) ;
#1415 = CARTESIAN_POINT ( 'NONE',  ( -56.17292740578360366, -3.330682475591782765, -0.6830477631804111605 ) ) ;
#1416 = DIRECTION ( 'NONE',  ( 0.000000000000000000, -0.4102564102564100201, -0.9119702176296790030 ) ) ;
#1417 = PRODUCT_CONTEXT ( 'NONE', #25911, 'mechanical' ) ;
#1418 = AXIS2_PLACEMENT_3D ( 'NONE', #9416, #25876, #21459 ) ;
#1419 = CARTESIAN_POINT ( 'NONE',  ( -59.35470925280786503, 2.309531243787677379, 1.299482330928217300 ) ) ;
#1420 = B_SPLINE_CURVE_WITH_KNOTS ( 'NONE', 3,
 ( #857, #29359, #15104, #27138, #24763, #12721, #5612, #25062, #3395, #13186, #22399, #20197 ),
 .UNSPECIFIED., .F., .F.,
 ( 4, 2, 2, 2, 2, 4 ),
 ( 0.000000000000000000, 5.522938194211729973E-05, 0.0001104587638842345995, 0.0002209175277684801765, 0.0004418350555369711949, 0.0008836701110739511719 ),
 .UNSPECIFIED. ) ;
#1421 = ORIENTED_EDGE ( 'NONE', *, *, #10213, .T. ) ;
#1422 = EDGE_CURVE ( 'NONE', #14417, #27508, #12555, .T. ) ;
#1423 = CARTESIAN_POINT ( 'NONE',  ( 47.08054495771335013, -4.178364716350985830, -1.001910748144235308 ) ) ;
#1424 = CARTESIAN_POINT ( 'NONE',  ( -36.23324115033477000, 3.272294129011982466, -4.050092634493898558 ) ) ;
#1425 = DIRECTION ( 'NONE',  ( 1.216509871872722247E-14, 3.491481338843133355E-15, -1.000000000000000000 ) ) ;
#1426 = PLANE ( 'NONE',  #20033 ) ;
#1427 = DIRECTION ( 'NONE',  ( -0.9993908270190957621, 0.03489949670250106634, 3.490838185622846777E-15 ) ) ;
#1429 = CARTESIAN_POINT ( 'NONE',  ( -36.11780688638202008, 1.123735543663980208, -5.289358694936469263 ) ) ;
#1428 = CARTESIAN_POINT ( 'NONE',  ( -57.72499999999997300, 2.811319000628834039E-15, 1.036730182770210180E-16 ) ) ;
#1430 = CIRCLE ( 'NONE', #23702, 0.09999999999999992228 ) ;
#1432 = CARTESIAN_POINT ( 'NONE',  ( -62.09999999999997300, -2.719773892260283876, -0.3638560033992588316 ) ) ;
#1431 = CARTESIAN_POINT ( 'NONE',  ( 58.65000000000001990, 6.143261415694495821E-13, 3.111507638930570854E-58 ) ) ;
#1433 = ORIENTED_EDGE ( 'NONE', *, *, #16160, .F. ) ;
#1434 = EDGE_CURVE ( 'NONE', #12273, #27518, #6793, .T. ) ;
#1435 = CARTESIAN_POINT ( 'NONE',  ( 61.25000000000003553, -0.9999999999993586242, -1.586072192556190252 ) ) ;
#1436 =( BOUNDED_SURFACE ( )  B_SPLINE_SURFACE ( 3, 2, ( 
 ( #15821, #3492, #3779 ),
 ( #13130, #1107, #22819 ),
 ( #21701, #26269, #23426 ),
 ( #18997, #4575, #30704 ),
 ( #12024, #14223, #21384 ),
 ( #26421, #16926, #31172 ),
 ( #9660, #23749, #4717 ),
 ( #14374, #23897, #30863 ),
 ( #21230, #14067, #31008 ),
 ( #19167, #7258, #2189 ) ),
 .UNSPECIFIED., .F., .F., .F. ) 
 B_SPLINE_SURFACE_WITH_KNOTS ( ( 4, 2, 2, 2, 4 ),
 ( 3, 3 ),
 ( 0.0001706658715694773631, 0.0002229276920777904640, 0.0002751895125861035648, 0.0003274513330944167199, 0.0003797131536027298208 ),
 ( 0.000000000000000000, 1.000000000000000000 ),
 .UNSPECIFIED. ) 
 GEOMETRIC_REPRESENTATION_ITEM ( )  RATIONAL_B_SPLINE_SURFACE ( (
 ( 1.000000000000000000, 0.7071067811865445751, 1.000000000000000000),
 ( 1.000000000000000000, 0.7375607040698810568, 1.000000000000000000),
 ( 1.000000000000000000, 0.7730431127426297122, 1.000000000000000000),
 ( 1.000000000000000000, 0.8321012486974134204, 1.000000000000000000),
 ( 1.000000000000000000, 0.8541932017392805943, 1.000000000000000000),
 ( 1.000000000000000000, 0.8545723906046818197, 1.000000000000000000),
 ( 1.000000000000000000, 0.8327032135036619431, 1.000000000000000000),
 ( 1.000000000000000000, 0.7734559727059460155, 1.000000000000000000),
 ( 1.000000000000000000, 0.7377766653993722556, 1.000000000000000000),
 ( 1.000000000000000000, 0.7071067811865451302, 1.000000000000000000) ) ) 
 REPRESENTATION_ITEM ( '' )  SURFACE ( )  );
#1437 = DIRECTION ( 'NONE',  ( 0.000000000000000000, 0.000000000000000000, -1.000000000000000000 ) ) ;
#1439 = CARTESIAN_POINT ( 'NONE',  ( -59.60191903105511813, -2.337626997591211619, -1.248237806062580058 ) ) ;
#1438 = DIRECTION ( 'NONE',  ( -3.489354422748178188E-15, 1.218509414717996091E-16, -1.000000000000000000 ) ) ;
#1440 = FACE_OUTER_BOUND ( 'NONE', #22331, .T. ) ;
#1441 = ORIENTED_EDGE ( 'NONE', *, *, #3910, .T. ) ;
#1442 = CARTESIAN_POINT ( 'NONE',  ( 51.29845177546387447, 3.894758067259834533, 2.049999999999820410 ) ) ;
#1443 = CARTESIAN_POINT ( 'NONE',  ( 51.12687253673781385, -0.9194130538815391551, -1.491219977510798600 ) ) ;
#1444 = EDGE_LOOP ( 'NONE', ( #5295, #15394 ) ) ;
#1445 = B_SPLINE_CURVE_WITH_KNOTS ( 'NONE', 3,
 ( #3476, #20424, #22473, #3151, #8364, #17882, #25459, #10598, #7899, #15502, #8214, #12643, #25314, #17575, #615, #10742, #25158, #1232, #29580, #20275, #13116, #27220, #27851, #22806, #8067, #5533, #947, #6161, #30049, #10276, #3308, #1092, #10437, #10895, #15810, #18047 ),
 .UNSPECIFIED., .F., .F.,
 ( 4, 2, 2, 2, 2, 2, 2, 2, 2, 2, 2, 2, 2, 2, 2, 2, 2, 4 ),
 ( 0.000000000000000000, 0.0004577609249772582344, 0.0009155218499545164689, 0.001373282774931774758, 0.001831043699909032938, 0.002746565549863547780, 0.003662087399818062840, 0.004577609249772577465, 0.005493131099727092959, 0.006408652949681607584, 0.007324174799636122210, 0.009155218499545142788, 0.01007074034949965481, 0.01098626219945416857, 0.01144402312443142111, 0.01190178404940867192, 0.01281730589936317527, 0.01464834959927219932 ),
 .UNSPECIFIED. ) ;
#1446 = DIRECTION ( 'NONE',  ( -3.489354422748178582E-15, 1.218509414717996338E-16, -1.000000000000000000 ) ) ;
#1447 = ADVANCED_FACE ( 'NONE', ( #22244 ), #19856, .F. ) ;
#1448 = ORIENTED_EDGE ( 'NONE', *, *, #2643, .F. ) ;
#1449 = CARTESIAN_POINT ( 'NONE',  ( 15.90468948301722918, 3.705258523861290509, -3.939862169952828452 ) ) ;
#1450 = DIRECTION ( 'NONE',  ( 1.000000000000000000, -0.000000000000000000, -1.047444401652940007E-14 ) ) ;
#1451 = VERTEX_POINT ( 'NONE', #23907 ) ;
#1452 = SURFACE_STYLE_USAGE ( .BOTH. , #15858 ) ;
#1453 = CARTESIAN_POINT ( 'NONE',  ( -55.19702994616203995, -2.078460969082628118, -3.600000000000204814 ) ) ;
#1454 = CARTESIAN_POINT ( 'NONE',  ( -59.58155989232410832, -1.962990915244706924, -3.400000000000217515 ) ) ;
#1455 = ORIENTED_EDGE ( 'NONE', *, *, #30812, .T. ) ;
#1456 = FACE_OUTER_BOUND ( 'NONE', #29555, .T. ) ;
#1457 = EDGE_LOOP ( 'NONE', ( #15335, #7101, #17819, #1921 ) ) ;
#1458 = ORIENTED_EDGE ( 'NONE', *, *, #4399, .T. ) ;
#1459 = AXIS2_PLACEMENT_3D ( 'NONE', #5210, #4906, #17574 ) ;
#1460 = EDGE_CURVE ( 'NONE', #23119, #21532, #3754, .T. ) ;
#1461 = CARTESIAN_POINT ( 'NONE',  ( -55.43749999999997158, -3.925981830489445379, -2.111188856984502568E-13 ) ) ;
#1462 = DIRECTION ( 'NONE',  ( 0.000000000000000000, 0.000000000000000000, -1.000000000000000000 ) ) ;
#1463 = CARTESIAN_POINT ( 'NONE',  ( 31.18344400622543233, 7.296549944477582095, -1.425000000000107958 ) ) ;
#1464 = CARTESIAN_POINT ( 'NONE',  ( 57.05000000000001847, -0.7794871794871796045, -1.732743413496389939 ) ) ;
#1465 = CARTESIAN_POINT ( 'NONE',  ( -54.49999999999996447, -0.3490374893396158695, -3.419248390956425965 ) ) ;
#1467 = CARTESIAN_POINT ( 'NONE',  ( 51.80000000000001847, 6.982261990806648555E-14, -1.796574372350448449E-13 ) ) ;
#1466 = CARTESIAN_POINT ( 'NONE',  ( 51.80000000000001847, 6.982261990806648555E-14, -1.796574372350448449E-13 ) ) ;
#1468 = CIRCLE ( 'NONE', #23234, 1.975000000000001865 ) ;
#1469 = LINE ( 'NONE', #18587, #22573 ) ;
#1470 = CARTESIAN_POINT ( 'NONE',  ( -59.63821477905805324, 2.352792697908280495, -1.234285180173720020 ) ) ;
#1471 = DIRECTION ( 'NONE',  ( 0.000000000000000000, 1.000000000000000000, 0.000000000000000000 ) ) ;
#1472 = CARTESIAN_POINT ( 'NONE',  ( 58.75000000000003553, -1.760622601995690983, -0.8948927608037045012 ) ) ;
#1473 = ADVANCED_FACE ( 'NONE', ( #23597 ), #7274, .F. ) ;
#1474 =( BOUNDED_SURFACE ( )  B_SPLINE_SURFACE ( 3, 2, ( 
 ( #6266, #6430, #13691 ),
 ( #16090, #25570, #25741 ),
 ( #4049, #21477, #2759 ),
 ( #26692, #2464, #4989 ),
 ( #23846, #12408, #24158 ),
 ( #12121, #26368, #7211 ) ),
 .UNSPECIFIED., .F., .F., .F. ) 
 B_SPLINE_SURFACE_WITH_KNOTS ( ( 4, 2, 4 ),
 ( 3, 3 ),
 ( 0.0001437848949530132453, 0.0003024153973479680024, 0.0004610458997429227324 ),
 ( 0.000000000000000000, 1.000000000000000000 ),
 .UNSPECIFIED. ) 
 GEOMETRIC_REPRESENTATION_ITEM ( )  RATIONAL_B_SPLINE_SURFACE ( (
 ( 1.000000000000000000, 0.7071067811865723307, 1.000000000000000000),
 ( 1.000000000000000000, 0.7306243023312024576, 1.000000000000000000),
 ( 1.000000000000000000, 0.7490085278696598792, 1.000000000000000000),
 ( 1.000000000000000000, 0.7725095633943623863, 1.000000000000000000),
 ( 1.000000000000000000, 0.7779630306550003871, 1.000000000000000000),
 ( 1.000000000000000000, 0.7779866052154992273, 1.000000000000000000) ) ) 
 REPRESENTATION_ITEM ( '' )  SURFACE ( )  );
#1476 = AXIS2_PLACEMENT_3D ( 'NONE', #477, #10141, #11927 ) ;
#1475 = CARTESIAN_POINT ( 'NONE',  ( 57.00872446408695993, 0.7491456045391122753, -2.490007504536590588 ) ) ;
#1477 = DIRECTION ( 'NONE',  ( 0.000000000000000000, -0.2008964009354147762, 0.9796124928211140670 ) ) ;
#1478 = VERTEX_POINT ( 'NONE', #4584 ) ;
#1479 = CARTESIAN_POINT ( 'NONE',  ( -54.49999999999997868, -6.938893903907228378E-14, 0.000000000000000000 ) ) ;
#1480 = DIRECTION ( 'NONE',  ( 0.000000000000000000, 0.000000000000000000, 1.000000000000000000 ) ) ;
#1481 = MECHANICAL_DESIGN_GEOMETRIC_PRESENTATION_REPRESENTATION (  '', ( #27754 ), #17683 ) ;
#1482 = AXIS2_PLACEMENT_3D ( 'NONE', #11066, #27699, #1242 ) ;
#1483 = ORIENTED_EDGE ( 'NONE', *, *, #18154, .T. ) ;
#1484 = CARTESIAN_POINT ( 'NONE',  ( 51.25000000000001421, 0.9938153758931693726, 1.589954715908409755 ) ) ;
#1485 = CARTESIAN_POINT ( 'NONE',  ( -44.59999999999995879, -1.433333333333312254, -4.054078878803053954 ) ) ;
#1487 = CARTESIAN_POINT ( 'NONE',  ( 58.75000000000002132, 6.153735859711025284E-13, 3.111507638930570854E-58 ) ) ;
#1486 = CARTESIAN_POINT ( 'NONE',  ( -55.06249999999997158, 3.925981830489463142, -1.814330073843579337E-13 ) ) ;
#1488 = ORIENTED_EDGE ( 'NONE', *, *, #4608, .T. ) ;
#1489 = EDGE_CURVE ( 'NONE', #14148, #10802, #5358, .T. ) ;
#1490 = VERTEX_POINT ( 'NONE', #21073 ) ;
#1491 = ORIENTED_EDGE ( 'NONE', *, *, #1862, .F. ) ;
#1492 = CIRCLE ( 'NONE', #26293, 2.685355339059328106 ) ;
#1493 = CARTESIAN_POINT ( 'NONE',  ( 48.49151045397272242, -1.391941090707485396, 3.850000000000024070 ) ) ;
#1494 = ORIENTED_EDGE ( 'NONE', *, *, #13570, .F. ) ;
#1495 = CARTESIAN_POINT ( 'NONE',  ( 22.41225425035812435, 6.886225699534504585, -1.950000000000111644 ) ) ;
#1496 = ADVANCED_FACE ( 'NONE', ( #16639 ), #8842, .T. ) ;
#1497 = DIRECTION ( 'NONE',  ( 0.000000000000000000, 0.000000000000000000, -1.000000000000000000 ) ) ;
#1498 = FACE_OUTER_BOUND ( 'NONE', #11151, .T. ) ;
#1499 = ORIENTED_EDGE ( 'NONE', *, *, #14118, .F. ) ;
#1500 = DIRECTION ( 'NONE',  ( -1.000000000000000000, -3.053848253006669023E-16, 2.042510438544995415E-16 ) ) ;
#1501 =( REPRESENTATION_RELATIONSHIP ('NONE','NONE', #7047, #27890 ) REPRESENTATION_RELATIONSHIP_WITH_TRANSFORMATION ( #11077 )SHAPE_REPRESENTATION_RELATIONSHIP( ) );
#1502 = EDGE_CURVE ( 'NONE', #489, #27700, #9332, .T. ) ;
#1503 = DIRECTION ( 'NONE',  ( 1.000000000000000000, 1.047444401652940007E-14, 0.000000000000000000 ) ) ;
#1504 = CARTESIAN_POINT ( 'NONE',  ( -61.34999999999997300, -2.482504579955461477, 0.4612981795977083577 ) ) ;
#1505 = EDGE_CURVE ( 'NONE', #16552, #4296, #28743, .T. ) ;
#1506 = CARTESIAN_POINT ( 'NONE',  ( 15.03925126672132961, 2.199885893005915527, 4.939696249117695892 ) ) ;
#1507 = CIRCLE ( 'NONE', #14142, 3.399999999999999911 ) ;
#1508 = CIRCLE ( 'NONE', #26289, 2.100000000000000089 ) ;
#1510 = LINE ( 'NONE', #4047, #10365 ) ;
#1509 = DIRECTION ( 'NONE',  ( 1.000000000000000000, 1.047444401652940007E-14, 0.000000000000000000 ) ) ;
#1511 = AXIS2_PLACEMENT_3D ( 'NONE', #13170, #3373, #5266 ) ;
#1512 = CARTESIAN_POINT ( 'NONE',  ( -59.51662234188409428, -2.295381144444371913, 1.432938519450777326 ) ) ;
#1513 = CARTESIAN_POINT ( 'NONE',  ( -77.28999999999996362, -0.2599193648183464878, -0.006474858487185624310 ) ) ;
#1514 = CYLINDRICAL_SURFACE ( 'NONE', #25070, 0.1000000000000000472 ) ;
#1515 = ORIENTED_EDGE ( 'NONE', *, *, #1253, .F. ) ;
#1516 = CARTESIAN_POINT ( 'NONE',  ( 54.33851261602290350, 5.996233363966824825, -2.046523645606439956 ) ) ;
#1517 = EDGE_LOOP ( 'NONE', ( #10786, #26947 ) ) ;
#1518 = CARTESIAN_POINT ( 'NONE',  ( 51.80000000000003979, -3.550773357292059007, 2.049880134335640758 ) ) ;
#1519 = AXIS2_PLACEMENT_3D ( 'NONE', #7836, #1183, #10841 ) ;
#1520 = ORIENTED_EDGE ( 'NONE', *, *, #16091, .F. ) ;
#1521 = CARTESIAN_POINT ( 'NONE',  ( 54.16188382698978643, 6.950389949135505674, 2.049999999999811084 ) ) ;
#1522 = CARTESIAN_POINT ( 'NONE',  ( -57.03335481156722864, 3.238593381231848145, 2.874284765127022911 ) ) ;
#1524 = CARTESIAN_POINT ( 'NONE',  ( -36.58413561666602476, 3.095036031508457519, 4.435288302043179698 ) ) ;
#1523 = CARTESIAN_POINT ( 'NONE',  ( 60.75000000000003553, -0.6499999999993626432, 1.489337100860685270 ) ) ;
#1525 = ORIENTED_EDGE ( 'NONE', *, *, #13910, .F. ) ;
#1526 = EDGE_CURVE ( 'NONE', #7829, #23041, #4725, .T. ) ;
#1527 = DIRECTION ( 'NONE',  ( 0.000000000000000000, -0.9996898646859343485, -0.02490330187381124133 ) ) ;
#1528 = EDGE_CURVE ( 'NONE', #28315, #6738, #5269, .T. ) ;
#1529 = CARTESIAN_POINT ( 'NONE',  ( -62.39999999999998437, 1.076401154667962023E-15, 2.259002067258145746E-15 ) ) ;
#1530 = ORIENTED_EDGE ( 'NONE', *, *, #16640, .F. ) ;
#1532 = CYLINDRICAL_SURFACE ( 'NONE', #17592, 0.2500000000000000000 ) ;
#1531 = FACE_OUTER_BOUND ( 'NONE', #4571, .T. ) ;
#1533 = EDGE_CURVE ( 'NONE', #10001, #12097, #20968, .T. ) ;
#1534 = CARTESIAN_POINT ( 'NONE',  ( -56.29806624327023457, 3.400000000000004352, 0.9110272542656333572 ) ) ;
#1535 = ORIENTED_EDGE ( 'NONE', *, *, #18081, .T. ) ;
#1536 = CARTESIAN_POINT ( 'NONE',  ( -35.98994760229851408, 5.086913989685197812, -1.171642050077498665 ) ) ;
#1537 = CARTESIAN_POINT ( 'NONE',  ( 58.74999981404330640, 1.865327579934561664, -0.5879486190987924799 ) ) ;
#1538 = VECTOR ( 'NONE', #7234, 1000.000000000000000 ) ;
#1539 = CARTESIAN_POINT ( 'NONE',  ( -35.85663232820584057, 2.199885893005902204, 4.939696249117695892 ) ) ;
#1540 = CARTESIAN_POINT ( 'NONE',  ( 57.05000000000001137, 0.7500000000000000000, 1.746008434843730583 ) ) ;
#1541 = CARTESIAN_POINT ( 'NONE',  ( -57.82202994616206126, 2.078460969082646770, 3.599999999999802025 ) ) ;
#1542 = PLANE ( 'NONE',  #8402 ) ;
#1543 = CARTESIAN_POINT ( 'NONE',  ( -59.11042740578360366, -2.936324665650199783, -2.606018187048500412 ) ) ;
#1544 = DIRECTION ( 'NONE',  ( -0.9993908270190956511, 0.03489949670250096919, 3.491481338843132961E-15 ) ) ;
#1545 = CARTESIAN_POINT ( 'NONE',  ( 36.50000000000002132, 9.184850993605150903E-17, 0.7500000000000001110 ) ) ;
#1547 = AXIS2_PLACEMENT_3D ( 'NONE', #10510, #4108, #5912 ) ;
#1546 = DIRECTION ( 'NONE',  ( 1.000000000000000000, -1.219044193948983948E-29, 3.491481338843133355E-15 ) ) ;
#1548 = CARTESIAN_POINT ( 'NONE',  ( 51.50000000000002132, 1.163569835200988601E-28, -1.798112889504214751E-13 ) ) ;
#1549 = ORIENTED_EDGE ( 'NONE', *, *, #18038, .T. ) ;
#1550 = CARTESIAN_POINT ( 'NONE',  ( 58.65266784251152643, 1.589569034372934730, 0.9945725797258593293 ) ) ;
#1551 = ORIENTED_EDGE ( 'NONE', *, *, #3019, .F. ) ;
#1552 = CARTESIAN_POINT ( 'NONE',  ( 51.87765138016309407, 8.698644590117595499, 2.049999999999819522 ) ) ;
#1554 = DIRECTION ( 'NONE',  ( 0.000000000000000000, 0.000000000000000000, 1.000000000000000000 ) ) ;
#1553 = CARTESIAN_POINT ( 'NONE',  ( 48.47204894654066010, 1.409900792624787513, 3.850000304694921827 ) ) ;
#1555 = ORIENTED_EDGE ( 'NONE', *, *, #533, .T. ) ;
#1556 = ADVANCED_FACE ( 'NONE', ( #28815 ), #8808, .T. ) ;
#1557 = EDGE_LOOP ( 'NONE', ( #27377, #4605, #25802, #28932 ) ) ;
#1558 = CARTESIAN_POINT ( 'NONE',  ( -59.50169947458152819, -2.403253767585091349, -1.124049747732174032 ) ) ;
#1559 = EDGE_CURVE ( 'NONE', #3444, #19303, #1222, .T. ) ;
#1560 = DIRECTION ( 'NONE',  ( 0.000000000000000000, -1.000000000000000000, 0.000000000000000000 ) ) ;
#1561 = SHAPE_REPRESENTATION ( 'Cap Ring', ( #9018 ), #12557 ) ;
#1563 = DIRECTION ( 'NONE',  ( 0.000000000000000000, 0.000000000000000000, -1.000000000000000000 ) ) ;
#1562 = CARTESIAN_POINT ( 'NONE',  ( -60.57202994616203995, -4.156921938165296204, -2.298664652687300067E-13 ) ) ;
#1564 = VERTEX_POINT ( 'NONE', #5200 ) ;
#1565 = CARTESIAN_POINT ( 'NONE',  ( -57.98542740578359656, 2.936324665650206889, 2.606018187048499080 ) ) ;
#1566 = DIRECTION ( 'NONE',  ( 1.000000000000000000, -0.000000000000000000, -1.047444401652940007E-14 ) ) ;
#1567 = STYLED_ITEM ( 'NONE', ( #16134 ), #4661 ) ;
#1568 = CARTESIAN_POINT ( 'NONE',  ( 53.29713869289653871, 4.966949757952739297, -1.611981027863837790 ) ) ;
#1569 = DIRECTION ( 'NONE',  ( 1.000000000000000000, 3.054025858079668409E-16, -2.042474015755241579E-16 ) ) ;
#1570 = CARTESIAN_POINT ( 'NONE',  ( -62.09999999999998010, -2.737158043526072504, 0.2654540351181892688 ) ) ;
#1571 = VERTEX_POINT ( 'NONE', #19638 ) ;
#1572 = ADVANCED_FACE ( 'NONE', ( #4893 ), #27035, .T. ) ;
#1573 = CARTESIAN_POINT ( 'NONE',  ( -57.31249999999996447, -0.7533615035078060629, 3.673546848079176197 ) ) ;
#1574 = CARTESIAN_POINT ( 'NONE',  ( 61.23913277633455721, 0.8963220027434347648, -1.755758457445524279 ) ) ;
#1575 = CARTESIAN_POINT ( 'NONE',  ( 61.25000000000004263, -2.008165151418346728, -0.5380862305909229759 ) ) ;
#1576 = CARTESIAN_POINT ( 'NONE',  ( 21.97322666366010324, 8.076925076899300393, -1.950000000000076117 ) ) ;
#1577 = DIRECTION ( 'NONE',  ( 0.000000000000000000, -1.000000000000000000, -4.379659758543263321E-15 ) ) ;
#1579 = CARTESIAN_POINT ( 'NONE',  ( -54.39999999999996305, 1.400000000000023670, -3.959797974644871044 ) ) ;
#1578 = DIRECTION ( 'NONE',  ( 0.000000000000000000, 0.000000000000000000, 1.000000000000000000 ) ) ;
#1580 = CARTESIAN_POINT ( 'NONE',  ( 47.54430904983911432, -4.350592967663754251, -1.494824413850514011 ) ) ;
#1582 = CARTESIAN_POINT ( 'NONE',  ( 50.25000000000004263, -1.960427193528665679, 0.3958853607747486181 ) ) ;
#1581 = CYLINDRICAL_SURFACE ( 'NONE', #862, 1.000000000000000000 ) ;
#1583 = ORIENTED_EDGE ( 'NONE', *, *, #24855, .T. ) ;
#1584 = VECTOR ( 'NONE', #2324, 1000.000000000000000 ) ;
#1585 = CARTESIAN_POINT ( 'NONE',  ( 67.99999999999998579, 3.214697847761800597E-16, -2.625000000000710987 ) ) ;
#1587 = DIRECTION ( 'NONE',  ( 0.000000000000000000, -1.000000000000000000, -3.491481338843133355E-15 ) ) ;
#1586 = CARTESIAN_POINT ( 'NONE',  ( 58.65838214097832548, 1.819565423307722973, 0.4528606663879586880 ) ) ;
#1588 = CARTESIAN_POINT ( 'NONE',  ( 15.74504787372211290, -5.206628483174585931, 1.466363261642503302 ) ) ;
#1589 = ORIENTED_EDGE ( 'NONE', *, *, #9009, .F. ) ;
#1590 = CARTESIAN_POINT ( 'NONE',  ( 54.21235476094170735, 5.862613896911504696, 2.049999999999810640 ) ) ;
#1591 = FACE_OUTER_BOUND ( 'NONE', #3116, .T. ) ;
#1592 = ADVANCED_FACE ( 'NONE', ( #2680 ), #9968, .F. ) ;
#1593 = ORIENTED_EDGE ( 'NONE', *, *, #1272, .T. ) ;
#1594 = DIRECTION ( 'NONE',  ( 0.000000000000000000, 0.000000000000000000, 1.000000000000000000 ) ) ;
#1595 = ORIENTED_EDGE ( 'NONE', *, *, #21006, .T. ) ;
#1596 = B_SPLINE_CURVE_WITH_KNOTS ( 'NONE', 3,
 ( #27344, #15465, #24658, #10401, #29721, #24954, #10862, #3450 ),
 .UNSPECIFIED., .F., .F.,
 ( 4, 2, 2, 4 ),
 ( 0.000000000000000000, 5.497193010381665759E-05, 0.0001099438602076330306, 0.0002198877204152543789 ),
 .UNSPECIFIED. ) ;
#1597 = CARTESIAN_POINT ( 'NONE',  ( -59.69999999999996732, -2.937205337104083380, -1.958225367202403921 ) ) ;
#1598 = ORIENTED_EDGE ( 'NONE', *, *, #27228, .F. ) ;
#1599 = CARTESIAN_POINT ( 'NONE',  ( 22.38053502801890104, 6.905764555043880648, 1.949999999999922018 ) ) ;
#1600 = CARTESIAN_POINT ( 'NONE',  ( -56.45655989232411542, 1.962990915244748891, -3.400000000000191314 ) ) ;
#1601 = ORIENTED_EDGE ( 'NONE', *, *, #767, .F. ) ;
#1602 = ORIENTED_EDGE ( 'NONE', *, *, #208, .T. ) ;
#1603 = ORIENTED_EDGE ( 'NONE', *, *, #30308, .T. ) ;
#1604 = AXIS2_PLACEMENT_3D ( 'NONE', #20605, #27537, #6178 ) ;
#1605 = CIRCLE ( 'NONE', #23373, 0.1000000000000000472 ) ;
#1606 = EDGE_CURVE ( 'NONE', #27342, #25393, #17410, .T. ) ;
#1607 = CARTESIAN_POINT ( 'NONE',  ( -57.12499999999997868, -3.920666489018328579E-15, 3.399999999999796518 ) ) ;
#1608 = DIRECTION ( 'NONE',  ( 0.000000000000000000, 1.000000000000000000, 3.491481338843130594E-15 ) ) ;
#1609 = DIRECTION ( 'NONE',  ( 0.000000000000000000, 0.000000000000000000, 1.000000000000000000 ) ) ;
#1610 = CARTESIAN_POINT ( 'NONE',  ( -60.49999999999997868, 2.624185894800580066, 0.06537116741875639847 ) ) ;
#1611 = CARTESIAN_POINT ( 'NONE',  ( -44.49999999999997868, -2.749999999999991562, -1.685844928847700069E-13 ) ) ;
#1613 = DIRECTION ( 'NONE',  ( 1.520093157366878429E-16, -0.5877852522924742473, 0.8090169943749465631 ) ) ;
#1612 = DIRECTION ( 'NONE',  ( 1.000000000000000000, 3.054025858079668409E-16, -2.042474015755241579E-16 ) ) ;
#1614 = CARTESIAN_POINT ( 'NONE',  ( 63.50000000000000000, 0.7500000000000000000, -2.238246715074021953 ) ) ;
#1615 = CARTESIAN_POINT ( 'NONE',  ( -59.65728261716281366, 2.366782727822268839, -1.230152085140874263 ) ) ;
#1616 = FACE_OUTER_BOUND ( 'NONE', #7253, .T. ) ;
#1617 = CARTESIAN_POINT ( 'NONE',  ( 56.97364842551142061, 0.7795706648299629560, 2.480376902516343129 ) ) ;
#1618 = PLANE ( 'NONE',  #2300 ) ;
#1619 = CARTESIAN_POINT ( 'NONE',  ( 50.39884346364546985, 0.8930148142854623661, -3.925689827643446428 ) ) ;
#1620 = ORIENTED_EDGE ( 'NONE', *, *, #27872, .T. ) ;
#1622 = CARTESIAN_POINT ( 'NONE',  ( -54.49999999999995737, -3.485114741320604281, -0.1344221940317323061 ) ) ;
#1621 = DIRECTION ( 'NONE',  ( 3.491481338843133355E-15, 0.000000000000000000, 1.000000000000000000 ) ) ;
#1623 =( NAMED_UNIT ( * ) SI_UNIT ( $, .STERADIAN. ) SOLID_ANGLE_UNIT ( ) );
#1624 = EDGE_CURVE ( 'NONE', #320, #12157, #2991, .T. ) ;
#1625 = ORIENTED_EDGE ( 'NONE', *, *, #27794, .F. ) ;
#1626 = CARTESIAN_POINT ( 'NONE',  ( 58.45000000000001705, 0.8000000000000000444, 1.778341924377873751 ) ) ;
#1627 = CARTESIAN_POINT ( 'NONE',  ( -59.62499999999996447, 2.944486372867106905, -1.700000000000199130 ) ) ;
#1628 = ADVANCED_FACE ( 'NONE', ( #26756, #27209 ), #29279, .F. ) ;
#1629 = ORIENTED_EDGE ( 'NONE', *, *, #2077, .F. ) ;
#1630 = ORIENTED_EDGE ( 'NONE', *, *, #27322, .T. ) ;
#1631 = CARTESIAN_POINT ( 'NONE',  ( 51.58839176096986989, -4.227734780419154070, -1.816236823409610679 ) ) ;
#1632 = ORIENTED_EDGE ( 'NONE', *, *, #29506, .T. ) ;
#1633 = CARTESIAN_POINT ( 'NONE',  ( 51.31943556899493331, 1.088761256244167086, -1.206353010735628395 ) ) ;
#1634 = DIRECTION ( 'NONE',  ( 0.000000000000000000, 0.000000000000000000, -1.000000000000000000 ) ) ;
#1635 = VERTEX_POINT ( 'NONE', #12633 ) ;
#1636 = CARTESIAN_POINT ( 'NONE',  ( 24.76493886329395977, 5.404133871416555657, -1.950000000000151390 ) ) ;
#1637 = AXIS2_PLACEMENT_3D ( 'NONE', #28074, #3564, #25711 ) ;
#1638 = DIRECTION ( 'NONE',  ( 2.117927888850091331E-16, -0.02490330187381135929, 0.9996898646859343485 ) ) ;
#1639 = CARTESIAN_POINT ( 'NONE',  ( -54.47481206296395584, -2.548105035733319035, -2.538836448934781664 ) ) ;
#1640 = EDGE_LOOP ( 'NONE', ( #23576, #7511, #21638, #13636 ) ) ;
#1641 = VERTEX_POINT ( 'NONE', #10117 ) ;
#1642 = ADVANCED_FACE ( 'NONE', ( #22317 ), #27005, .T. ) ;
#1643 = CARTESIAN_POINT ( 'NONE',  ( 47.06862320199297756, -4.259946794064910058, -1.000000024775397289 ) ) ;
#1644 = DIRECTION ( 'NONE',  ( 7.637891338979824674E-45, -1.000000000000000000, -3.491481338843135327E-15 ) ) ;
#1645 = CARTESIAN_POINT ( 'NONE',  ( -45.15971931043468146, 4.700000000000000178, 0.000000000000000000 ) ) ;
#1646 = CARTESIAN_POINT ( 'NONE',  ( -59.41132486540516311, 2.423250918913632201, 1.250136525132548027 ) ) ;
#1647 = CARTESIAN_POINT ( 'NONE',  ( 15.32752150720753725, 3.997744010329658426, 3.641645661657159749 ) ) ;
#1648 = FACE_OUTER_BOUND ( 'NONE', #24289, .T. ) ;
#1649 = CARTESIAN_POINT ( 'NONE',  ( 58.73307976133193620, -0.5681412931372339381, 1.786904874453541181 ) ) ;
#1651 = CARTESIAN_POINT ( 'NONE',  ( 51.52218784613614844, -4.266866293145943345, 1.720819027621672381 ) ) ;
#1650 = CARTESIAN_POINT ( 'NONE',  ( -36.27260443516977517, -2.900433254921178428, 4.320265374240116252 ) ) ;
#1652 = EDGE_CURVE ( 'NONE', #18954, #20483, #19935, .T. ) ;
#1653 = DIRECTION ( 'NONE',  ( 1.000000000000000000, 3.054025858079668409E-16, -2.042474015755241579E-16 ) ) ;
#1654 = CARTESIAN_POINT ( 'NONE',  ( -59.12486116251333357, -1.737685414808515905, 3.471684241605564658 ) ) ;
#1655 = DIRECTION ( 'NONE',  ( 0.000000000000000000, 0.000000000000000000, 1.000000000000000000 ) ) ;
#1656 = DIRECTION ( 'NONE',  ( 1.000000000000000000, 1.047444401652940007E-14, 0.000000000000000000 ) ) ;
#1657 = AXIS2_PLACEMENT_3D ( 'NONE', #30446, #11286, #18439 ) ;
#1658 = ORIENTED_EDGE ( 'NONE', *, *, #20916, .T. ) ;
#1659 = ORIENTED_EDGE ( 'NONE', *, *, #1892, .T. ) ;
#1660 = ORIENTED_EDGE ( 'NONE', *, *, #10869, .F. ) ;
#1661 = ADVANCED_FACE ( 'NONE', ( #19471 ), #2369, .T. ) ;
#1662 = DIRECTION ( 'NONE',  ( 1.000000000000000000, 1.047444401652940007E-14, 0.000000000000000000 ) ) ;
#1663 = EDGE_LOOP ( 'NONE', ( #16263, #15937, #26989, #11465 ) ) ;
#1664 = ADVANCED_FACE ( 'NONE', ( #29419 ), #7881, .T. ) ;
#1665 = CARTESIAN_POINT ( 'NONE',  ( 53.90340377275681760, 6.895264694547793560, 2.049999999999684963 ) ) ;
#1666 = CARTESIAN_POINT ( 'NONE',  ( -58.03335481156723574, 0.8699069336946690933, -4.241846523238430144 ) ) ;
#1668 = CARTESIAN_POINT ( 'NONE',  ( -36.92443669619590452, 3.051830235923023604, 4.466755975380251265 ) ) ;
#1667 = CARTESIAN_POINT ( 'NONE',  ( 61.16418558922029547, -0.6863720863828340901, 1.477277441814885073 ) ) ;
#1669 = EDGE_CURVE ( 'NONE', #12243, #22848, #26520, .T. ) ;
#1670 = VERTEX_POINT ( 'NONE', #21711 ) ;
#1671 = ORIENTED_EDGE ( 'NONE', *, *, #20492, .F. ) ;
#1672 = CYLINDRICAL_SURFACE ( 'NONE', #20988, 4.100000000000022737 ) ;
#1673 = ORIENTED_EDGE ( 'NONE', *, *, #1078, .F. ) ;
#1674 = DIRECTION ( 'NONE',  ( 0.000000000000000000, -1.000000000000000000, 0.000000000000000000 ) ) ;
#1675 = ORIENTED_EDGE ( 'NONE', *, *, #851, .F. ) ;
#1677 = FACE_OUTER_BOUND ( 'NONE', #21892, .T. ) ;
#1676 = CARTESIAN_POINT ( 'NONE',  ( -73.89999999999997726, -0.7497673985144535092, -0.01867747640535382878 ) ) ;
#1678 = DIRECTION ( 'NONE',  ( 9.754918421198722508E-16, 0.9601771338024398528, 0.2793919678926571337 ) ) ;
#1679 = ORIENTED_EDGE ( 'NONE', *, *, #5046, .F. ) ;
#1680 = DIRECTION ( 'NONE',  ( -1.000000000000000000, 0.000000000000000000, 0.000000000000000000 ) ) ;
#1681 = CARTESIAN_POINT ( 'NONE',  ( 51.21569492700663062, -0.9844681138054331981, -1.555342057744142359 ) ) ;
#1682 = FACE_OUTER_BOUND ( 'NONE', #29942, .T. ) ;
#1683 = CARTESIAN_POINT ( 'NONE',  ( 49.00000000000004263, -0.6617647058823530326, 1.754335336828920511 ) ) ;
#1684 = CARTESIAN_POINT ( 'NONE',  ( -58.88452994616202574, 2.093608279459372350E-14, -3.600000000000208811 ) ) ;
#1685 = CIRCLE ( 'NONE', #9284, 0.09999999999999997780 ) ;
#1686 = DIRECTION ( 'NONE',  ( 0.000000000000000000, 0.000000000000000000, 1.000000000000000000 ) ) ;
#1687 = CARTESIAN_POINT ( 'NONE',  ( 50.40000000000001279, 0.7711297561636268894, -3.938774833552663335 ) ) ;
#1688 = EDGE_CURVE ( 'NONE', #3021, #30927, #2747, .T. ) ;
#1689 = CARTESIAN_POINT ( 'NONE',  ( -56.54792740578360366, 3.330682475591789871, 0.6830477631804130478 ) ) ;
#1691 = ADVANCED_FACE ( 'NONE', ( #2535, #12183 ), #29117, .T. ) ;
#1690 = CARTESIAN_POINT ( 'NONE',  ( -54.39999999999997016, 1.514093959731561467, -3.183260039818582854 ) ) ;
#1692 = VERTEX_POINT ( 'NONE', #27979 ) ;
#1693 = CARTESIAN_POINT ( 'NONE',  ( 54.34016439512038943, 6.711820450561376994, -2.050000000000188116 ) ) ;
#1694 = CARTESIAN_POINT ( 'NONE',  ( -36.21152527658243514, 0.2904410314644398361, 5.200000000384614296 ) ) ;
#1695 = DIRECTION ( 'NONE',  ( 1.000000000000000000, 3.053848253006669023E-16, -2.042510438544995415E-16 ) ) ;
#1696 = VERTEX_POINT ( 'NONE', #18198 ) ;
#1697 = CARTESIAN_POINT ( 'NONE',  ( -57.24999999999997158, 2.944486372867089585, 1.699999999999812772 ) ) ;
#1698 = ORIENTED_EDGE ( 'NONE', *, *, #22069, .F. ) ;
#1699 = TOROIDAL_SURFACE ( 'NONE', #19434, 2.649999999999999911, 0.05000000000000000278 ) ;
#1701 = CARTESIAN_POINT ( 'NONE',  ( 58.75000000000004263, -1.394635017527501075, 1.253243060178017121 ) ) ;
#1700 = CARTESIAN_POINT ( 'NONE',  ( 48.39328721529930277, 1.343285922954075007, 3.873819829599202791 ) ) ;
#1702 = ADVANCED_FACE ( 'NONE', ( #23094 ), #18343, .F. ) ;
#1703 = EDGE_LOOP ( 'NONE', ( #2562, #14946, #29197, #1747 ) ) ;
#1704 = ORIENTED_EDGE ( 'NONE', *, *, #29407, .F. ) ;
#1705 = CARTESIAN_POINT ( 'NONE',  ( -59.14665968485343228, -2.559517124687094913, -0.9190674295589560394 ) ) ;
#1706 = CARTESIAN_POINT ( 'NONE',  ( -44.49999999999997868, 1.499999999999999556, -4.029888335921975262 ) ) ;
#1708 = CARTESIAN_POINT ( 'NONE',  ( 58.45000000000001705, 0.7500000000000000000, -1.745709025009608784 ) ) ;
#1707 = CARTESIAN_POINT ( 'NONE',  ( -60.00952994616204705, -4.643455692769866465E-15, 3.599999999999786038 ) ) ;
#1709 = VERTEX_POINT ( 'NONE', #20571 ) ;
#1710 = CARTESIAN_POINT ( 'NONE',  ( -60.73542740578358945, -3.725040285533365747, 1.239922660687676093 ) ) ;
#1711 = VECTOR ( 'NONE', #4485, 1000.000000000000000 ) ;
#1712 = CARTESIAN_POINT ( 'NONE',  ( 50.31971926781695004, 8.252744006147214151, 2.049999999999824407 ) ) ;
#1713 = APPLICATION_PROTOCOL_DEFINITION ( 'draft international standard', 'automotive_design', 1998, #7524 ) ;
#1714 = CARTESIAN_POINT ( 'NONE',  ( -61.39919398045554999, -2.624618644152858948, -0.6335224862127015744 ) ) ;
#1715 = CARTESIAN_POINT ( 'NONE',  ( 68.00000000000001421, -1.025519176787267142E-28, -7.122621931239990530E-13 ) ) ;
#1716 = DIRECTION ( 'NONE',  ( 0.000000000000000000, 0.000000000000000000, -1.000000000000000000 ) ) ;
#1717 = ADVANCED_BREP_SHAPE_REPRESENTATION ( '', ( #25183, #9018 ), #25221 ) ;
#1718 = ORIENTED_EDGE ( 'NONE', *, *, #12779, .F. ) ;
#1719 = TOROIDAL_SURFACE ( 'NONE', #5786, 2.750000000000000000, 0.05000000000000000278 ) ;
#1720 = CARTESIAN_POINT ( 'NONE',  ( 57.04306286658350444, -0.7495164233357125561, 1.778776689171566172 ) ) ;
#1721 = CARTESIAN_POINT ( 'NONE',  ( -36.89250464418361020, 3.430438802933478470, -4.182416543699397415 ) ) ;
#1722 = DIRECTION ( 'NONE',  ( 0.000000000000000000, 0.000000000000000000, 1.000000000000000000 ) ) ;
#1723 = AXIS2_PLACEMENT_3D ( 'NONE', #11069, #8535, #18221 ) ;
#1724 = DIRECTION ( 'NONE',  ( 1.000000000000000000, -1.219044193948983948E-29, 3.491481338843133355E-15 ) ) ;
#1725 = ADVANCED_FACE ( 'NONE', ( #25449 ), #4036, .T. ) ;
#1726 = EDGE_CURVE ( 'NONE', #25442, #19414, #7799, .T. ) ;
#1727 = CARTESIAN_POINT ( 'NONE',  ( 16.08093158123429234, 0.2888463313200336779, -5.401384060636564399 ) ) ;
#1729 = DIRECTION ( 'NONE',  ( -1.000000000000000000, -0.000000000000000000, 1.047444401652940007E-14 ) ) ;
#1728 = DIRECTION ( 'NONE',  ( 1.040834085586084257E-14, 0.000000000000000000, 1.000000000000000000 ) ) ;
#1730 = AXIS2_PLACEMENT_3D ( 'NONE', #7436, #14709, #22794 ) ;
#1731 = DIRECTION ( 'NONE',  ( 1.000000000000000000, 0.000000000000000000, 0.000000000000000000 ) ) ;
#1733 = CARTESIAN_POINT ( 'NONE',  ( 51.80000000000001847, 2.428612866367529932E-14, -1.808587333520743709E-13 ) ) ;
#1732 = DIRECTION ( 'NONE',  ( 0.000000000000000000, 0.9996898646859344595, 0.02490330187381105745 ) ) ;
#1734 = VERTEX_POINT ( 'NONE', #3753 ) ;
#1735 = CARTESIAN_POINT ( 'NONE',  ( -74.39999999999997726, 1.239615432210556367, 0.03088009432353080660 ) ) ;
#1736 = DIRECTION ( 'NONE',  ( 0.9993908270190956511, -0.03489949670250096919, -3.491481338843132961E-15 ) ) ;
#1738 = CARTESIAN_POINT ( 'NONE',  ( -36.11780688638068426, 4.683225673667265276, 2.703237737472885538 ) ) ;
#1737 = CARTESIAN_POINT ( 'NONE',  ( 58.74999981196283017, 1.865248186430322752, 0.5877861523419425360 ) ) ;
#1739 = CARTESIAN_POINT ( 'NONE',  ( 15.66436536804551771, -5.256245472275819175, 1.286369972357283675 ) ) ;
#1740 =( GEOMETRIC_REPRESENTATION_CONTEXT ( 3 ) GLOBAL_UNCERTAINTY_ASSIGNED_CONTEXT ( ( #4743 ) ) GLOBAL_UNIT_ASSIGNED_CONTEXT ( ( #18140, #23030, #8747 ) ) REPRESENTATION_CONTEXT ( 'NONE', 'WORKASPACE' ) );
#1741 = EDGE_LOOP ( 'NONE', ( #26496, #6868, #28975, #18320 ) ) ;
#1742 = CIRCLE ( 'NONE', #25547, 0.4999999999999996114 ) ;
#1743 = ORIENTED_EDGE ( 'NONE', *, *, #9646, .F. ) ;
#1744 = CARTESIAN_POINT ( 'NONE',  ( 48.37818655883430807, 1.309616516426969302, 3.885368734293527471 ) ) ;
#1745 = DIRECTION ( 'NONE',  ( 0.000000000000000000, -1.000000000000000000, 0.000000000000000000 ) ) ;
#1746 = ADVANCED_FACE ( 'NONE', ( #13104 ), #15655, .F. ) ;
#1747 = ORIENTED_EDGE ( 'NONE', *, *, #29928, .F. ) ;
#1748 = AXIS2_PLACEMENT_3D ( 'NONE', #12275, #19279, #14185 ) ;
#1749 = CARTESIAN_POINT ( 'NONE',  ( -35.85663232820583346, -3.817150320980530864, 2.203324261490918090 ) ) ;
#1750 = VERTEX_POINT ( 'NONE', #1390 ) ;
#1751 = CYLINDRICAL_SURFACE ( 'NONE', #7892, 0.5000000000000000000 ) ;
#1752 = VERTEX_POINT ( 'NONE', #10881 ) ;
#1753 =( NAMED_UNIT ( * ) PLANE_ANGLE_UNIT ( ) SI_UNIT ( $, .RADIAN. ) );
#1754 = CARTESIAN_POINT ( 'NONE',  ( 22.01652470039608289, 7.767688062055312592, 1.949999999999924016 ) ) ;
#1755 = CARTESIAN_POINT ( 'NONE',  ( -57.08155989232412963, 3.925981830489463142, -1.884825173204143128E-13 ) ) ;
#1756 = ORIENTED_EDGE ( 'NONE', *, *, #1170, .F. ) ;
#1757 =( NAMED_UNIT ( * ) PLANE_ANGLE_UNIT ( ) SI_UNIT ( $, .RADIAN. ) );
#1758 = CIRCLE ( 'NONE', #24519, 1.474417381223824153 ) ;
#1759 = ORIENTED_EDGE ( 'NONE', *, *, #20992, .T. ) ;
#1760 = EDGE_LOOP ( 'NONE', ( #12970, #14626, #2969, #14426 ) ) ;
#1761 = CARTESIAN_POINT ( 'NONE',  ( -59.24999999999997158, -2.944486372867089141, 1.699999999999778799 ) ) ;
#1762 = CARTESIAN_POINT ( 'NONE',  ( -54.95655989232412963, 1.962990915244748891, -3.400000000000186873 ) ) ;
#1763 = FACE_OUTER_BOUND ( 'NONE', #1200, .T. ) ;
#1764 = CIRCLE ( 'NONE', #11908, 0.1000000000000000472 ) ;
#1765 = CARTESIAN_POINT ( 'NONE',  ( 60.88446240048056524, 0.5000000000006363798, 1.718465885608440491 ) ) ;
#1766 = EDGE_CURVE ( 'NONE', #1752, #14189, #12854, .T. ) ;
#1768 = CARTESIAN_POINT ( 'NONE',  ( 51.70000000000002416, 2.428612866367529932E-14, -1.805095852181900386E-13 ) ) ;
#1767 = CARTESIAN_POINT ( 'NONE',  ( 51.25000000000001421, 5.368152558471320595E-13, 3.111507638930570854E-58 ) ) ;
#1769 = FACE_OUTER_BOUND ( 'NONE', #8576, .T. ) ;
#1770 = FACE_OUTER_BOUND ( 'NONE', #25402, .T. ) ;
#1771 = VECTOR ( 'NONE', #23692, 1000.000000000000000 ) ;
#1772 = CARTESIAN_POINT ( 'NONE',  ( 16.07279755198653604, 5.235729994560204048, -1.359191621353886159 ) ) ;
#1773 = CARTESIAN_POINT ( 'NONE',  ( 58.75000000694009827, -1.658042653848017300, -0.9860766835992956780 ) ) ;
#1774 = AXIS2_PLACEMENT_3D ( 'NONE', #16068, #20976, #8758 ) ;
#1775 = DIRECTION ( 'NONE',  ( 0.000000000000000000, 0.000000000000000000, -1.000000000000000000 ) ) ;
#1776 = ORIENTED_EDGE ( 'NONE', *, *, #6848, .T. ) ;
#1778 = CARTESIAN_POINT ( 'NONE',  ( 15.03925126672132784, 3.817150320980643663, 2.203324261490567704 ) ) ;
#1777 = DIRECTION ( 'NONE',  ( -1.000000000000000000, 0.000000000000000000, 1.047444401652940007E-14 ) ) ;
#1779 = PLANE ( 'NONE',  #27597 ) ;
#1780 = ADVANCED_FACE ( 'NONE', ( #27682 ), #17831, .T. ) ;
#1781 = ORIENTED_EDGE ( 'NONE', *, *, #7380, .T. ) ;
#1782 = CARTESIAN_POINT ( 'NONE',  ( 51.80000000000001847, -3.726179070414207928, 1.100000000000000533 ) ) ;
#1783 = CARTESIAN_POINT ( 'NONE',  ( -59.69142724121850563, 2.412383461849218591, -1.233589124872089826 ) ) ;
#1784 = CARTESIAN_POINT ( 'NONE',  ( -55.82202994616203995, 2.078460969082674747, -3.600000000000189715 ) ) ;
#1785 = VERTEX_POINT ( 'NONE', #1980 ) ;
#1786 = AXIS2_PLACEMENT_3D ( 'NONE', #8044, #17551, #27356 ) ;
#1787 = VERTEX_POINT ( 'NONE', #18624 ) ;
#1788 = CIRCLE ( 'NONE', #16470, 0.1000000000000000749 ) ;
#1789 = CARTESIAN_POINT ( 'NONE',  ( 69.24999999999998579, 3.823533025773894613E-16, -2.750000000000725198 ) ) ;
#1790 = ORIENTED_EDGE ( 'NONE', *, *, #24377, .F. ) ;
#1791 = AXIS2_PLACEMENT_3D ( 'NONE', #10351, #20027, #29670 ) ;
#1792 = CARTESIAN_POINT ( 'NONE',  ( 58.75000000000003553, -1.655311165516861083, 1.077297519403202175 ) ) ;
#1793 = CARTESIAN_POINT ( 'NONE',  ( 68.00000000000004263, 0.8382352941176474115, 2.222158093316569438 ) ) ;
#1794 = ORIENTED_EDGE ( 'NONE', *, *, #13176, .T. ) ;
#1795 = CARTESIAN_POINT ( 'NONE',  ( 52.20711756518983293, 0.5000000000005468959, -1.996089927833914146 ) ) ;
#1796 = DIRECTION ( 'NONE',  ( 0.000000000000000000, 0.000000000000000000, -1.000000000000000000 ) ) ;
#1797 = AXIS2_PLACEMENT_3D ( 'NONE', #7442, #459, #10123 ) ;
#1798 = EDGE_CURVE ( 'NONE', #21024, #15281, #30548, .T. ) ;
#1799 = DIRECTION ( 'NONE',  ( -1.000000000000000000, -3.053848253006669023E-16, 2.042510438544995169E-16 ) ) ;
#1800 = VERTEX_POINT ( 'NONE', #1645 ) ;
#1801 = ORIENTED_EDGE ( 'NONE', *, *, #3505, .F. ) ;
#1802 = CIRCLE ( 'NONE', #17505, 4.600000000000000533 ) ;
#1803 = CYLINDRICAL_SURFACE ( 'NONE', #15773, 2.625000000000000444 ) ;
#1804 = CIRCLE ( 'NONE', #13399, 0.1000000000000000472 ) ;
#1805 =( BOUNDED_CURVE ( )  B_SPLINE_CURVE ( 3, ( #14575, #3006, #7288, #19798 ),
 .UNSPECIFIED., .F., .T. ) 
 B_SPLINE_CURVE_WITH_KNOTS ( ( 4, 4 ),
 ( 1.033802687944702203, 1.276740478505648868 ),
 .UNSPECIFIED. ) 
 CURVE ( )  GEOMETRIC_REPRESENTATION_ITEM ( )  RATIONAL_B_SPLINE_CURVE ( ( 1.000000000000000000, 0.9950878134350369386, 0.9950878134350369386, 1.000000000000000000 ) ) 
 REPRESENTATION_ITEM ( '' )  );
#1806 = DIRECTION ( 'NONE',  ( 0.000000000000000000, 0.000000000000000000, 1.000000000000000000 ) ) ;
#1807 = CARTESIAN_POINT ( 'NONE',  ( -54.97085481156724285, 2.489203624310592833, -2.804704140674919799 ) ) ;
#1808 = VERTEX_POINT ( 'NONE', #13682 ) ;
#1809 = DIRECTION ( 'NONE',  ( 1.000000000000000000, -1.219044193948983948E-29, 3.491481338843133355E-15 ) ) ;
#1810 = CARTESIAN_POINT ( 'NONE',  ( -57.22499999999997300, 2.964020293532818446E-15, 1.549317489258312010E-18 ) ) ;
#1811 = EDGE_CURVE ( 'NONE', #13465, #25040, #31059, .T. ) ;
#1812 = CARTESIAN_POINT ( 'NONE',  ( 50.80000000000001847, -3.936726248589971444, -1.145507068360071434 ) ) ;
#1813 = AXIS2_PLACEMENT_3D ( 'NONE', #13875, #30364, #15808 ) ;
#1814 = CARTESIAN_POINT ( 'NONE',  ( 57.03906491987265781, 0.7487895892850940927, -1.779428968492786867 ) ) ;
#1816 = CARTESIAN_POINT ( 'NONE',  ( 58.66118217212468267, -0.9228675180754075669, 1.632243256842505819 ) ) ;
#1815 = CARTESIAN_POINT ( 'NONE',  ( 58.75000000000003553, -1.323060376181095732, -1.499837071478052453 ) ) ;
#1817 = B_SPLINE_CURVE_WITH_KNOTS ( 'NONE', 3,
 ( #2704, #19960, #3016, #15045, #17748, #10143, #7918 ),
 .UNSPECIFIED., .F., .F.,
 ( 4, 3, 4 ),
 ( 0.000000000000000000, 4.155177920956839920E-05, 5.510430741949099299E-05 ),
 .UNSPECIFIED. ) ;
#1818 = AXIS2_PLACEMENT_3D ( 'NONE', #29013, #4951, #3037 ) ;
#1819 = LINE ( 'NONE', #30472, #24589 ) ;
#1820 = CIRCLE ( 'NONE', #4856, 0.1000000000000000472 ) ;
#1821 = LINE ( 'NONE', #11495, #16058 ) ;
#1823 = FACE_OUTER_BOUND ( 'NONE', #28727, .T. ) ;
#1822 = CIRCLE ( 'NONE', #12942, 0.1500000000000001887 ) ;
#1824 = CARTESIAN_POINT ( 'NONE',  ( 51.80000000000001137, -4.003661535119149129, -1.269131321892099207 ) ) ;
#1825 = VERTEX_POINT ( 'NONE', #11482 ) ;
#1826 = CIRCLE ( 'NONE', #7431, 0.1499999999999999667 ) ;
#1827 = VERTEX_POINT ( 'NONE', #6575 ) ;
#1828 = AXIS2_PLACEMENT_3D ( 'NONE', #2424, #26330, #19224 ) ;
#1829 = EDGE_CURVE ( 'NONE', #7143, #11640, #11722, .T. ) ;
#1830 = CARTESIAN_POINT ( 'NONE',  ( 51.85588625589981859, 0.1560022812617363475, -4.362189373992536368 ) ) ;
#1831 = VERTEX_POINT ( 'NONE', #1504 ) ;
#1832 = AXIS2_PLACEMENT_3D ( 'NONE', #11958, #30628, #30802 ) ;
#1833 = CARTESIAN_POINT ( 'NONE',  ( 51.74555621289474061, 3.825902093565871631, 2.049999999999819522 ) ) ;
#1834 = CARTESIAN_POINT ( 'NONE',  ( -55.78335481156723574, 0.8699069336946694264, -4.241846523238430144 ) ) ;
#1836 = CARTESIAN_POINT ( 'NONE',  ( -36.38139716712170468, 2.291889356119548804, 4.901871067649744340 ) ) ;
#1835 = DIRECTION ( 'NONE',  ( 1.000000000000000000, 3.054025858079668409E-16, -2.042474015755241579E-16 ) ) ;
#1837 = ORIENTED_EDGE ( 'NONE', *, *, #11563, .T. ) ;
#1838 = LINE ( 'NONE', #21016, #12869 ) ;
#1839 = ORIENTED_EDGE ( 'NONE', *, *, #8570, .T. ) ;
#1840 = CARTESIAN_POINT ( 'NONE',  ( -59.69999999999997442, 8.366749974758454467E-15, -2.120534355533670266E-13 ) ) ;
#1841 = EDGE_LOOP ( 'NONE', ( #628, #26422, #5505, #21184 ) ) ;
#1843 = FACE_BOUND ( 'NONE', #20133, .T. ) ;
#1842 = DIRECTION ( 'NONE',  ( -1.000000000000000000, 0.000000000000000000, 0.000000000000000000 ) ) ;
#1844 = AXIS2_PLACEMENT_3D ( 'NONE', #9808, #26758, #28820 ) ;
#1845 = ORIENTED_EDGE ( 'NONE', *, *, #7926, .T. ) ;
#1846 = CARTESIAN_POINT ( 'NONE',  ( 53.42585677208777639, 7.844055467211287436, 1.880068497670932537 ) ) ;
#1847 = EDGE_CURVE ( 'NONE', #27521, #23889, #26879, .T. ) ;
#1848 = VECTOR ( 'NONE', #24236, 1000.000000000000000 ) ;
#1849 = CARTESIAN_POINT ( 'NONE',  ( 58.72200624034154259, 1.816790722508793365, -0.4641018782086855921 ) ) ;
#1850 = AXIS2_PLACEMENT_3D ( 'NONE', #6631, #30519, #23420 ) ;
#1851 = CARTESIAN_POINT ( 'NONE',  ( -35.85663232820584057, 1.123735532908267665, -5.289358697221546279 ) ) ;
#1852 = VECTOR ( 'NONE', #28973, 1000.000000000000000 ) ;
#1853 = CARTESIAN_POINT ( 'NONE',  ( 69.25000000000004263, -0.7500000000000000000, 1.988246715072630844 ) ) ;
#1854 = CARTESIAN_POINT ( 'NONE',  ( -59.57202994616203995, 2.078460969082674747, -3.600000000000202593 ) ) ;
#1855 = VECTOR ( 'NONE', #18825, 1000.000000000000000 ) ;
#1856 = CARTESIAN_POINT ( 'NONE',  ( 51.86925381625176357, 0.07373004000955572790, 4.369615861601171325 ) ) ;
#1857 = AXIS2_PLACEMENT_3D ( 'NONE', #23515, #15768, #11021 ) ;
#1858 = EDGE_CURVE ( 'NONE', #19651, #21772, #2734, .T. ) ;
#1859 = VECTOR ( 'NONE', #5757, 1000.000000000000000 ) ;
#1861 = AXIS2_PLACEMENT_3D ( 'NONE', #24937, #17517, #2537 ) ;
#1860 = DIRECTION ( 'NONE',  ( -1.000000000000000000, 0.000000000000000000, 0.000000000000000000 ) ) ;
#1862 = EDGE_CURVE ( 'NONE', #15671, #16732, #14052, .T. ) ;
#1863 = DIRECTION ( 'NONE',  ( 2.581436205204234006E-16, -0.9796124928211140670, -0.2008964009354148872 ) ) ;
#1864 = EDGE_CURVE ( 'NONE', #4537, #9168, #27893, .T. ) ;
#1865 = CARTESIAN_POINT ( 'NONE',  ( -56.11042740578360366, -2.936324665650196675, -2.606018187048503076 ) ) ;
#1866 = DIRECTION ( 'NONE',  ( 1.000000000000000000, -0.000000000000000000, -1.047444401652940007E-14 ) ) ;
#1867 = ORIENTED_EDGE ( 'NONE', *, *, #22678, .T. ) ;
#1868 = CIRCLE ( 'NONE', #21107, 2.549999999999999822 ) ;
#1869 = CARTESIAN_POINT ( 'NONE',  ( 49.00000000000002132, 1.401298464324817071E-42, -5.132477568099407673E-13 ) ) ;
#1870 = CARTESIAN_POINT ( 'NONE',  ( 54.41366571437519184, 6.718673005292170153, -1.976179938780096013 ) ) ;
#1871 = AXIS2_PLACEMENT_3D ( 'NONE', #6443, #8189, #25753 ) ;
#1872 = CARTESIAN_POINT ( 'NONE',  ( -36.30424252565905618, -0.1108756495952975957, 5.200000001675011418 ) ) ;
#1873 = SPHERICAL_SURFACE ( 'NONE', #24635, 0.1000000000000000056 ) ;
#1874 = ORIENTED_EDGE ( 'NONE', *, *, #12571, .T. ) ;
#1875 = EDGE_CURVE ( 'NONE', #10792, #18525, #6890, .T. ) ;
#1876 = CARTESIAN_POINT ( 'NONE',  ( 58.72419296898070940, 1.601054456121395964, 0.9760445624818194776 ) ) ;
#1877 = CIRCLE ( 'NONE', #6952, 0.1499999999999999667 ) ;
#1878 = ORIENTED_EDGE ( 'NONE', *, *, #11695, .T. ) ;
#1879 = DIRECTION ( 'NONE',  ( 0.000000000000000000, -1.000000000000000000, -3.491481338843129017E-15 ) ) ;
#1881 = CARTESIAN_POINT ( 'NONE',  ( 58.74999981196286569, -1.441661833134154636, 1.321459237641457563 ) ) ;
#1880 = CARTESIAN_POINT ( 'NONE',  ( 51.67753520601183936, -4.133513435957371307, -2.021478398489999329 ) ) ;
#1882 = VERTEX_POINT ( 'NONE', #15903 ) ;
#1883 = ORIENTED_EDGE ( 'NONE', *, *, #21252, .T. ) ;
#1884 = DIRECTION ( 'NONE',  ( 0.000000000000000000, 0.000000000000000000, 1.000000000000000000 ) ) ;
#1885 = AXIS2_PLACEMENT_3D ( 'NONE', #11670, #28126, #16410 ) ;
#1886 = CIRCLE ( 'NONE', #27175, 0.05000000000000005829 ) ;
#1888 = CARTESIAN_POINT ( 'NONE',  ( 47.07708546080149858, 8.766223091587903582, 1.549999999999835953 ) ) ;
#1887 = CARTESIAN_POINT ( 'NONE',  ( 51.80000000000001137, -3.995259070520241540, -2.068697874512001267 ) ) ;
#1889 = CIRCLE ( 'NONE', #379, 1.875000000000001776 ) ;
#1890 = ORIENTED_EDGE ( 'NONE', *, *, #27079, .T. ) ;
#1891 = CARTESIAN_POINT ( 'NONE',  ( -55.43749999999997158, 0.8699069336946690933, -4.241846523238429256 ) ) ;
#1892 = EDGE_CURVE ( 'NONE', #3863, #2409, #3845, .T. ) ;
#1893 = CARTESIAN_POINT ( 'NONE',  ( -55.24005354137803181, -3.399999999999995026, 0.9110272542656064898 ) ) ;
#1894 = CONTEXT_DEPENDENT_SHAPE_REPRESENTATION ( #25307, #20998 ) ;
#1895 = DIRECTION ( 'NONE',  ( 1.000000000000000000, 1.047444401652940007E-14, 0.000000000000000000 ) ) ;
#1896 = CARTESIAN_POINT ( 'NONE',  ( -67.99999999999995737, -3.266925685480207642E-16, 2.202315069465528948E-15 ) ) ;
#1897 = EDGE_CURVE ( 'NONE', #17885, #10721, #16797, .T. ) ;
#1898 = CARTESIAN_POINT ( 'NONE',  ( -62.09999999999998721, -2.677618807081935781, 0.1824170939552585136 ) ) ;
#1899 = AXIS2_PLACEMENT_3D ( 'NONE', #11192, #13560, #3744 ) ;
#1900 = VERTEX_POINT ( 'NONE', #31101 ) ;
#1901 = AXIS2_PLACEMENT_3D ( 'NONE', #24169, #2478, #12132 ) ;
#1902 = LINE ( 'NONE', #31188, #22603 ) ;
#1903 = CIRCLE ( 'NONE', #21669, 2.150647426004269835 ) ;
#1904 = CARTESIAN_POINT ( 'NONE',  ( -36.31440869660544735, 3.100731772197836911, -4.174739983989952385 ) ) ;
#1905 = EDGE_CURVE ( 'NONE', #15713, #3198, #25367, .T. ) ;
#1906 = DIRECTION ( 'NONE',  ( 1.000000000000000000, 1.047444401652940007E-14, 0.000000000000000000 ) ) ;
#1907 = CARTESIAN_POINT ( 'NONE',  ( -35.85663232820584057, -1.854603232583471356E-14, -5.200000000000000178 ) ) ;
#1908 = ADVANCED_FACE ( 'NONE', ( #12113 ), #20053, .F. ) ;
#1909 = VECTOR ( 'NONE', #16588, 1000.000000000000000 ) ;
#1910 = CARTESIAN_POINT ( 'NONE',  ( 58.75000000000002132, 6.153735859711025284E-13, 3.111507638930570854E-58 ) ) ;
#1911 = CARTESIAN_POINT ( 'NONE',  ( -59.29999999999997584, -0.7533615035078030653, 3.673546848079178417 ) ) ;
#1913 = CARTESIAN_POINT ( 'NONE',  ( 50.33046473658142617, -1.366509374015013600, -3.854674997130604908 ) ) ;
#1912 = CARTESIAN_POINT ( 'NONE',  ( 65.00000000000007105, 1.401298464324817071E-42, 3.499999999999319211 ) ) ;
#1914 = ORIENTED_EDGE ( 'NONE', *, *, #8510, .F. ) ;
#1915 = CARTESIAN_POINT ( 'NONE',  ( 51.25000000000002842, -1.099999999999462963, -1.996089927833914146 ) ) ;
#1916 = CARTESIAN_POINT ( 'NONE',  ( -54.44999999999997442, -6.938893903907228378E-14, 0.000000000000000000 ) ) ;
#1917 = VECTOR ( 'NONE', #16680, 1000.000000000000000 ) ;
#1919 = CARTESIAN_POINT ( 'NONE',  ( -67.99999999999997158, 0.6177564328764001411, -3.012308415424923780 ) ) ;
#1918 = FACE_OUTER_BOUND ( 'NONE', #16878, .T. ) ;
#1920 = DIRECTION ( 'NONE',  ( -0.000000000000000000, -0.000000000000000000, -1.000000000000000000 ) ) ;
#1921 = ORIENTED_EDGE ( 'NONE', *, *, #16414, .T. ) ;
#1922 = ORIENTED_EDGE ( 'NONE', *, *, #24349, .F. ) ;
#1923 = CARTESIAN_POINT ( 'NONE',  ( 48.34316787720665332, 1.211455355144567703, 3.917539841352833285 ) ) ;
#1924 = CARTESIAN_POINT ( 'NONE',  ( 50.34656340841117839, -1.329326705022595201, 3.861343257506214766 ) ) ;
#1925 = CIRCLE ( 'NONE', #26709, 0.01000000000000001929 ) ;
#1926 = AXIS2_PLACEMENT_3D ( 'NONE', #4634, #4487, #24276 ) ;
#1927 = ORIENTED_EDGE ( 'NONE', *, *, #30575, .T. ) ;
#1928 = CARTESIAN_POINT ( 'NONE',  ( -56.49999999999997158, -2.489203624310589280, 2.804704140674913582 ) ) ;
#1929 = ORIENTED_EDGE ( 'NONE', *, *, #22320, .T. ) ;
#1930 = EDGE_CURVE ( 'NONE', #12841, #15664, #7354, .T. ) ;
#1931 = CARTESIAN_POINT ( 'NONE',  ( 58.75000000000000000, 1.972190280208565571, -0.1053114364790996016 ) ) ;
#1932 = ORIENTED_EDGE ( 'NONE', *, *, #14326, .F. ) ;
#1933 = ADVANCED_FACE ( 'NONE', ( #21468 ), #23872, .T. ) ;
#1934 = CARTESIAN_POINT ( 'NONE',  ( -60.14405989232410832, 2.944486372867106461, -1.700000000000200684 ) ) ;
#1935 = VERTEX_POINT ( 'NONE', #19094 ) ;
#1936 =( NAMED_UNIT ( * ) PLANE_ANGLE_UNIT ( ) SI_UNIT ( $, .RADIAN. ) );
#1937 = EDGE_CURVE ( 'NONE', #28767, #12009, #26394, .T. ) ;
#1938 = EDGE_LOOP ( 'NONE', ( #12459, #23077, #1593, #2183, #2772, #8705, #7012, #6440, #1602, #10918, #15569, #29963, #25365, #13655, #18880, #9456, #23543 ) ) ;
#1939 = VERTEX_POINT ( 'NONE', #14316 ) ;
#1940 = CARTESIAN_POINT ( 'NONE',  ( -56.13452994616205416, -3.117691453623976816, 1.799999999999788436 ) ) ;
#1941 = CARTESIAN_POINT ( 'NONE',  ( 57.01810253486932112, -0.8103601741748552856, 2.470489098966295316 ) ) ;
#1942 = DIRECTION ( 'NONE',  ( 0.000000000000000000, 0.000000000000000000, -1.000000000000000000 ) ) ;
#1943 = CARTESIAN_POINT ( 'NONE',  ( 58.75000000000003553, -1.800471618824714071, 1.039502773796719959 ) ) ;
#1944 = CARTESIAN_POINT ( 'NONE',  ( -58.28335481156723574, -4.108500314926509134, 1.367561758111407677 ) ) ;
#1945 =( GEOMETRIC_REPRESENTATION_CONTEXT ( 3 ) GLOBAL_UNCERTAINTY_ASSIGNED_CONTEXT ( ( #6994 ) ) GLOBAL_UNIT_ASSIGNED_CONTEXT ( ( #26465, #6678, #26158 ) ) REPRESENTATION_CONTEXT ( 'NONE', 'WORKASPACE' ) );
#1946 =( BOUNDED_SURFACE ( )  B_SPLINE_SURFACE ( 3, 2, ( 
 ( #18514, #3770, #28157 ),
 ( #15673, #20889, #13409 ),
 ( #20745, #30055, #22811 ),
 ( #1097, #3940, #6310 ),
 ( #25624, #16295, #22951 ),
 ( #1406, #1241, #27996 ),
 ( #20431, #8676, #1700 ),
 ( #30694, #25320, #8369 ),
 ( #13581, #1553, #6478 ),
 ( #28325, #11216, #13732 ) ),
 .UNSPECIFIED., .F., .F., .F. ) 
 B_SPLINE_SURFACE_WITH_KNOTS ( ( 4, 2, 2, 2, 4 ),
 ( 3, 3 ),
 ( 0.0004005301535625022482, 0.0008279283193725973976, 0.001041627402277645054, 0.001148476943730168936, 0.001255326485182692601 ),
 ( 0.000000000000000000, 1.000000000000000000 ),
 .UNSPECIFIED. ) 
 GEOMETRIC_REPRESENTATION_ITEM ( )  RATIONAL_B_SPLINE_SURFACE ( (
 ( 1.000000000000000000, 0.7071067811865260344, 1.000000000000000000),
 ( 1.000000000000000000, 0.7463463187144947497, 1.000000000000000000),
 ( 1.000000000000000000, 0.7946150999565809725, 1.000000000000000000),
 ( 1.000000000000000000, 0.8720431506958414847, 1.000000000000000000),
 ( 1.000000000000000000, 0.8987780092778684393, 1.000000000000000000),
 ( 1.000000000000000000, 0.9375340664365204857, 1.000000000000000000),
 ( 1.000000000000000000, 0.9504270566176279411, 1.000000000000000000),
 ( 1.000000000000000000, 0.9732249474031190450, 1.000000000000000000),
 ( 1.000000000000000000, 0.9839441327696822892, 1.000000000000000000),
 ( 1.000000000000000000, 0.9842509842514762797, 1.000000000000000000) ) ) 
 REPRESENTATION_ITEM ( '' )  SURFACE ( )  );
#1948 = DIRECTION ( 'NONE',  ( -0.6819983600625022513, 0.7313537016191670181, 2.468850131082277965E-15 ) ) ;
#1947 = CARTESIAN_POINT ( 'NONE',  ( 48.00000000000001421, -4.416814815491191482, -1.285203052306389981 ) ) ;
#1949 = CARTESIAN_POINT ( 'NONE',  ( 57.05000000000001847, 0.7500000000000000000, -2.489477856900920383 ) ) ;
#1950 = DIRECTION ( 'NONE',  ( -1.000000000000000000, -0.000000000000000000, 3.491481338843133355E-15 ) ) ;
#1951 = CARTESIAN_POINT ( 'NONE',  ( 15.44259799936806488, 5.012895491272638893, -1.399447560527434797 ) ) ;
#1952 = CARTESIAN_POINT ( 'NONE',  ( 58.65000038048068376, -1.663933463835848059, -0.8644232797864647155 ) ) ;
#1953 = CARTESIAN_POINT ( 'NONE',  ( -59.44102194137920492, 2.226395001412990737, 1.446970701571959728 ) ) ;
#1954 = CARTESIAN_POINT ( 'NONE',  ( 52.78861517463008823, 8.494192748968428575, 2.049999999999816858 ) ) ;
#1955 = ORIENTED_EDGE ( 'NONE', *, *, #9126, .T. ) ;
#1957 = CARTESIAN_POINT ( 'NONE',  ( -54.39999999999999147, -1.433333333333339343, 4.054078878802656938 ) ) ;
#1956 = LINE ( 'NONE', #28548, #26629 ) ;
#1958 = FACE_OUTER_BOUND ( 'NONE', #27770, .T. ) ;
#1959 = ORIENTED_EDGE ( 'NONE', *, *, #24978, .F. ) ;
#1960 = DIRECTION ( 'NONE',  ( 3.491481338843133355E-15, -0.000000000000000000, 1.000000000000000000 ) ) ;
#1961 = CARTESIAN_POINT ( 'NONE',  ( 60.75000000000001421, 0.6500000000006350698, -1.489337100860685048 ) ) ;
#1962 = CARTESIAN_POINT ( 'NONE',  ( -59.74999999999995737, 2.023778652682510945E-14, -3.400000000000212186 ) ) ;
#1963 = EDGE_LOOP ( 'NONE', ( #10035, #26095, #29334, #18935, #7350, #21515, #2912 ) ) ;
#1964 = ORIENTED_EDGE ( 'NONE', *, *, #8148, .T. ) ;
#1965 = DIRECTION ( 'NONE',  ( 0.000000000000000000, 0.000000000000000000, 1.000000000000000000 ) ) ;
#1966 = EDGE_LOOP ( 'NONE', ( #11467, #21378, #11264, #28038 ) ) ;
#1967 = EDGE_CURVE ( 'NONE', #31291, #24125, #14030, .T. ) ;
#1968 = CARTESIAN_POINT ( 'NONE',  ( 58.65266784251147669, -1.656109637134997703, 0.8793208749736606267 ) ) ;
#1969 = AXIS2_PLACEMENT_3D ( 'NONE', #23194, #25536, #1317 ) ;
#1970 = CARTESIAN_POINT ( 'NONE',  ( -54.38452994616203995, 2.093608279459366986E-14, -3.600000000000193268 ) ) ;
#1971 = ORIENTED_EDGE ( 'NONE', *, *, #28816, .T. ) ;
#1972 = CARTESIAN_POINT ( 'NONE',  ( 51.80000000000001847, -0.2842225609755594795, -1.577752156565102655E-15 ) ) ;
#1973 = ADVANCED_FACE ( 'NONE', ( #26683 ), #14477, .F. ) ;
#1974 = CARTESIAN_POINT ( 'NONE',  ( 58.65000000000004121, -1.872332544500605378, 0.09997921184723741750 ) ) ;
#1975 = CARTESIAN_POINT ( 'NONE',  ( -54.49400863111429061, -3.204489435302700695, -1.562885166739987008 ) ) ;
#1976 = VERTEX_POINT ( 'NONE', #17476 ) ;
#1977 = ORIENTED_EDGE ( 'NONE', *, *, #30437, .T. ) ;
#1978 = LINE ( 'NONE', #26031, #19825 ) ;
#1979 = DIRECTION ( 'NONE',  ( 1.000000000000000000, 3.053848253006669023E-16, -2.042510438544995415E-16 ) ) ;
#1980 = CARTESIAN_POINT ( 'NONE',  ( 69.00000000000000000, 4.155057991226904698E-16, -3.020710678119368886 ) ) ;
#1981 = ORIENTED_EDGE ( 'NONE', *, *, #21499, .T. ) ;
#1982 = AXIS2_PLACEMENT_3D ( 'NONE', #17687, #3261, #22592 ) ;
#1983 = DIRECTION ( 'NONE',  ( -1.000000000000000000, 1.219044193948983948E-29, -3.491481338843133355E-15 ) ) ;
#1984 = CARTESIAN_POINT ( 'NONE',  ( 68.00000000000000000, 0.5000000000000000000, -1.988246715074070581 ) ) ;
#1985 = ADVANCED_FACE ( 'NONE', ( #25225 ), #849, .F. ) ;
#1986 = CARTESIAN_POINT ( 'NONE',  ( -60.49999999999995737, 1.963826825011730345E-15, 6.704595576490977020E-16 ) ) ;
#1987 = DIRECTION ( 'NONE',  ( -1.000000000000000000, 0.000000000000000000, 0.000000000000000000 ) ) ;
#1988 = DIRECTION ( 'NONE',  ( 0.000000000000000000, 0.000000000000000000, 1.000000000000000000 ) ) ;
#1989 = DIRECTION ( 'NONE',  ( 0.000000000000000000, -0.000000000000000000, 1.000000000000000000 ) ) ;
#1990 = DIRECTION ( 'NONE',  ( 0.000000000000000000, 0.000000000000000000, -1.000000000000000000 ) ) ;
#1991 = CIRCLE ( 'NONE', #12599, 3.499999999999999556 ) ;
#1992 = CARTESIAN_POINT ( 'NONE',  ( 51.25000000000001421, 5.368159983410797313E-13, 3.111507638930570854E-58 ) ) ;
#1993 = VERTEX_POINT ( 'NONE', #10515 ) ;
#1994 = CARTESIAN_POINT ( 'NONE',  ( 58.72153194576635826, 0.5000000000006150636, -1.827449685318863093 ) ) ;
#1995 = VERTEX_POINT ( 'NONE', #22717 ) ;
#1996 = CARTESIAN_POINT ( 'NONE',  ( 53.66376481541393417, 4.683274397263343047, 2.049999999999812861 ) ) ;
#1997 = CARTESIAN_POINT ( 'NONE',  ( -58.09585481156723574, -1.184343223768586473, -3.558065644182725418 ) ) ;
#1999 = CARTESIAN_POINT ( 'NONE',  ( -36.22955757456080761, 3.272340825137115772, 4.050058705652215707 ) ) ;
#1998 = DIRECTION ( 'NONE',  ( 1.000000000000000000, 0.000000000000000000, -0.000000000000000000 ) ) ;
#2000 = ORIENTED_EDGE ( 'NONE', *, *, #3617, .F. ) ;
#2001 = DIRECTION ( 'NONE',  ( 1.000000000000000000, 0.000000000000000000, -1.047444401652940007E-14 ) ) ;
#2002 = ORIENTED_EDGE ( 'NONE', *, *, #26851, .F. ) ;
#2003 = ADVANCED_FACE ( 'NONE', ( #27591 ), #10192, .T. ) ;
#2004 = FACE_OUTER_BOUND ( 'NONE', #18517, .T. ) ;
#2005 = CIRCLE ( 'NONE', #18203, 2.700000000000000178 ) ;
#2006 = VERTEX_POINT ( 'NONE', #29820 ) ;
#2008 = CARTESIAN_POINT ( 'NONE',  ( -59.19999999999996732, 3.264622394567737729, -0.9498634748674483763 ) ) ;
#2007 = CARTESIAN_POINT ( 'NONE',  ( 50.45688046812396976, 1.211457450596386209, 3.917546004217189015 ) ) ;
#2009 = VERTEX_POINT ( 'NONE', #24598 ) ;
#2010 = CARTESIAN_POINT ( 'NONE',  ( 53.78583825613542757, 7.269801125715066092, 1.827185152435081283 ) ) ;
#2011 = FACE_OUTER_BOUND ( 'NONE', #28396, .T. ) ;
#2012 = AXIS2_PLACEMENT_3D ( 'NONE', #25284, #1371, #27494 ) ;
#2013 = CARTESIAN_POINT ( 'NONE',  ( 47.54047041873123902, -4.349936135048430685, 1.496764967786690326 ) ) ;
#2014 = AXIS2_PLACEMENT_3D ( 'NONE', #25807, #25484, #8694 ) ;
#2015 = CARTESIAN_POINT ( 'NONE',  ( -54.39999999999996305, -1.399999999999979039, -3.959797974644881258 ) ) ;
#2016 = CARTESIAN_POINT ( 'NONE',  ( -58.38452994616204705, -3.117691453623976816, 1.799999999999780442 ) ) ;
#2017 = CARTESIAN_POINT ( 'NONE',  ( -59.37009172985672478, 3.234433134214944161, -1.048065980887175952 ) ) ;
#2018 = VECTOR ( 'NONE', #20215, 1000.000000000000000 ) ;
#2019 = ADVANCED_FACE ( 'NONE', ( #5920 ), #17946, .F. ) ;
#2020 = CARTESIAN_POINT ( 'NONE',  ( -59.19999999999997442, -3.371540527096009932, 0.6493167879416990029 ) ) ;
#2021 = CARTESIAN_POINT ( 'NONE',  ( 58.75000000000000711, 1.932246131437593162, 0.4087173687853762338 ) ) ;
#2022 = CARTESIAN_POINT ( 'NONE',  ( -55.79792740578360366, 3.330682475591789427, 0.6830477631804118266 ) ) ;
#2023 = CARTESIAN_POINT ( 'NONE',  ( 61.23770293222972327, 0.8897917884438596436, 1.791164585743606041 ) ) ;
#2024 = ORIENTED_EDGE ( 'NONE', *, *, #17179, .F. ) ;
#2025 = FACE_OUTER_BOUND ( 'NONE', #23862, .T. ) ;
#2026 = CARTESIAN_POINT ( 'NONE',  ( -36.22909104983144601, -0.6969927240738240659, 5.374332520738271057 ) ) ;
#2027 = CARTESIAN_POINT ( 'NONE',  ( -67.91948434493399134, -1.598692187574555446, -0.03982506530960670810 ) ) ;
#2028 = ORIENTED_EDGE ( 'NONE', *, *, #11758, .F. ) ;
#2029 = CARTESIAN_POINT ( 'NONE',  ( -36.79682133506353381, -4.944296796129610705, 2.193698057025720072 ) ) ;
#2030 = ORIENTED_EDGE ( 'NONE', *, *, #6783, .F. ) ;
#2031 = DIRECTION ( 'NONE',  ( 0.04332611568076707997, -0.9990609829735204173, 0.000000000000000000 ) ) ;
#2033 = CARTESIAN_POINT ( 'NONE',  ( 58.74999999305997989, -1.345908541131179081, 1.382203543031325088 ) ) ;
#2032 = CARTESIAN_POINT ( 'NONE',  ( -57.37499999999996447, 2.944486372867110902, -1.700000000000183809 ) ) ;
#2034 = VERTEX_POINT ( 'NONE', #8131 ) ;
#2035 = EDGE_LOOP ( 'NONE', ( #12776, #23464, #28372, #21264 ) ) ;
#2036 = CARTESIAN_POINT ( 'NONE',  ( 53.91574522233626965, 6.672251602764244893, -1.774295313897662485 ) ) ;
#2037 = AXIS2_PLACEMENT_3D ( 'NONE', #3711, #15896, #25554 ) ;
#2038 = EDGE_CURVE ( 'NONE', #2740, #15300, #22545, .T. ) ;
#2039 = DIRECTION ( 'NONE',  ( 1.000000000000000000, 3.053848253006669023E-16, -2.042510438544995415E-16 ) ) ;
#2041 = CARTESIAN_POINT ( 'NONE',  ( -54.49999999999996447, 1.400000000000021450, -3.363870538531680943 ) ) ;
#2040 = DIRECTION ( 'NONE',  ( 0.000000000000000000, 0.000000000000000000, 1.000000000000000000 ) ) ;
#2042 = ORIENTED_EDGE ( 'NONE', *, *, #646, .T. ) ;
#2043 = CARTESIAN_POINT ( 'NONE',  ( -55.81249999999997158, -0.8699069336946620989, 4.241846523238426592 ) ) ;
#2044 = CARTESIAN_POINT ( 'NONE',  ( 33.47623932017462778, 1.123735532908310519, 5.289358697221540950 ) ) ;
#2045 = CARTESIAN_POINT ( 'NONE',  ( 61.25000000000001421, 1.000000000000641709, 1.546164609606623053 ) ) ;
#2046 = EDGE_CURVE ( 'NONE', #11900, #27954, #16272, .T. ) ;
#2047 = CARTESIAN_POINT ( 'NONE',  ( 58.75000000000002132, 6.153735859711025284E-13, 3.111507638930570854E-58 ) ) ;
#2048 = CARTESIAN_POINT ( 'NONE',  ( -59.69464122902330416, 2.086944863889884871, 1.740854861534822273 ) ) ;
#2049 = CARTESIAN_POINT ( 'NONE',  ( 31.58270314793947620, 7.514175884156568230, 1.424999999999890132 ) ) ;
#2050 = CARTESIAN_POINT ( 'NONE',  ( -54.44999999999997442, 1.499999999999999556, -4.029888335921975262 ) ) ;
#2051 = EDGE_LOOP ( 'NONE', ( #18958, #15900, #15848, #30933 ) ) ;
#2052 = EDGE_CURVE ( 'NONE', #14020, #27339, #18813, .T. ) ;
#2053 = CARTESIAN_POINT ( 'NONE',  ( 51.80000000000002558, -3.637377585518695611, 2.099877210782855830 ) ) ;
#2054 = CARTESIAN_POINT ( 'NONE',  ( -36.27260443516960464, 2.900433254920971038, -4.320265374240186418 ) ) ;
#2055 = LINE ( 'NONE', #9194, #17675 ) ;
#2056 = B_SPLINE_CURVE_WITH_KNOTS ( 'NONE', 3,
 ( #26685, #6729, #21326, #11956, #14168, #23693, #26510, #26362, #21796, #23990, #9273, #16872, #12258, #18937, #82, #7208 ),
 .UNSPECIFIED., .F., .F.,
 ( 4, 3, 3, 3, 3, 4 ),
 ( 0.000000000000000000, 3.111139534546023401E-05, 6.583698738123831937E-05, 9.811465807641186142E-05, 0.0001294159172546408877, 0.0001609582457662007114 ),
 .UNSPECIFIED. ) ;
#2057 = DIRECTION ( 'NONE',  ( 0.000000000000000000, 1.000000000000000000, 3.491481338843132961E-15 ) ) ;
#2058 = VECTOR ( 'NONE', #19470, 1000.000000000000000 ) ;
#2059 = CARTESIAN_POINT ( 'NONE',  ( 57.02528775048638465, -0.7434661330690420789, -2.425538622349843632 ) ) ;
#2061 = DIRECTION ( 'NONE',  ( 0.000000000000000000, -1.626303258728255862E-15, 1.000000000000000000 ) ) ;
#2060 = CARTESIAN_POINT ( 'NONE',  ( -55.06684846062113081, -0.2309624077929038066, -3.875409454552791733 ) ) ;
#2062 = EDGE_CURVE ( 'NONE', #20216, #21772, #20343, .T. ) ;
#2063 = CARTESIAN_POINT ( 'NONE',  ( 47.00000000000000711, -3.994423162662119609, -2.070282222600184685 ) ) ;
#2065 = CARTESIAN_POINT ( 'NONE',  ( -59.69999999999996732, -1.873569517744609447, -3.074042495181142698 ) ) ;
#2064 = CARTESIAN_POINT ( 'NONE',  ( -44.49999999999997868, 1.499999999999998890, 3.300094695611021756 ) ) ;
#2066 = ORIENTED_EDGE ( 'NONE', *, *, #28274, .F. ) ;
#2067 = CARTESIAN_POINT ( 'NONE',  ( 58.75000000000004263, -1.922112613533886405, 0.4146634982040790507 ) ) ;
#2068 = CARTESIAN_POINT ( 'NONE',  ( 54.26434950415730896, 6.004763229855418771, -2.050000000000188560 ) ) ;
#2070 = CARTESIAN_POINT ( 'NONE',  ( 47.10000000000002274, 2.428612866367529932E-14, -1.644487710595116631E-13 ) ) ;
#2069 = CARTESIAN_POINT ( 'NONE',  ( 15.29384114148407647, -2.734418404389891144, -4.440882220947494297 ) ) ;
#2071 = CARTESIAN_POINT ( 'NONE',  ( 69.20000000000001705, 0.6617647058823536987, -1.754335336830159076 ) ) ;
#2072 = ORIENTED_EDGE ( 'NONE', *, *, #4979, .F. ) ;
#2073 = ORIENTED_EDGE ( 'NONE', *, *, #11797, .T. ) ;
#2074 = EDGE_CURVE ( 'NONE', #19955, #5910, #15898, .T. ) ;
#2075 = ORIENTED_EDGE ( 'NONE', *, *, #28271, .T. ) ;
#2076 = CARTESIAN_POINT ( 'NONE',  ( 56.96117471280891209, 0.7619384116854249767, -2.485869561276773165 ) ) ;
#2077 = EDGE_CURVE ( 'NONE', #507, #20216, #12900, .T. ) ;
#2078 = CARTESIAN_POINT ( 'NONE',  ( 58.68279620299848176, 0.5000000000006146195, 1.809045707182517004 ) ) ;
#2079 = ORIENTED_EDGE ( 'NONE', *, *, #30465, .T. ) ;
#2080 = EDGE_CURVE ( 'NONE', #23979, #15338, #22392, .T. ) ;
#2081 = CARTESIAN_POINT ( 'NONE',  ( 58.75000018595667939, 1.936190688449842767, -0.04992417795777597672 ) ) ;
#2082 = ORIENTED_EDGE ( 'NONE', *, *, #10520, .T. ) ;
#2083 = CARTESIAN_POINT ( 'NONE',  ( -60.33155989232410121, -1.962990915244706924, -3.400000000000220179 ) ) ;
#2084 = SHAPE_REPRESENTATION_RELATIONSHIP ( 'NONE' , 'NONE' ,  #1561, #15356 ) ;
#2085 = EDGE_LOOP ( 'NONE', ( #4934, #25212, #8117, #15158, #24252, #16329 ) ) ;
#2086 = ORIENTED_EDGE ( 'NONE', *, *, #25090, .T. ) ;
#2087 = CARTESIAN_POINT ( 'NONE',  ( -59.56249999999996447, 3.925981830489463142, -1.971446734091520023E-13 ) ) ;
#2088 = PLANE ( 'NONE',  #22096 ) ;
#2089 = DIRECTION ( 'NONE',  ( -1.047444401652940007E-14, 0.000000000000000000, -1.000000000000000000 ) ) ;
#2090 = CARTESIAN_POINT ( 'NONE',  ( 51.49472959044967268, -1.070956530527746420, -1.224612562803250038 ) ) ;
#2091 = AXIS2_PLACEMENT_3D ( 'NONE', #30693, #30853, #6778 ) ;
#2092 = CARTESIAN_POINT ( 'NONE',  ( 61.00000000000002132, 6.389410850082937196E-13, 3.111507638930570854E-58 ) ) ;
#2093 = AXIS2_PLACEMENT_3D ( 'NONE', #6612, #10880, #6146 ) ;
#2094 = DIRECTION ( 'NONE',  ( 0.000000000000000000, -8.673617379884032317E-15, -1.000000000000000000 ) ) ;
#2095 = EDGE_CURVE ( 'NONE', #20905, #12969, #10805, .T. ) ;
#2096 = CARTESIAN_POINT ( 'NONE',  ( 47.10000000000002274, 6.982261990806648555E-14, -1.632474749424821370E-13 ) ) ;
#2097 = CARTESIAN_POINT ( 'NONE',  ( -60.84461143194913291, -2.333522038737472215, -0.9693817630866828905 ) ) ;
#2098 = CARTESIAN_POINT ( 'NONE',  ( 15.29954477411490821, 5.377732435184259252, -0.5657657035920871103 ) ) ;
#2099 = ORIENTED_EDGE ( 'NONE', *, *, #13067, .F. ) ;
#2100 = DIRECTION ( 'NONE',  ( 1.000000000000000000, 0.000000000000000000, 0.000000000000000000 ) ) ;
#2101 = EDGE_CURVE ( 'NONE', #21049, #9458, #14244, .T. ) ;
#2102 = CARTESIAN_POINT ( 'NONE',  ( 50.40000000000001990, 0.6304760106459518232, -3.950000000000022826 ) ) ;
#2103 = EDGE_LOOP ( 'NONE', ( #1874, #13106, #955, #8764, #22442, #24197 ) ) ;
#2105 = CARTESIAN_POINT ( 'NONE',  ( 50.34875358082581442, -1.383300983803858797, 3.859740869727655621 ) ) ;
#2104 = CARTESIAN_POINT ( 'NONE',  ( 48.37840743871460347, -1.310166284604358244, 3.885185101012172737 ) ) ;
#2106 = CARTESIAN_POINT ( 'NONE',  ( 54.20407241913904528, 5.668441268431575253, -2.050000000000189004 ) ) ;
#2107 = DIRECTION ( 'NONE',  ( 1.000000000000000000, 0.000000000000000000, 0.000000000000000000 ) ) ;
#2108 = AXIS2_PLACEMENT_3D ( 'NONE', #10341, #20014, #7982 ) ;
#2109 = ORIENTED_EDGE ( 'NONE', *, *, #20115, .T. ) ;
#2110 = DIRECTION ( 'NONE',  ( 0.000000000000000000, -0.9996898646859344595, -0.02490330187381124133 ) ) ;
#2111 = DIRECTION ( 'NONE',  ( 1.000000000000000000, -1.219044193948983948E-29, 3.491481338843133355E-15 ) ) ;
#2112 = CARTESIAN_POINT ( 'NONE',  ( -60.24999999999997158, 2.944486372867092250, 1.699999999999797673 ) ) ;
#2113 = ORIENTED_EDGE ( 'NONE', *, *, #18597, .F. ) ;
#2114 = EDGE_LOOP ( 'NONE', ( #16744, #13809, #12837, #23029 ) ) ;
#2115 = EDGE_CURVE ( 'NONE', #19132, #7871, #593, .T. ) ;
#2116 = CARTESIAN_POINT ( 'NONE',  ( -59.53611077946203523, 3.324882312671999518, -1.143917123867393304 ) ) ;
#2117 = ORIENTED_EDGE ( 'NONE', *, *, #14849, .F. ) ;
#2118 = CARTESIAN_POINT ( 'NONE',  ( 51.80056040574818610, 4.600011524547849895, -0.2639097402654416724 ) ) ;
#2119 = AXIS2_PLACEMENT_3D ( 'NONE', #12111, #21793, #7351 ) ;
#2120 = CARTESIAN_POINT ( 'NONE',  ( -54.69702994616206837, -2.078460969082657872, 3.599999999999797584 ) ) ;
#2121 = EDGE_LOOP ( 'NONE', ( #1483, #30560, #19045, #30745 ) ) ;
#2122 = DIRECTION ( 'NONE',  ( -1.000000000000000000, 0.000000000000000000, 0.000000000000000000 ) ) ;
#2123 = CARTESIAN_POINT ( 'NONE',  ( -59.53056271719990633, -2.463209972446139595, -1.140713948626901120 ) ) ;
#2124 = CARTESIAN_POINT ( 'NONE',  ( 54.40000000000001990, 0.000000000000000000, -3.299999999999999822 ) ) ;
#2125 = ORIENTED_EDGE ( 'NONE', *, *, #2514, .T. ) ;
#2126 = VERTEX_POINT ( 'NONE', #535 ) ;
#2127 =( BOUNDED_SURFACE ( )  B_SPLINE_SURFACE ( 3, 2, ( 
 ( #30225, #8531, #18217 ),
 ( #6167, #25465, #2181 ),
 ( #2348, #9172, #19159 ),
 ( #16770, #12014, #4411 ),
 ( #21696, #31161, #7415 ),
 ( #21222, #28798, #31320 ),
 ( #18835, #7110, #4243 ),
 ( #9496, #14540, #11546 ),
 ( #26414, #9787, #11847 ),
 ( #19455, #28639, #14060 ) ),
 .UNSPECIFIED., .F., .F., .F. ) 
 B_SPLINE_SURFACE_WITH_KNOTS ( ( 4, 2, 2, 2, 4 ),
 ( 3, 3 ),
 ( 0.0001706658715691171911, 0.0002229276920778207674, 0.0002751895125865243437, 0.0003274513330952279200, 0.0003797131536039315505 ),
 ( 0.000000000000000000, 1.000000000000000000 ),
 .UNSPECIFIED. ) 
 GEOMETRIC_REPRESENTATION_ITEM ( )  RATIONAL_B_SPLINE_SURFACE ( (
 ( 1.000000000000000000, 0.7071067811865445751, 1.000000000000000000),
 ( 1.000000000000000000, 0.7375607040702577555, 1.000000000000000000),
 ( 1.000000000000000000, 0.7730431127429812088, 1.000000000000000000),
 ( 1.000000000000000000, 0.8321012486994131541, 1.000000000000000000),
 ( 1.000000000000000000, 0.8541932017417729339, 1.000000000000000000),
 ( 1.000000000000000000, 0.8545723906072647535, 1.000000000000000000),
 ( 1.000000000000000000, 0.8327032135058914930, 1.000000000000000000),
 ( 1.000000000000000000, 0.7734559727064781454, 1.000000000000000000),
 ( 1.000000000000000000, 0.7377766653997793744, 1.000000000000000000),
 ( 1.000000000000000000, 0.7071067811865466846, 1.000000000000000000) ) ) 
 REPRESENTATION_ITEM ( '' )  SURFACE ( )  );
#2128 = DIRECTION ( 'NONE',  ( 1.000000000000000000, 3.054025858079668409E-16, -2.042474015755241579E-16 ) ) ;
#2129 = CARTESIAN_POINT ( 'NONE',  ( -62.09999999999997300, -2.678008572308610002, 0.1572561257273979995 ) ) ;
#2130 = CARTESIAN_POINT ( 'NONE',  ( 58.75000000000002842, -0.8948927608030053937, -1.760622601996600922 ) ) ;
#2131 = VERTEX_POINT ( 'NONE', #683 ) ;
#2132 = ADVANCED_BREP_SHAPE_REPRESENTATION ( '', ( #25333, #9018 ), #22713 ) ;
#2133 = FACE_OUTER_BOUND ( 'NONE', #19427, .T. ) ;
#2134 = DIRECTION ( 'NONE',  ( -0.000000000000000000, -0.000000000000000000, -1.000000000000000000 ) ) ;
#2135 = CARTESIAN_POINT ( 'NONE',  ( -54.39999999999996305, -1.499999999999981126, -3.363870538531691601 ) ) ;
#2136 = CARTESIAN_POINT ( 'NONE',  ( 50.40000000000001990, -4.899999999999999467, -4.100000000000022737 ) ) ;
#2137 = EDGE_CURVE ( 'NONE', #22777, #5429, #20332, .T. ) ;
#2138 = CARTESIAN_POINT ( 'NONE',  ( 51.47729133425610115, 0.9526829978902818796, 1.321356857234310178 ) ) ;
#2139 = ADVANCED_FACE ( 'NONE', ( #29657 ), #17646, .F. ) ;
#2140 = CARTESIAN_POINT ( 'NONE',  ( 34.50000000000001421, 0.000000000000000000, 0.000000000000000000 ) ) ;
#2141 = CARTESIAN_POINT ( 'NONE',  ( 58.50000000000001421, 0.8000000000000000444, 2.421260002560649660 ) ) ;
#2142 = ADVANCED_FACE ( 'NONE', ( #18740 ), #25522, .F. ) ;
#2143 = ORIENTED_EDGE ( 'NONE', *, *, #12156, .T. ) ;
#2144 = ORIENTED_EDGE ( 'NONE', *, *, #28819, .F. ) ;
#2145 = DIRECTION ( 'NONE',  ( 0.000000000000000000, 0.000000000000000000, 1.000000000000000000 ) ) ;
#2146 = ORIENTED_EDGE ( 'NONE', *, *, #31322, .T. ) ;
#2147 = CARTESIAN_POINT ( 'NONE',  ( 54.23701917430469877, 5.946187982713466269, 2.049999999999810640 ) ) ;
#2148 = AXIS2_PLACEMENT_3D ( 'NONE', #14226, #29110, #24216 ) ;
#2149 = CARTESIAN_POINT ( 'NONE',  ( -56.29792740578360366, -2.256877952708263635, 2.542931754211924300 ) ) ;
#2151 = CARTESIAN_POINT ( 'NONE',  ( -36.56390771145526486, 3.008101665203156028, 4.495550615867659694 ) ) ;
#2150 = CARTESIAN_POINT ( 'NONE',  ( 58.75000000000002842, -1.039502773796102897, -1.800471618824325493 ) ) ;
#2152 = ORIENTED_EDGE ( 'NONE', *, *, #24073, .T. ) ;
#2153 = LINE ( 'NONE', #28915, #3277 ) ;
#2154 = ORIENTED_EDGE ( 'NONE', *, *, #14114, .T. ) ;
#2155 = EDGE_CURVE ( 'NONE', #20739, #26219, #22857, .T. ) ;
#2156 = DIRECTION ( 'NONE',  ( 1.000000000000000000, 1.047444401652940007E-14, 0.000000000000000000 ) ) ;
#2157 = VERTEX_POINT ( 'NONE', #4300 ) ;
#2159 = FACE_BOUND ( 'NONE', #15755, .T. ) ;
#2158 = CARTESIAN_POINT ( 'NONE',  ( 50.39865716130687190, 0.9106118309513187015, 3.923752762110599424 ) ) ;
#2160 = ORIENTED_EDGE ( 'NONE', *, *, #24446, .T. ) ;
#2161 = CARTESIAN_POINT ( 'NONE',  ( -71.49999999999998579, 0.9743475445367603127, -4.751120590182400960 ) ) ;
#2162 = CARTESIAN_POINT ( 'NONE',  ( 57.05000000000001847, 0.7500000000000000000, 1.778341924377873751 ) ) ;
#2163 = CARTESIAN_POINT ( 'NONE',  ( -54.49983832461118283, -1.542920080254277959, -3.327619142904491234 ) ) ;
#2164 = CARTESIAN_POINT ( 'NONE',  ( 51.14630318392394770, 0.9364487020639118420, -1.503522130792751987 ) ) ;
#2165 = CARTESIAN_POINT ( 'NONE',  ( -56.50952994616203995, 3.117691453623994580, -1.800000000000187006 ) ) ;
#2166 = DIRECTION ( 'NONE',  ( 1.000000000000000000, 0.000000000000000000, -1.047444401652940007E-14 ) ) ;
#2167 = CARTESIAN_POINT ( 'NONE',  ( 56.95000000000001705, 0.000000000000000000, 0.000000000000000000 ) ) ;
#2168 = CARTESIAN_POINT ( 'NONE',  ( -56.19184846062112371, 0.2309624077929113561, 3.875409454552790844 ) ) ;
#2169 = AXIS2_PLACEMENT_3D ( 'NONE', #4645, #17626, #19994 ) ;
#2170 = CARTESIAN_POINT ( 'NONE',  ( 51.31572262954153985, -0.7526089581371979698, -1.996089927833914146 ) ) ;
#2171 = EDGE_CURVE ( 'NONE', #19277, #10332, #22348, .T. ) ;
#2172 = CARTESIAN_POINT ( 'NONE',  ( -59.19999999999997442, 4.156921938165317520, -0.9498634748674451567 ) ) ;
#2173 = ORIENTED_EDGE ( 'NONE', *, *, #11386, .F. ) ;
#2174 = CARTESIAN_POINT ( 'NONE',  ( 57.05000000000001137, -0.7500000000000000000, -2.421260002560653213 ) ) ;
#2175 = CARTESIAN_POINT ( 'NONE',  ( -36.04581030752768811, -0.7747498452693805104, 5.363501451415725541 ) ) ;
#2176 = CARTESIAN_POINT ( 'NONE',  ( 53.81464057712625504, 5.799094425976106137, 0.8364386040616162976 ) ) ;
#2177 = ORIENTED_EDGE ( 'NONE', *, *, #6013, .T. ) ;
#2178 = CARTESIAN_POINT ( 'NONE',  ( -54.47328085509070661, 1.505517457405397996, 4.033720452520547894 ) ) ;
#2179 = EDGE_LOOP ( 'NONE', ( #21179, #29517, #30612, #21844 ) ) ;
#2180 = CARTESIAN_POINT ( 'NONE',  ( 15.44259799936805422, 0.2181161761757584028, -5.200000001420963969 ) ) ;
#2182 = CARTESIAN_POINT ( 'NONE',  ( 58.72200624034191208, -1.341335979946730816, 1.310319377727102497 ) ) ;
#2181 = CARTESIAN_POINT ( 'NONE',  ( 58.65000038048047060, 0.8644232797865400997, -1.663933463836744231 ) ) ;
#2183 = ORIENTED_EDGE ( 'NONE', *, *, #11013, .T. ) ;
#2184 = EDGE_LOOP ( 'NONE', ( #27777, #22817, #4422, #9131, #26467 ) ) ;
#2185 = DIRECTION ( 'NONE',  ( 3.489354422748178582E-15, -1.218509414717996338E-16, 1.000000000000000000 ) ) ;
#2186 = EDGE_CURVE ( 'NONE', #22413, #3208, #15560, .T. ) ;
#2187 = DIRECTION ( 'NONE',  ( -1.000000000000000000, -3.053848253006669023E-16, 2.042510438544995415E-16 ) ) ;
#2189 = CARTESIAN_POINT ( 'NONE',  ( 58.65000000000000568, 0.8495817349399593654, 1.671477153794648896 ) ) ;
#2188 = CARTESIAN_POINT ( 'NONE',  ( 58.65815574817776223, -0.5272471384221183444, 1.799565140951959963 ) ) ;
#2190 = VERTEX_POINT ( 'NONE', #30280 ) ;
#2191 = CARTESIAN_POINT ( 'NONE',  ( -55.06249999999997158, -0.8699069336946619879, 4.241846523238426592 ) ) ;
#2192 = CIRCLE ( 'NONE', #25448, 2.525000000000001243 ) ;
#2193 = CYLINDRICAL_SURFACE ( 'NONE', #27936, 0.04999999999999991257 ) ;
#2194 = CARTESIAN_POINT ( 'NONE',  ( -37.18272003341174070, -1.653865106024005477E-14, 0.000000000000000000 ) ) ;
#2195 = CARTESIAN_POINT ( 'NONE',  ( -55.51905989232413674, 2.944486372867090029, 1.699999999999817213 ) ) ;
#2196 = ITEM_DEFINED_TRANSFORMATION ( 'NONE', 'NONE', #30297,  #9018 ) ;
#2197 = CARTESIAN_POINT ( 'NONE',  ( -61.36380732660158799, -2.615533412885217679, -0.6059315537932544737 ) ) ;
#2198 = DIRECTION ( 'NONE',  ( 0.000000000000000000, 0.000000000000000000, 1.000000000000000000 ) ) ;
#2199 = DIRECTION ( 'NONE',  ( 1.000000000000000000, 0.000000000000000000, -4.738179285253022937E-16 ) ) ;
#2201 = ORIENTED_EDGE ( 'NONE', *, *, #1606, .T. ) ;
#2200 = EDGE_CURVE ( 'NONE', #11901, #24741, #8672, .T. ) ;
#2202 = CARTESIAN_POINT ( 'NONE',  ( 57.00320971560400096, -0.7176258130632211518, 1.806074485252040285 ) ) ;
#2203 = CARTESIAN_POINT ( 'NONE',  ( -57.31249999999996447, 3.400000000000008349, -1.881930883448047941E-13 ) ) ;
#2204 = CARTESIAN_POINT ( 'NONE',  ( 58.75000000000000000, 2.079005547593415937, 1.004182178118534636E-12 ) ) ;
#2205 = CARTESIAN_POINT ( 'NONE',  ( 49.00000000000000000, -0.6617647058823530326, -1.754335336829947023 ) ) ;
#2206 = B_SPLINE_CURVE_WITH_KNOTS ( 'NONE', 3,
 ( #22940, #20578, #10593, #22468, #24832, #19939, #8061, #7891, #27687, #29573, #3471, #3148, #13109, #12788, #8210, #13398, #6006, #17727, #20419 ),
 .UNSPECIFIED., .F., .F.,
 ( 4, 3, 3, 3, 3, 3, 4 ),
 ( 0.000000000000000000, 1.471960608404945498E-05, 2.936908138775499782E-05, 4.497395798386056491E-05, 6.315917083330130442E-05, 8.519491945895780777E-05, 8.667572485204612181E-05 ),
 .UNSPECIFIED. ) ;
#2207 = CARTESIAN_POINT ( 'NONE',  ( 57.03559403007977124, -0.7482252654948684523, -2.422430812887707230 ) ) ;
#2208 = EDGE_CURVE ( 'NONE', #4977, #1831, #29745, .T. ) ;
#2210 = DIRECTION ( 'NONE',  ( 1.000000000000000000, 1.047444401652940007E-14, 0.000000000000000000 ) ) ;
#2209 = CARTESIAN_POINT ( 'NONE',  ( -61.58550117504142918, -2.616993147716194290, 0.3722059216910014179 ) ) ;
#2211 = AXIS2_PLACEMENT_3D ( 'NONE', #28907, #7217, #95 ) ;
#2212 = EDGE_CURVE ( 'NONE', #29156, #28572, #6857, .T. ) ;
#2213 = CARTESIAN_POINT ( 'NONE',  ( -62.06826892193116407, -2.655650422564618474, -0.3277852898564783124 ) ) ;
#2215 = CARTESIAN_POINT ( 'NONE',  ( -55.06249999999997158, 3.400000000000007905, -1.826733775103631524E-13 ) ) ;
#2214 = DIRECTION ( 'NONE',  ( -0.000000000000000000, -0.000000000000000000, -1.000000000000000000 ) ) ;
#2216 = ORIENTED_EDGE ( 'NONE', *, *, #635, .T. ) ;
#2217 = LINE ( 'NONE', #11881, #7261 ) ;
#2218 = CARTESIAN_POINT ( 'NONE',  ( 51.25000000000002842, -1.099999999999462963, 1.196087371390569087 ) ) ;
#2220 = LINE ( 'NONE', #1919, #29290 ) ;
#2219 = CARTESIAN_POINT ( 'NONE',  ( -59.69999999999997442, 3.400000000000007905, -2.001823990013003858E-13 ) ) ;
#2221 = CARTESIAN_POINT ( 'NONE',  ( 16.07512358269929464, -5.037778396015496263, 1.970103387724016386 ) ) ;
#2222 = VERTEX_POINT ( 'NONE', #11267 ) ;
#2223 = ORIENTED_EDGE ( 'NONE', *, *, #30510, .T. ) ;
#2224 = CARTESIAN_POINT ( 'NONE',  ( 51.35647303904148231, -1.001029238032807633, -1.398203054920482025 ) ) ;
#2225 = EDGE_CURVE ( 'NONE', #29589, #67, #17282, .T. ) ;
#2226 = EDGE_LOOP ( 'NONE', ( #14269, #5947, #13939, #7004 ) ) ;
#2227 = CARTESIAN_POINT ( 'NONE',  ( 57.02825620192501077, 0.8138444489294278661, -2.469346200785457413 ) ) ;
#2228 = CARTESIAN_POINT ( 'NONE',  ( 58.67159525762672700, 0.5000000000007230883, 1.807104036850089468 ) ) ;
#2229 = ORIENTED_EDGE ( 'NONE', *, *, #25840, .T. ) ;
#2230 = LINE ( 'NONE', #11895, #29634 ) ;
#2231 = EDGE_LOOP ( 'NONE', ( #12494, #26433, #20885, #23045, #6777, #24843 ) ) ;
#2232 = SURFACE_STYLE_FILL_AREA ( #21893 ) ;
#2233 = CARTESIAN_POINT ( 'NONE',  ( -59.89405989232412963, -3.920666489018293080E-15, 3.399999999999786304 ) ) ;
#2234 = CIRCLE ( 'NONE', #31053, 0.04999999999999989175 ) ;
#2235 = EDGE_CURVE ( 'NONE', #22264, #27880, #25361, .T. ) ;
#2236 = ORIENTED_EDGE ( 'NONE', *, *, #11052, .T. ) ;
#2237 = B_SPLINE_CURVE_WITH_KNOTS ( 'NONE', 3,
 ( #11135, #20811, #30132, #1622, #10989, #18434, #20669, #18135 ),
 .UNSPECIFIED., .F., .F.,
 ( 4, 2, 2, 4 ),
 ( 0.001352388525252836175, 0.001863402819022369787, 0.002374417112791903615, 0.003396445700330970839 ),
 .UNSPECIFIED. ) ;
#2238 = CARTESIAN_POINT ( 'NONE',  ( -54.44702994616203995, -2.078460969082631227, -3.600000000000199485 ) ) ;
#2239 = CARTESIAN_POINT ( 'NONE',  ( -54.44999999999997442, 5.755839955992559655E-16, -4.700000000000000178 ) ) ;
#2240 = CARTESIAN_POINT ( 'NONE',  ( -60.59999999999997300, -2.458552378503722657, 0.9390651652154902163 ) ) ;
#2241 = AXIS2_PLACEMENT_3D ( 'NONE', #20904, #4257, #28659 ) ;
#2242 = DIRECTION ( 'NONE',  ( 0.000000000000000000, -1.000000000000000000, 0.000000000000000000 ) ) ;
#2243 = CARTESIAN_POINT ( 'NONE',  ( -60.59540624230464090, -2.407984592044280614, -1.061968112081668192 ) ) ;
#2244 = EDGE_CURVE ( 'NONE', #19839, #15713, #16035, .T. ) ;
#2246 = CARTESIAN_POINT ( 'NONE',  ( -35.85663232820584057, -3.056483311920867862, 4.206888370749728878 ) ) ;
#2245 = CARTESIAN_POINT ( 'NONE',  ( 15.03925126672132961, 1.123735532908280765, -5.289358697221546279 ) ) ;
#2247 = EDGE_CURVE ( 'NONE', #28320, #20006, #21853, .T. ) ;
#2248 = EDGE_CURVE ( 'NONE', #9056, #12796, #6654, .T. ) ;
#2249 = CIRCLE ( 'NONE', #12863, 1.625000000000000222 ) ;
#2250 = DIRECTION ( 'NONE',  ( 0.000000000000000000, -0.9996898646859343485, -0.02490330187381143562 ) ) ;
#2251 = PLANE ( 'NONE',  #17506 ) ;
#2252 = CARTESIAN_POINT ( 'NONE',  ( 67.99999999999997158, -1.025519176787267142E-28, -3.500000000000711875 ) ) ;
#2253 = VERTEX_POINT ( 'NONE', #26633 ) ;
#2254 = DIRECTION ( 'NONE',  ( 1.000000000000000000, 1.047444401652940007E-14, 0.000000000000000000 ) ) ;
#2255 = AXIS2_PLACEMENT_3D ( 'NONE', #14695, #24356, #31005 ) ;
#2256 = DIRECTION ( 'NONE',  ( 1.000000000000000000, 0.000000000000000000, -1.047444401652940007E-14 ) ) ;
#2258 = CARTESIAN_POINT ( 'NONE',  ( 50.40896409817931101, -1.199904535326220767, 3.921111011342365060 ) ) ;
#2257 = CARTESIAN_POINT ( 'NONE',  ( 48.37893541770432648, -0.9199776782965987110, 3.998258245321878235 ) ) ;
#2259 = CARTESIAN_POINT ( 'NONE',  ( 54.40859250694163052, 6.718200028317722783, -1.988253509196054036 ) ) ;
#2260 = LINE ( 'NONE', #26488, #13429 ) ;
#2261 = EDGE_CURVE ( 'NONE', #24391, #2569, #19237, .T. ) ;
#2262 = EDGE_LOOP ( 'NONE', ( #1555, #13342, #20827, #1981 ) ) ;
#2263 = CIRCLE ( 'NONE', #18464, 0.1000000000000000472 ) ;
#2264 = CARTESIAN_POINT ( 'NONE',  ( 58.65000000000001279, 0.6121634413844184719, -1.877732920580865272 ) ) ;
#2265 = CARTESIAN_POINT ( 'NONE',  ( -43.84599839145305111, 4.786668705877430874, 0.000000000000000000 ) ) ;
#2266 = CARTESIAN_POINT ( 'NONE',  ( -54.75952994616206837, -4.643455692769931152E-15, 3.599999999999804245 ) ) ;
#2268 = ORIENTED_EDGE ( 'NONE', *, *, #21431, .T. ) ;
#2267 = B_SPLINE_CURVE_WITH_KNOTS ( 'NONE', 3,
 ( #9388, #7175, #4477, #21599, #14128, #11759, #23803, #16515 ),
 .UNSPECIFIED., .F., .F.,
 ( 4, 2, 2, 4 ),
 ( 0.000000000000000000, 0.0001089356377969812170, 0.0001634034566954674752, 0.0002178712755939534894 ),
 .UNSPECIFIED. ) ;
#2269 = ORIENTED_EDGE ( 'NONE', *, *, #25539, .T. ) ;
#2270 = CARTESIAN_POINT ( 'NONE',  ( -59.56618930482535745, 3.265896025948629600, -1.161282968582738162 ) ) ;
#2271 = ORIENTED_EDGE ( 'NONE', *, *, #7399, .F. ) ;
#2272 = CARTESIAN_POINT ( 'NONE',  ( 51.83526099861352776, 4.481294105856048482, -1.046211687970766580 ) ) ;
#2273 = CARTESIAN_POINT ( 'NONE',  ( -54.75952994616206837, -4.643455692769931152E-15, 3.599999999999804245 ) ) ;
#2274 = ORIENTED_EDGE ( 'NONE', *, *, #29608, .F. ) ;
#2275 = DIRECTION ( 'NONE',  ( 1.000000000000000000, -0.000000000000000000, -1.047444401652940007E-14 ) ) ;
#2276 =( BOUNDED_SURFACE ( )  B_SPLINE_SURFACE ( 3, 2, ( 
 ( #1792, #16224, #18611 ),
 ( #30610, #11469, #13519 ),
 ( #6712, #30307, #21312 ),
 ( #18920, #16374, #8617 ),
 ( #18293, #13983, #13347 ),
 ( #8757, #23040, #4026 ),
 ( #8924, #16067, #28409 ),
 ( #25719, #28561, #1968 ),
 ( #27933, #11633, #21152 ),
 ( #28254, #30941, #6564 ) ),
 .UNSPECIFIED., .F., .F., .F. ) 
 B_SPLINE_SURFACE_WITH_KNOTS ( ( 4, 2, 2, 2, 4 ),
 ( 3, 3 ),
 ( 0.0001706658715701343896, 0.0002229276920781098699, 0.0002751895125860853502, 0.0003274513330940608848, 0.0003797131536020363651 ),
 ( 0.000000000000000000, 1.000000000000000000 ),
 .UNSPECIFIED. ) 
 GEOMETRIC_REPRESENTATION_ITEM ( )  RATIONAL_B_SPLINE_SURFACE ( (
 ( 1.000000000000000000, 0.7071067811873458231, 1.000000000000000000),
 ( 1.000000000000000000, 0.7375607040708066497, 1.000000000000000000),
 ( 1.000000000000000000, 0.7730431127427257465, 1.000000000000000000),
 ( 1.000000000000000000, 0.8321012486970551514, 1.000000000000000000),
 ( 1.000000000000000000, 0.8541932017381971276, 1.000000000000000000),
 ( 1.000000000000000000, 0.8545723906028362959, 1.000000000000000000),
 ( 1.000000000000000000, 0.8327032135022484072, 1.000000000000000000),
 ( 1.000000000000000000, 0.7734559727053097467, 1.000000000000000000),
 ( 1.000000000000000000, 0.7377766653992025025, 1.000000000000000000),
 ( 1.000000000000000000, 0.7071067811865759944, 1.000000000000000000) ) ) 
 REPRESENTATION_ITEM ( '' )  SURFACE ( )  );
#2277 = CARTESIAN_POINT ( 'NONE',  ( 51.23644008536124517, -1.080112125195908046, 1.214076932077873039 ) ) ;
#2278 = EDGE_CURVE ( 'NONE', #4498, #9785, #4044, .T. ) ;
#2279 = AXIS2_PLACEMENT_3D ( 'NONE', #9892, #19568, #29213 ) ;
#2280 = CARTESIAN_POINT ( 'NONE',  ( 31.37624803221882175, 7.388935654832296862, 1.949999999999890710 ) ) ;
#2281 = ORIENTED_EDGE ( 'NONE', *, *, #4470, .F. ) ;
#2282 = CARTESIAN_POINT ( 'NONE',  ( -77.29999999999998295, -3.473832742311974792E-15, 5.302342620690189014E-15 ) ) ;
#2283 = ADVANCED_FACE ( 'NONE', ( #7016 ), #29163, .T. ) ;
#2284 = DIRECTION ( 'NONE',  ( -1.144559819201192819E-14, 0.000000000000000000, -1.000000000000000000 ) ) ;
#2286 = CARTESIAN_POINT ( 'NONE',  ( -60.59999999999997300, -2.471065902200942688, 0.9400020572919363104 ) ) ;
#2285 = CIRCLE ( 'NONE', #15922, 0.1000000000000001027 ) ;
#2287 = ORIENTED_EDGE ( 'NONE', *, *, #26051, .T. ) ;
#2288 = CARTESIAN_POINT ( 'NONE',  ( -59.40743313238012036, 2.395752775956333291, 1.250136525132548027 ) ) ;
#2289 = PLANE ( 'NONE',  #13484 ) ;
#2290 = AXIS2_PLACEMENT_3D ( 'NONE', #12031, #18847, #14381 ) ;
#2292 = CARTESIAN_POINT ( 'NONE',  ( 50.87477060347629987, 8.633605004120575188, -1.550000000000176792 ) ) ;
#2291 = CARTESIAN_POINT ( 'NONE',  ( -59.51024032614731851, 3.088598804228899652, 1.421463128792039843 ) ) ;
#2293 = EDGE_CURVE ( 'NONE', #23458, #29895, #18212, .T. ) ;
#2294 = EDGE_CURVE ( 'NONE', #10074, #9283, #26165, .T. ) ;
#2295 = CARTESIAN_POINT ( 'NONE',  ( 51.02976068049071756, 1.019450805965458340, 1.268081568884036114 ) ) ;
#2296 = DIRECTION ( 'NONE',  ( 1.047444401652940007E-14, 0.000000000000000000, 1.000000000000000000 ) ) ;
#2297 = DIRECTION ( 'NONE',  ( 1.000000000000000000, 1.047444401652940007E-14, 0.000000000000000000 ) ) ;
#2298 = ORIENTED_EDGE ( 'NONE', *, *, #16497, .F. ) ;
#2299 = CIRCLE ( 'NONE', #12395, 0.1500000000000001887 ) ;
#2300 = AXIS2_PLACEMENT_3D ( 'NONE', #28066, #25857, #6384 ) ;
#2301 = ORIENTED_EDGE ( 'NONE', *, *, #27476, .F. ) ;
#2302 = CARTESIAN_POINT ( 'NONE',  ( -59.11588618124505246, -2.336267030162283653, 1.253430707195199334 ) ) ;
#2303 = ORIENTED_EDGE ( 'NONE', *, *, #10658, .F. ) ;
#2304 = CARTESIAN_POINT ( 'NONE',  ( 53.90445947017991557, 7.548890922513427526, 2.049999999999810196 ) ) ;
#2305 = CARTESIAN_POINT ( 'NONE',  ( -59.97085481156722864, 1.184343223768590470, 3.558065644182727638 ) ) ;
#2307 = DIRECTION ( 'NONE',  ( -0.8787808829753843698, -0.4772254810013855097, 3.008227586482355247E-15 ) ) ;
#2306 = CARTESIAN_POINT ( 'NONE',  ( -35.85663232820584057, 2.686240680702099759, 4.475885388010746979 ) ) ;
#2308 = ORIENTED_EDGE ( 'NONE', *, *, #28100, .T. ) ;
#2309 = VERTEX_POINT ( 'NONE', #24103 ) ;
#2310 = CARTESIAN_POINT ( 'NONE',  ( 69.20000000000001705, -0.7500000000000000000, -1.988246715074082793 ) ) ;
#2311 = ORIENTED_EDGE ( 'NONE', *, *, #21252, .F. ) ;
#2312 = AXIS2_PLACEMENT_3D ( 'NONE', #26682, #22092, #22247 ) ;
#2313 = CARTESIAN_POINT ( 'NONE',  ( 22.09275828236362571, 6.785783592403104691, 1.949999999999922018 ) ) ;
#2314 =( BOUNDED_CURVE ( )  B_SPLINE_CURVE ( 2, ( #10539, #5778, #3418, #7543, #17204, #410, #5472, #5153, #17668 ),
 .UNSPECIFIED., .F., .T. ) 
 B_SPLINE_CURVE_WITH_KNOTS ( ( 3, 2, 2, 2, 3 ),
 ( 0.2500000000000000000, 0.2592592592592592449, 0.2777777777777777901, 0.2962962962962962798, 0.3055555555555555802 ),
 .UNSPECIFIED. ) 
 CURVE ( )  GEOMETRIC_REPRESENTATION_ITEM ( )  RATIONAL_B_SPLINE_CURVE ( ( 0.9330127018922192983, 0.9330127018922194093, 1.000000000000000000, 0.8660254037844387076, 1.000000000000000000, 0.8660254037844387076, 1.000000000000000000, 0.9330127018922191873, 0.9330127018922194093 ) ) 
 REPRESENTATION_ITEM ( '' )  );
#2315 = ORIENTED_EDGE ( 'NONE', *, *, #3799, .T. ) ;
#2316 = CARTESIAN_POINT ( 'NONE',  ( 58.65000000000004121, -1.590093208332549413, 0.9941784314378853127 ) ) ;
#2317 = AXIS2_PLACEMENT_3D ( 'NONE', #23251, #22931, #30357 ) ;
#2318 = ORIENTED_EDGE ( 'NONE', *, *, #23511, .F. ) ;
#2319 = CARTESIAN_POINT ( 'NONE',  ( 53.88560544134391961, 6.996383340473027346, 1.802989201814990894 ) ) ;
#2320 = ADVANCED_FACE ( 'NONE', ( #26791 ), #10012, .F. ) ;
#2321 = CARTESIAN_POINT ( 'NONE',  ( 57.00000000000001421, 0.6999999999999999556, 1.820027472320129736 ) ) ;
#2322 = ADVANCED_FACE ( 'NONE', ( #16982 ), #491, .T. ) ;
#2323 = CARTESIAN_POINT ( 'NONE',  ( 47.20956584626475916, -4.226158602834445333, 1.819860353018571297 ) ) ;
#2324 = DIRECTION ( 'NONE',  ( 1.000000000000000000, 2.586136946169074517E-16, -0.000000000000000000 ) ) ;
#2325 = EDGE_CURVE ( 'NONE', #9593, #10413, #9631, .T. ) ;
#2326 = CARTESIAN_POINT ( 'NONE',  ( -56.39405989232412253, 2.944486372867106461, -1.700000000000187583 ) ) ;
#2327 = DIRECTION ( 'NONE',  ( -1.000000000000000000, 0.000000000000000000, 1.047444401652940007E-14 ) ) ;
#2328 = CIRCLE ( 'NONE', #6366, 3.500000000000000000 ) ;
#2329 = CIRCLE ( 'NONE', #22049, 0.2500000000000002220 ) ;
#2330 = DIRECTION ( 'NONE',  ( 0.000000000000000000, 0.000000000000000000, -1.000000000000000000 ) ) ;
#2331 = CARTESIAN_POINT ( 'NONE',  ( 57.05000000000001847, 0.7500000000000000000, -1.778341924377873751 ) ) ;
#2332 = AXIS2_PLACEMENT_3D ( 'NONE', #23085, #1381, #15792 ) ;
#2333 = AXIS2_PLACEMENT_3D ( 'NONE', #7561, #19610, #16906 ) ;
#2334 = AXIS2_PLACEMENT_3D ( 'NONE', #29970, #27291, #5607 ) ;
#2335 = CARTESIAN_POINT ( 'NONE',  ( -59.68658240507107138, -2.223882124562203799, 1.531065007683262591 ) ) ;
#2336 = VECTOR ( 'NONE', #6657, 1000.000000000000000 ) ;
#2337 = CIRCLE ( 'NONE', #20052, 3.750000000000000444 ) ;
#2338 = CARTESIAN_POINT ( 'NONE',  ( -36.92398358572908990, -0.2875137064282174415, 5.407399902318747564 ) ) ;
#2339 = ORIENTED_EDGE ( 'NONE', *, *, #5681, .F. ) ;
#2340 = CARTESIAN_POINT ( 'NONE',  ( 56.95000000000001705, 0.6820512820512819596, 1.773360101234998210 ) ) ;
#2341 = CARTESIAN_POINT ( 'NONE',  ( 57.05000000000001847, -0.7794871794871796045, 1.732743413496389939 ) ) ;
#2342 = CARTESIAN_POINT ( 'NONE',  ( 51.25000000000001421, 5.368152558471320595E-13, 3.111507638930570854E-58 ) ) ;
#2343 = ORIENTED_EDGE ( 'NONE', *, *, #19355, .F. ) ;
#2344 = CIRCLE ( 'NONE', #20057, 1.487500000000000933 ) ;
#2345 = SPHERICAL_SURFACE ( 'NONE', #167, 0.05000000000000000278 ) ;
#2346 = ORIENTED_EDGE ( 'NONE', *, *, #30119, .T. ) ;
#2347 = CARTESIAN_POINT ( 'NONE',  ( 15.41217651307626291, 0.2668145608218919218, -5.199999998579035498 ) ) ;
#2349 = CARTESIAN_POINT ( 'NONE',  ( 58.75000000000002132, 6.153735859711025284E-13, 3.111507638930570854E-58 ) ) ;
#2348 = CARTESIAN_POINT ( 'NONE',  ( 58.74999981404332772, 0.9032433253516619631, -1.734728236459875728 ) ) ;
#2350 = ORIENTED_EDGE ( 'NONE', *, *, #13832, .F. ) ;
#2351 = TOROIDAL_SURFACE ( 'NONE', #20062, 160.5997717543497743, 0.1000000000000000056 ) ;
#2352 = DIRECTION ( 'NONE',  ( 0.000000000000000000, 0.000000000000000000, 1.000000000000000000 ) ) ;
#2353 = FACE_OUTER_BOUND ( 'NONE', #837, .T. ) ;
#2354 = AXIS2_PLACEMENT_3D ( 'NONE', #28391, #16518, #7178 ) ;
#2356 = DIRECTION ( 'NONE',  ( 0.000000000000000000, 0.000000000000000000, -1.000000000000000000 ) ) ;
#2355 = CARTESIAN_POINT ( 'NONE',  ( 58.75000000000004263, -2.079005547593188119, 1.932245437381540134E-15 ) ) ;
#2357 = EDGE_LOOP ( 'NONE', ( #7788, #752, #639, #20784 ) ) ;
#2358 = CARTESIAN_POINT ( 'NONE',  ( -55.87499999999997158, 1.184343223768590692, 3.558065644182724974 ) ) ;
#2359 = CARTESIAN_POINT ( 'NONE',  ( 61.25000000000001421, 1.000000000000641709, 1.655766640118845112 ) ) ;
#2360 = CARTESIAN_POINT ( 'NONE',  ( 57.00000000000001421, 0.6999999999999999556, 2.452039967047845437 ) ) ;
#2361 = VECTOR ( 'NONE', #20954, 1000.000000000000000 ) ;
#2362 = LINE ( 'NONE', #12030, #8793 ) ;
#2363 = AXIS2_PLACEMENT_3D ( 'NONE', #7095, #24024, #28929 ) ;
#2364 = EDGE_CURVE ( 'NONE', #28412, #17938, #22756, .T. ) ;
#2365 = CIRCLE ( 'NONE', #17529, 1.875000000000001776 ) ;
#2366 = CARTESIAN_POINT ( 'NONE',  ( 58.64999999999999858, 1.655311165516931471, 1.077297519405395310 ) ) ;
#2367 = DIRECTION ( 'NONE',  ( 0.000000000000000000, -1.000000000000000000, 0.000000000000000000 ) ) ;
#2368 = VECTOR ( 'NONE', #12525, 1000.000000000000000 ) ;
#2369 = CYLINDRICAL_SURFACE ( 'NONE', #724, 4.849999999999999645 ) ;
#2370 = EDGE_LOOP ( 'NONE', ( #6560, #30304, #10944, #27026 ) ) ;
#2371 = DIRECTION ( 'NONE',  ( 0.000000000000000000, 0.000000000000000000, 1.000000000000000000 ) ) ;
#2372 = CARTESIAN_POINT ( 'NONE',  ( -57.72499999999997300, 0.9241234443029108236, -4.506217466977124886 ) ) ;
#2373 = LINE ( 'NONE', #12041, #31310 ) ;
#2374 = CIRCLE ( 'NONE', #4401, 1.899999999999999911 ) ;
#2375 = CARTESIAN_POINT ( 'NONE',  ( 51.88812122917229175, 8.998461838226505805, -1.950000000000180256 ) ) ;
#2376 = AXIS2_PLACEMENT_3D ( 'NONE', #4697, #2327, #21679 ) ;
#2377 = TOROIDAL_SURFACE ( 'NONE', #10980, 0.3000000000000000444, 0.05000000000000000278 ) ;
#2378 = CARTESIAN_POINT ( 'NONE',  ( -62.06395008846758543, -2.671759355462868246, 0.2104784954680237186 ) ) ;
#2379 = EDGE_CURVE ( 'NONE', #27051, #15300, #11016, .T. ) ;
#2380 = VECTOR ( 'NONE', #19019, 1000.000000000000000 ) ;
#2382 = DIRECTION ( 'NONE',  ( -1.000000000000000000, -2.586136946169074517E-16, 0.000000000000000000 ) ) ;
#2381 = DIRECTION ( 'NONE',  ( 0.000000000000000000, -1.000000000000000000, 0.000000000000000000 ) ) ;
#2383 = CARTESIAN_POINT ( 'NONE',  ( 61.24672990992804245, -0.9412912739128637130, 1.685898893893857053 ) ) ;
#2384 = VECTOR ( 'NONE', #15364, 1000.000000000000000 ) ;
#2386 = CARTESIAN_POINT ( 'NONE',  ( 24.34823467037697498, 5.521868380698618850, 1.424999999999915445 ) ) ;
#2385 = CARTESIAN_POINT ( 'NONE',  ( 58.45000000000001705, 0.8000000000000000444, -2.471260002560649927 ) ) ;
#2387 = VERTEX_POINT ( 'NONE', #4770 ) ;
#2388 = CYLINDRICAL_SURFACE ( 'NONE', #28487, 0.09999999999999982514 ) ;
#2389 = VECTOR ( 'NONE', #3649, 1000.000000000000000 ) ;
#2390 = CIRCLE ( 'NONE', #20103, 0.05000000000000012768 ) ;
#2392 = CARTESIAN_POINT ( 'NONE',  ( -36.04581030752630255, 4.861582136949842869, 2.394243986683832315 ) ) ;
#2391 = CARTESIAN_POINT ( 'NONE',  ( 51.45655683570191741, -0.9591657938390835136, -1.468576096419531574 ) ) ;
#2393 = CARTESIAN_POINT ( 'NONE',  ( 52.20711756518982583, 0.7500000000005468959, 1.718465885608440269 ) ) ;
#2394 = EDGE_LOOP ( 'NONE', ( #27307, #9449, #29332, #27452 ) ) ;
#2395 = ORIENTED_EDGE ( 'NONE', *, *, #12678, .F. ) ;
#2396 = CARTESIAN_POINT ( 'NONE',  ( 50.30000000000001847, 1.391941090707534023, -3.750000000000022649 ) ) ;
#2397 = ORIENTED_EDGE ( 'NONE', *, *, #22347, .T. ) ;
#2398 = DIRECTION ( 'NONE',  ( 1.000000000000000000, -0.000000000000000000, -0.000000000000000000 ) ) ;
#2399 = DIRECTION ( 'NONE',  ( 0.000000000000000000, -1.000000000000000000, 0.000000000000000000 ) ) ;
#2400 = TOROIDAL_SURFACE ( 'NONE', #11510, 1.375000000000001332, 0.2500000000000000000 ) ;
#2401 = ORIENTED_EDGE ( 'NONE', *, *, #21227, .T. ) ;
#2402 = CARTESIAN_POINT ( 'NONE',  ( -36.23324115033477710, -4.863061488092512263, -1.860589201779685231 ) ) ;
#2403 = ORIENTED_EDGE ( 'NONE', *, *, #2856, .F. ) ;
#2404 = VECTOR ( 'NONE', #21854, 1000.000000000000000 ) ;
#2405 = ADVANCED_FACE ( 'NONE', ( #23799, #187, #22044 ), #342, .T. ) ;
#2406 = DIRECTION ( 'NONE',  ( -2.095850865446309212E-30, -1.000000000000000000, -2.891205793294679411E-15 ) ) ;
#2407 = AXIS2_PLACEMENT_3D ( 'NONE', #17777, #15847, #13010 ) ;
#2408 = FILL_AREA_STYLE ('',( #29154 ) ) ;
#2409 = VERTEX_POINT ( 'NONE', #2240 ) ;
#2410 = CIRCLE ( 'NONE', #20121, 1.875000000000001776 ) ;
#2411 = CARTESIAN_POINT ( 'NONE',  ( -60.93749999999997868, 1.962990915244722689, 3.399999999999791633 ) ) ;
#2412 = VECTOR ( 'NONE', #11803, 1000.000000000000000 ) ;
#2413 = VECTOR ( 'NONE', #23951, 1000.000000000000000 ) ;
#2414 = CARTESIAN_POINT ( 'NONE',  ( 53.90445947017990136, 7.548890922513427526, -2.050000000000186784 ) ) ;
#2415 = DIRECTION ( 'NONE',  ( 3.489354422748178582E-15, -1.218509414717996338E-16, 1.000000000000000000 ) ) ;
#2416 = CARTESIAN_POINT ( 'NONE',  ( -56.90835481156723574, -0.7533615035077978472, 3.673546848079179750 ) ) ;
#2417 = DIRECTION ( 'NONE',  ( 1.000000000000000000, 1.047444401652940007E-14, 0.000000000000000000 ) ) ;
#2418 = EDGE_CURVE ( 'NONE', #14402, #20590, #21249, .T. ) ;
#2420 = CARTESIAN_POINT ( 'NONE',  ( -36.92443669619682112, 0.1565107631086873063, -5.407502298984291578 ) ) ;
#2419 = CARTESIAN_POINT ( 'NONE',  ( 58.65000000000000568, 1.077297519403822568, 1.655311165517741490 ) ) ;
#2421 = AXIS2_PLACEMENT_3D ( 'NONE', #17430, #7625, #12521 ) ;
#2422 = AXIS2_PLACEMENT_3D ( 'NONE', #22267, #17199, #5468 ) ;
#2423 = CARTESIAN_POINT ( 'NONE',  ( 47.06870114826936913, -4.259946762565045120, 1.000000153509832179 ) ) ;
#2424 = CARTESIAN_POINT ( 'NONE',  ( 51.50000000000001421, 1.163569835200988601E-28, -1.375000000000181188 ) ) ;
#2426 = CARTESIAN_POINT ( 'NONE',  ( 61.25000000000004263, -1.895722432251839562, -0.6373668173467583742 ) ) ;
#2425 = DIRECTION ( 'NONE',  ( 0.000000000000000000, 1.000000000000000000, 3.491481338843130594E-15 ) ) ;
#2427 = ORIENTED_EDGE ( 'NONE', *, *, #21785, .F. ) ;
#2429 = CARTESIAN_POINT ( 'NONE',  ( 67.95000000000003126, -1.025519176787267142E-28, -7.117384709231726808E-13 ) ) ;
#2428 = AXIS2_PLACEMENT_3D ( 'NONE', #27057, #28981, #2556 ) ;
#2430 = CARTESIAN_POINT ( 'NONE',  ( 15.03925126672132961, -0.4576450603546987628, 5.200000000000000178 ) ) ;
#2432 = CARTESIAN_POINT ( 'NONE',  ( 50.30000000000001847, -1.409901620910170017, 3.850000000000021849 ) ) ;
#2431 = CARTESIAN_POINT ( 'NONE',  ( 48.42155979508061137, -1.181909706220196643, 3.885998080850099790 ) ) ;
#2433 = EDGE_CURVE ( 'NONE', #25954, #30783, #4549, .T. ) ;
#2434 = CARTESIAN_POINT ( 'NONE',  ( 54.31978947732369534, 6.362875530773669297, -2.050000000000190781 ) ) ;
#2435 = ORIENTED_EDGE ( 'NONE', *, *, #10032, .F. ) ;
#2436 = DIRECTION ( 'NONE',  ( 0.000000000000000000, 0.000000000000000000, 1.000000000000000000 ) ) ;
#2437 = ORIENTED_EDGE ( 'NONE', *, *, #25376, .F. ) ;
#2438 = CARTESIAN_POINT ( 'NONE',  ( 22.72662675107779506, 7.272876594663846284, 1.424999999999921219 ) ) ;
#2439 = CARTESIAN_POINT ( 'NONE',  ( -57.13452994616205416, 3.117691453623979481, 1.799999999999809086 ) ) ;
#2440 = ORIENTED_EDGE ( 'NONE', *, *, #18349, .T. ) ;
#2441 = ORIENTED_EDGE ( 'NONE', *, *, #29407, .T. ) ;
#2442 = CARTESIAN_POINT ( 'NONE',  ( -59.48573950359912743, 3.423031164920794289, -1.114835254188495162 ) ) ;
#2443 = EDGE_LOOP ( 'NONE', ( #12858, #26263, #19765, #17088 ) ) ;
#2444 = CARTESIAN_POINT ( 'NONE',  ( 58.65000000000003411, -1.394635017527501297, 1.253243060178016455 ) ) ;
#2445 = EDGE_CURVE ( 'NONE', #20300, #355, #10467, .T. ) ;
#2446 = CARTESIAN_POINT ( 'NONE',  ( -56.07202994616204705, -4.156921938165296204, -2.141547992439359634E-13 ) ) ;
#2447 = ORIENTED_EDGE ( 'NONE', *, *, #29611, .F. ) ;
#2448 = CARTESIAN_POINT ( 'NONE',  ( -56.72499999999997300, -0.9241234443029054946, 4.506217466977124886 ) ) ;
#2449 = EDGE_CURVE ( 'NONE', #950, #3421, #973, .T. ) ;
#2450 = CARTESIAN_POINT ( 'NONE',  ( 51.59739104186229497, -1.010292945602101256, 1.272765950230260623 ) ) ;
#2451 = ADVANCED_FACE ( 'NONE', ( #3501 ), #22259, .T. ) ;
#2452 = CARTESIAN_POINT ( 'NONE',  ( 29.24156346100637549, 6.028130203020907629, 2.050000000000804512 ) ) ;
#2453 = ORIENTED_EDGE ( 'NONE', *, *, #23414, .T. ) ;
#2454 = AXIS2_PLACEMENT_3D ( 'NONE', #10410, #19925, #8195 ) ;
#2455 = CARTESIAN_POINT ( 'NONE',  ( 52.15659655364832048, -0.4999999999994547695, -1.807104036850121886 ) ) ;
#2456 = CARTESIAN_POINT ( 'NONE',  ( 52.06628335902946247, -0.5434431642975677823, 1.718465885608439603 ) ) ;
#2457 = DIRECTION ( 'NONE',  ( 0.000000000000000000, -1.000000000000000000, 0.000000000000000000 ) ) ;
#2458 = DIRECTION ( 'NONE',  ( 0.000000000000000000, 0.000000000000000000, 1.000000000000000000 ) ) ;
#2459 = DIRECTION ( 'NONE',  ( 0.000000000000000000, 0.02490330187380867394, -0.9996898646859344595 ) ) ;
#2460 = EDGE_CURVE ( 'NONE', #7502, #6162, #1508, .T. ) ;
#2462 = CARTESIAN_POINT ( 'NONE',  ( 58.73379417893118415, -0.8670685180651961366, 1.662624490945991740 ) ) ;
#2461 = CARTESIAN_POINT ( 'NONE',  ( 65.00000000000001421, -1.025519176787267142E-28, -6.808388610744108654E-13 ) ) ;
#2463 = B_SPLINE_CURVE_WITH_KNOTS ( 'NONE', 3,
 ( #10047, #7803, #29654, #14781 ),
 .UNSPECIFIED., .F., .F.,
 ( 4, 4 ),
 ( 0.000000000000000000, 7.924777108412403711E-05 ),
 .UNSPECIFIED. ) ;
#2464 = CARTESIAN_POINT ( 'NONE',  ( 51.76226673693759039, -4.256154442720826658, 1.015631899367400948 ) ) ;
#2465 = CARTESIAN_POINT ( 'NONE',  ( -56.18749999999997868, 0.7533615035078125022, -3.673546848079176641 ) ) ;
#2466 = DIRECTION ( 'NONE',  ( 0.000000000000000000, 0.000000000000000000, 1.000000000000000000 ) ) ;
#2467 = VERTEX_POINT ( 'NONE', #10624 ) ;
#2468 = EDGE_CURVE ( 'NONE', #11413, #17625, #14760, .T. ) ;
#2469 = CIRCLE ( 'NONE', #20182, 0.09999999999999942268 ) ;
#2470 = CIRCLE ( 'NONE', #20185, 0.1000000000000001721 ) ;
#2471 = ORIENTED_EDGE ( 'NONE', *, *, #9703, .T. ) ;
#2472 = AXIS2_PLACEMENT_3D ( 'NONE', #17817, #5768, #15421 ) ;
#2473 = CARTESIAN_POINT ( 'NONE',  ( -58.43749999999997158, 0.7533615035078148336, -3.673546848079175309 ) ) ;
#2474 = EDGE_LOOP ( 'NONE', ( #6328, #2570, #20144, #14080, #18366, #17961 ) ) ;
#2475 =( BOUNDED_SURFACE ( )  B_SPLINE_SURFACE ( 3, 2, ( 
 ( #15199, #19807, #14145 ),
 ( #29440, #26341, #11626 ),
 ( #29592, #7752, #10289 ),
 ( #24536, #4644, #17418 ) ),
 .UNSPECIFIED., .F., .F., .F. ) 
 B_SPLINE_SURFACE_WITH_KNOTS ( ( 4, 4 ),
 ( 3, 3 ),
 ( 4.041453792691653391, 4.300872134317200945 ),
 ( 0.000000000000000000, 1.000000000000000000 ),
 .UNSPECIFIED. ) 
 GEOMETRIC_REPRESENTATION_ITEM ( )  RATIONAL_B_SPLINE_SURFACE ( (
 ( 1.000000000000000000, 0.8699658093904929501, 1.000000000000000000),
 ( 1.000000000000000000, 0.8538860448759273414, 1.000000000000000000),
 ( 1.000000000000000000, 0.8356979842195431107, 1.000000000000000000),
 ( 1.000000000000000000, 0.8156258140602941076, 1.000000000000000000) ) ) 
 REPRESENTATION_ITEM ( '' )  SURFACE ( )  );
#2476 = CARTESIAN_POINT ( 'NONE',  ( 61.25000000000003553, -1.106298139389941149, 1.666164585742037296 ) ) ;
#2477 = CARTESIAN_POINT ( 'NONE',  ( -60.53335481156722864, -4.108500314926510022, 1.367561758111408343 ) ) ;
#2479 = CARTESIAN_POINT ( 'NONE',  ( 50.40000000000001990, -4.899999999999999467, 4.100000000000022737 ) ) ;
#2478 = DIRECTION ( 'NONE',  ( 1.000000000000000000, 1.047444401652940007E-14, -0.000000000000000000 ) ) ;
#2480 = EDGE_LOOP ( 'NONE', ( #29463, #7474, #4333, #26667, #1530 ) ) ;
#2481 = ORIENTED_EDGE ( 'NONE', *, *, #22900, .F. ) ;
#2482 = DIRECTION ( 'NONE',  ( -1.047444401652940007E-14, 0.000000000000000000, -1.000000000000000000 ) ) ;
#2483 = ORIENTED_EDGE ( 'NONE', *, *, #13665, .F. ) ;
#2484 = FACE_OUTER_BOUND ( 'NONE', #7910, .T. ) ;
#2485 = EDGE_LOOP ( 'NONE', ( #8470, #10363, #14101, #4533 ) ) ;
#2486 = CARTESIAN_POINT ( 'NONE',  ( -36.92398358572908990, 5.053896291911939009, 1.944420249220693675 ) ) ;
#2487 = ADVANCED_FACE ( 'NONE', ( #17602 ), #14936, .T. ) ;
#2488 = VERTEX_POINT ( 'NONE', #3026 ) ;
#2489 = CARTESIAN_POINT ( 'NONE',  ( 56.95000076968187130, -0.7321971888534951622, 1.754073505128400878 ) ) ;
#2490 = EDGE_CURVE ( 'NONE', #9458, #22270, #17710, .T. ) ;
#2491 = CARTESIAN_POINT ( 'NONE',  ( 57.03449256411899881, 0.7475344026195360758, 1.780552047803072302 ) ) ;
#2492 = CARTESIAN_POINT ( 'NONE',  ( -35.85663232820583346, -4.817150320980683631, 2.203324261490539282 ) ) ;
#2493 = CARTESIAN_POINT ( 'NONE',  ( -56.14405989232413674, -3.920666489018339623E-15, 3.399999999999799627 ) ) ;
#2494 = CARTESIAN_POINT ( 'NONE',  ( 52.72267294271966165, 4.003822062839299534, -2.050000000000183675 ) ) ;
#2495 = MECHANICAL_DESIGN_GEOMETRIC_PRESENTATION_REPRESENTATION (  '', ( #4497 ), #24233 ) ;
#2496 = AXIS2_PLACEMENT_3D ( 'NONE', #29793, #8107, #17776 ) ;
#2497 = DIRECTION ( 'NONE',  ( 0.000000000000000000, 0.000000000000000000, 1.000000000000000000 ) ) ;
#2498 = CARTESIAN_POINT ( 'NONE',  ( 50.32795105345940101, 1.409900792624783294, -3.850000304694921827 ) ) ;
#2499 = CARTESIAN_POINT ( 'NONE',  ( 15.59055531549694429, -5.360541651686761000, -0.7128348320084266776 ) ) ;
#2500 = CARTESIAN_POINT ( 'NONE',  ( -36.72207054450174724, 0.6818242347930701941, 5.365311767243446717 ) ) ;
#2501 = VECTOR ( 'NONE', #3103, 1000.000000000000000 ) ;
#2502 = ORIENTED_EDGE ( 'NONE', *, *, #8643, .T. ) ;
#2503 = ADVANCED_FACE ( 'NONE', ( #20149 ), #19971, .F. ) ;
#2504 = CARTESIAN_POINT ( 'NONE',  ( -44.59999999999997300, -3.624999999999988010, -1.997442628057709707E-13 ) ) ;
#2506 = CARTESIAN_POINT ( 'NONE',  ( -63.84999999999997300, 2.699162634652023662, 0.06723891505929292800 ) ) ;
#2505 = CARTESIAN_POINT ( 'NONE',  ( -36.23324115033477710, -2.840672495176407075, -4.363684107482597163 ) ) ;
#2507 = CYLINDRICAL_SURFACE ( 'NONE', #7444, 0.1000000000000000472 ) ;
#2508 = EDGE_CURVE ( 'NONE', #21159, #28946, #14385, .T. ) ;
#2509 = ORIENTED_EDGE ( 'NONE', *, *, #23253, .T. ) ;
#2510 = DIRECTION ( 'NONE',  ( 0.000000000000000000, 0.9996898646859347926, 0.02490330187379526453 ) ) ;
#2511 =( BOUNDED_CURVE ( )  B_SPLINE_CURVE ( 3, ( #2017, #28308, #24021, #8986 ),
 .UNSPECIFIED., .F., .T. ) 
 B_SPLINE_CURVE_WITH_KNOTS ( ( 4, 4 ),
 ( 4.399031134232678220, 4.429249381401446861 ),
 .UNSPECIFIED. ) 
 CURVE ( )  GEOMETRIC_REPRESENTATION_ITEM ( )  RATIONAL_B_SPLINE_CURVE ( ( 1.000000000000000000, 0.9999239062424463143, 0.9999239062424463143, 1.000000000000000000 ) ) 
 REPRESENTATION_ITEM ( '' )  );
#2512 = AXIS2_PLACEMENT_3D ( 'NONE', #8226, #3489, #30379 ) ;
#2513 = ORIENTED_EDGE ( 'NONE', *, *, #29211, .F. ) ;
#2514 = EDGE_CURVE ( 'NONE', #1336, #2034, #12622, .T. ) ;
#2515 = CARTESIAN_POINT ( 'NONE',  ( 15.03925126672122836, 1.123735532908292312, -5.289358697221543615 ) ) ;
#2516 = CARTESIAN_POINT ( 'NONE',  ( -36.11122220296839203, -4.822476035523795446, 1.985498375066742982 ) ) ;
#2518 = FACE_OUTER_BOUND ( 'NONE', #27815, .T. ) ;
#2517 = DIRECTION ( 'NONE',  ( -1.000000000000000000, -3.054025858079668409E-16, 2.042474015755241579E-16 ) ) ;
#2519 = ORIENTED_EDGE ( 'NONE', *, *, #8623, .T. ) ;
#2520 = CARTESIAN_POINT ( 'NONE',  ( 50.87477060347373481, 8.633605004118187765, -2.050000000000176570 ) ) ;
#2521 = STYLED_ITEM ( 'NONE', ( #12068 ), #28934 ) ;
#2522 = CIRCLE ( 'NONE', #13630, 3.750000000000000444 ) ;
#2523 = DIRECTION ( 'NONE',  ( 0.000000000000000000, -1.000000000000000000, 0.000000000000000000 ) ) ;
#2525 = CARTESIAN_POINT ( 'NONE',  ( -54.49999516060625382, -1.549196738101655368, -4.063926895246979143 ) ) ;
#2524 = DIRECTION ( 'NONE',  ( 0.000000000000000000, 1.000000000000000000, 0.000000000000000000 ) ) ;
#2526 = VERTEX_POINT ( 'NONE', #13752 ) ;
#2527 = CARTESIAN_POINT ( 'NONE',  ( -57.62499999999997158, 2.489203624310591056, -2.804704140674917578 ) ) ;
#2528 = CARTESIAN_POINT ( 'NONE',  ( 61.24012582333622845, 0.9011229182324727027, 1.742583661752045820 ) ) ;
#2529 = LINE ( 'NONE', #2045, #8954 ) ;
#2530 = CARTESIAN_POINT ( 'NONE',  ( -55.18749999999996447, 1.962990915244749557, -3.400000000000187761 ) ) ;
#2531 = AXIS2_PLACEMENT_3D ( 'NONE', #20331, #12549, #15089 ) ;
#2532 = B_SPLINE_CURVE_WITH_KNOTS ( 'NONE', 3,
 ( #14574, #19486, #19194, #16656, #24238, #17121 ),
 .UNSPECIFIED., .F., .F.,
 ( 4, 2, 4 ),
 ( 0.000000000000000000, 0.0001000270069610660921, 0.0002000540139221321841 ),
 .UNSPECIFIED. ) ;
#2533 = DIRECTION ( 'NONE',  ( -7.145967004358956819E-15, 0.5454670984331110306, -0.8381322357044637128 ) ) ;
#2534 = CARTESIAN_POINT ( 'NONE',  ( -35.85663232820584057, 1.793057972834477765, -4.026191436120592826 ) ) ;
#2535 = FACE_OUTER_BOUND ( 'NONE', #11935, .T. ) ;
#2536 = ORIENTED_EDGE ( 'NONE', *, *, #12223, .F. ) ;
#2537 = DIRECTION ( 'NONE',  ( 0.000000000000000000, 0.000000000000000000, 1.000000000000000000 ) ) ;
#2538 = CARTESIAN_POINT ( 'NONE',  ( 15.45522337368514521, -3.212533369474619427, 4.093511368021648167 ) ) ;
#2539 = DIRECTION ( 'NONE',  ( 0.03489949670185131525, 0.9993908270191184107, 0.000000000000000000 ) ) ;
#2540 = CARTESIAN_POINT ( 'NONE',  ( -62.05037051514401014, -2.687515796301105819, 0.2593462970732348660 ) ) ;
#2541 = AXIS2_PLACEMENT_3D ( 'NONE', #26876, #7865, #281 ) ;
#2543 = CARTESIAN_POINT ( 'NONE',  ( 53.37676683120072596, 7.899656915230087506, -1.885229198846103404 ) ) ;
#2542 = CARTESIAN_POINT ( 'NONE',  ( -59.51761855918065436, 2.467398989037824286, -1.133240635510041727 ) ) ;
#2544 = EDGE_CURVE ( 'NONE', #19199, #2126, #16698, .T. ) ;
#2546 = AXIS2_PLACEMENT_3D ( 'NONE', #9299, #21498, #9465 ) ;
#2545 = DIRECTION ( 'NONE',  ( 0.000000000000000000, -0.2008964009354147762, 0.9796124928211140670 ) ) ;
#2548 = CARTESIAN_POINT ( 'NONE',  ( 26.18134456910377494, 5.211034382732834480, 1.424999999999908562 ) ) ;
#2547 = CARTESIAN_POINT ( 'NONE',  ( 51.70000000000003126, -3.550773357292059007, 2.049880134335640758 ) ) ;
#2549 = EDGE_CURVE ( 'NONE', #28731, #28363, #7089, .T. ) ;
#2550 = ORIENTED_EDGE ( 'NONE', *, *, #14624, .T. ) ;
#2551 = CARTESIAN_POINT ( 'NONE',  ( 58.65000000000004121, -1.782657835994441387, 0.5811678240968194409 ) ) ;
#2552 = ADVANCED_FACE ( 'NONE', ( #3795 ), #15832, .T. ) ;
#2553 = CARTESIAN_POINT ( 'NONE',  ( 54.40000000000001990, 1.029992063861229212E-15, -4.375000000000002665 ) ) ;
#2555 = CARTESIAN_POINT ( 'NONE',  ( -35.85663232820584057, -3.275050215668598774, -2.949461045527609127 ) ) ;
#2554 = CARTESIAN_POINT ( 'NONE',  ( 15.03925126672127810, -2.686240680702128625, -4.475885388010734545 ) ) ;
#2556 = DIRECTION ( 'NONE',  ( 0.000000000000000000, 0.000000000000000000, -1.000000000000000000 ) ) ;
#2557 = ORIENTED_EDGE ( 'NONE', *, *, #18563, .T. ) ;
#2558 = ORIENTED_EDGE ( 'NONE', *, *, #15305, .T. ) ;
#2559 = ORIENTED_EDGE ( 'NONE', *, *, #30590, .F. ) ;
#2560 = DIRECTION ( 'NONE',  ( 1.000000000000000000, 3.054025858079668409E-16, -2.042474015755241579E-16 ) ) ;
#2561 = CARTESIAN_POINT ( 'NONE',  ( -56.43749999999997158, -4.108500314926507357, 1.367561758111402792 ) ) ;
#2562 = ORIENTED_EDGE ( 'NONE', *, *, #22320, .F. ) ;
#2563 = DIRECTION ( 'NONE',  ( -1.000000000000000000, -0.000000000000000000, 3.491481338843133355E-15 ) ) ;
#2564 = ORIENTED_EDGE ( 'NONE', *, *, #10095, .F. ) ;
#2565 = SURFACE_STYLE_FILL_AREA ( #28995 ) ;
#2566 = ADVANCED_FACE ( 'NONE', ( #11393 ), #11623, .T. ) ;
#2567 = B_SPLINE_CURVE_WITH_KNOTS ( 'NONE', 3,
 ( #27347, #29723, #29402, #5656, #8035, #12925, #19919, #14833, #21987, #280 ),
 .UNSPECIFIED., .F., .F.,
 ( 4, 2, 2, 2, 4 ),
 ( 0.000000000000000000, 0.0004363777631660865864, 0.0006545666447491310181, 0.0007636610855406569202, 0.0008727555263321828223 ),
 .UNSPECIFIED. ) ;
#2568 = DIRECTION ( 'NONE',  ( -1.000000000000000000, 0.000000000000000000, 1.047444401652940007E-14 ) ) ;
#2569 = VERTEX_POINT ( 'NONE', #18379 ) ;
#2570 = ORIENTED_EDGE ( 'NONE', *, *, #9386, .T. ) ;
#2571 = ORIENTED_EDGE ( 'NONE', *, *, #23479, .F. ) ;
#2572 = AXIS2_PLACEMENT_3D ( 'NONE', #7590, #12181, #16636 ) ;
#2573 = CARTESIAN_POINT ( 'NONE',  ( -57.50952994616203995, -3.117691453623963938, -1.800000000000215206 ) ) ;
#2574 = CARTESIAN_POINT ( 'NONE',  ( 58.75000000000003553, -1.800471618824714071, 1.039502773796719959 ) ) ;
#2575 = DIRECTION ( 'NONE',  ( 0.000000000000000000, -1.000000000000000000, -3.491481338843139666E-15 ) ) ;
#2576 = DIRECTION ( 'NONE',  ( 0.000000000000000000, -1.000000000000000000, 0.000000000000000000 ) ) ;
#2577 = CARTESIAN_POINT ( 'NONE',  ( 31.35411506832756601, 7.935106539446550755, -1.425000000000109068 ) ) ;
#2579 = CARTESIAN_POINT ( 'NONE',  ( -36.56390771145571961, 0.2088129849843024799, -5.405094643512487806 ) ) ;
#2578 = CARTESIAN_POINT ( 'NONE',  ( 50.55258015808398397, 5.293720379222080095E-13, -1.177580158083963546 ) ) ;
#2580 = CARTESIAN_POINT ( 'NONE',  ( 51.70000000000002416, 2.428612866367529932E-14, -1.805095852181900386E-13 ) ) ;
#2581 = CARTESIAN_POINT ( 'NONE',  ( 16.10660252424457184, -2.945786441214570672, 4.543674732827748031 ) ) ;
#2583 = CARTESIAN_POINT ( 'NONE',  ( 61.25000000000001421, 1.106298139389969348, 1.666164585743605375 ) ) ;
#2582 = CARTESIAN_POINT ( 'NONE',  ( 54.49860577577695864, -0.002682860454195030130, -4.292318283074052054 ) ) ;
#2584 = EDGE_CURVE ( 'NONE', #23640, #22807, #11115, .T. ) ;
#2585 = ORIENTED_EDGE ( 'NONE', *, *, #9944, .T. ) ;
#2586 = CARTESIAN_POINT ( 'NONE',  ( 58.65000000000003411, -1.394635017527761311, -1.253243060177727131 ) ) ;
#2587 = CARTESIAN_POINT ( 'NONE',  ( -36.14504829323105639, -5.374753047227058822, -0.5963205376973962357 ) ) ;
#2588 = VECTOR ( 'NONE', #13273, 1000.000000000000000 ) ;
#2590 = CARTESIAN_POINT ( 'NONE',  ( 52.50881341635840727, 3.945078575635807550, 1.125510014975697803 ) ) ;
#2589 = DIRECTION ( 'NONE',  ( 1.000000000000000000, -1.165806029810706544E-15, -1.108125256279691767E-14 ) ) ;
#2591 = DIRECTION ( 'NONE',  ( 1.047444401652940007E-14, 0.000000000000000000, 1.000000000000000000 ) ) ;
#2592 = VERTEX_POINT ( 'NONE', #6332 ) ;
#2593 = CARTESIAN_POINT ( 'NONE',  ( 51.41639946534622396, 0.9865458190826668083, 1.594793944595433111 ) ) ;
#2594 = VERTEX_POINT ( 'NONE', #8849 ) ;
#2595 = CARTESIAN_POINT ( 'NONE',  ( 26.19155409318043937, 5.638511060912940742, 1.424999999999908784 ) ) ;
#2596 = ORIENTED_EDGE ( 'NONE', *, *, #14438, .T. ) ;
#2597 = ORIENTED_EDGE ( 'NONE', *, *, #12546, .T. ) ;
#2598 = DIRECTION ( 'NONE',  ( -1.000000000000000000, -0.000000000000000000, 3.491481338843133355E-15 ) ) ;
#2599 = EDGE_LOOP ( 'NONE', ( #17167, #21447 ) ) ;
#2600 = DIRECTION ( 'NONE',  ( 1.000000000000000000, 3.053848253006669023E-16, -2.042510438544995415E-16 ) ) ;
#2601 = EDGE_CURVE ( 'NONE', #10532, #10212, #24224, .T. ) ;
#2602 = CARTESIAN_POINT ( 'NONE',  ( -57.13452994616205416, 3.117691453623979481, 1.799999999999809086 ) ) ;
#2603 = VERTEX_POINT ( 'NONE', #20614 ) ;
#2604 = CARTESIAN_POINT ( 'NONE',  ( 61.21683709729278888, -0.7974544867251196489, -1.837034727152028424 ) ) ;
#2605 = CARTESIAN_POINT ( 'NONE',  ( 50.25000000000004263, -1.800471618824301734, -1.039502773796582069 ) ) ;
#2606 = CARTESIAN_POINT ( 'NONE',  ( 30.73039769179423786, 7.037486595896031538, 2.050000000000022915 ) ) ;
#2607 = ORIENTED_EDGE ( 'NONE', *, *, #4355, .F. ) ;
#2608 = CIRCLE ( 'NONE', #6060, 0.1499999999999999667 ) ;
#2609 = CARTESIAN_POINT ( 'NONE',  ( -54.81249999999998579, -1.962990915244731793, 3.399999999999796962 ) ) ;
#2610 = CARTESIAN_POINT ( 'NONE',  ( -54.48118151432741030, -1.510613940323803694, 4.037256667234631280 ) ) ;
#2611 = CARTESIAN_POINT ( 'NONE',  ( -60.59999999999997300, -2.476825173781434852, 0.9422510591782664591 ) ) ;
#2612 = FACE_OUTER_BOUND ( 'NONE', #1760, .T. ) ;
#2613 = FACE_OUTER_BOUND ( 'NONE', #3696, .T. ) ;
#2615 = FACE_OUTER_BOUND ( 'NONE', #17055, .T. ) ;
#2614 = FACE_BOUND ( 'NONE', #11778, .T. ) ;
#2616 = CARTESIAN_POINT ( 'NONE',  ( 51.36283714269074352, 1.001673184508090397, 1.284520656909115877 ) ) ;
#2617 = DIRECTION ( 'NONE',  ( 0.000000000000000000, 0.000000000000000000, -1.000000000000000000 ) ) ;
#2618 = EDGE_CURVE ( 'NONE', #24348, #28516, #29867, .T. ) ;
#2619 = AXIS2_PLACEMENT_3D ( 'NONE', #12861, #1012, #24757 ) ;
#2620 = CARTESIAN_POINT ( 'NONE',  ( 53.78456803694547972, 5.661108390837235937, 2.049999999999812417 ) ) ;
#2621 = ORIENTED_EDGE ( 'NONE', *, *, #6295, .T. ) ;
#2622 = ORIENTED_EDGE ( 'NONE', *, *, #20452, .F. ) ;
#2623 = CIRCLE ( 'NONE', #4124, 0.4576450603546982632 ) ;
#2624 = VERTEX_POINT ( 'NONE', #1259 ) ;
#2625 = CARTESIAN_POINT ( 'NONE',  ( 44.98443556292537693, -3.826179070414207573, 1.100000000000000311 ) ) ;
#2626 = CARTESIAN_POINT ( 'NONE',  ( -54.48542740578361077, 0.7887156198831670739, -3.845940847736174728 ) ) ;
#2628 = CARTESIAN_POINT ( 'NONE',  ( -35.85663232820601820, 2.199885893005899096, 4.939696249117697668 ) ) ;
#2627 = DIRECTION ( 'NONE',  ( 0.03489949670185131525, 0.9993908270191184107, 0.000000000000000000 ) ) ;
#2629 = ORIENTED_EDGE ( 'NONE', *, *, #16126, .T. ) ;
#2630 = ORIENTED_EDGE ( 'NONE', *, *, #20852, .F. ) ;
#2631 = CARTESIAN_POINT ( 'NONE',  ( 22.07280086217093640, 8.086143481909148889, -2.050000000000076650 ) ) ;
#2632 = ORIENTED_EDGE ( 'NONE', *, *, #11598, .F. ) ;
#2633 = DIRECTION ( 'NONE',  ( 9.654113257610060303E-15, 0.000000000000000000, 1.000000000000000000 ) ) ;
#2634 = EDGE_CURVE ( 'NONE', #24678, #14148, #6039, .T. ) ;
#2635 = ORIENTED_EDGE ( 'NONE', *, *, #15008, .F. ) ;
#2636 = FACE_OUTER_BOUND ( 'NONE', #23492, .T. ) ;
#2637 = ORIENTED_EDGE ( 'NONE', *, *, #6688, .T. ) ;
#2638 = CARTESIAN_POINT ( 'NONE',  ( 51.13996726386385916, -0.9386186536664237190, 1.439073407537155180 ) ) ;
#2639 = DIRECTION ( 'NONE',  ( 1.000000000000000000, 1.047444401652940007E-14, 0.000000000000000000 ) ) ;
#2640 = SPHERICAL_SURFACE ( 'NONE', #24366, 0.1000000000000000056 ) ;
#2642 = AXIS2_PLACEMENT_3D ( 'NONE', #10077, #5160, #14512 ) ;
#2641 = CARTESIAN_POINT ( 'NONE',  ( -55.45655989232413674, 1.962990915244722245, 3.399999999999810285 ) ) ;
#2643 = EDGE_CURVE ( 'NONE', #19132, #30566, #10273, .T. ) ;
#2644 = CARTESIAN_POINT ( 'NONE',  ( 53.60009913848111296, 4.619321414059949227, -2.050000000000186784 ) ) ;
#2645 = CARTESIAN_POINT ( 'NONE',  ( 22.07280086217093640, 8.086143481909152442, -1.950000000000076339 ) ) ;
#2647 = ORIENTED_EDGE ( 'NONE', *, *, #775, .T. ) ;
#2646 = CARTESIAN_POINT ( 'NONE',  ( 15.03925126672132961, -3.275050215668596998, 2.949461045527590475 ) ) ;
#2648 = CARTESIAN_POINT ( 'NONE',  ( -59.09999999999997300, -2.465712773623968790, -0.9709585562669303949 ) ) ;
#2649 = ADVANCED_FACE ( 'NONE', ( #10922 ), #8550, .F. ) ;
#2650 = LINE ( 'NONE', #22137, #12906 ) ;
#2651 = EDGE_CURVE ( 'NONE', #11471, #3677, #1003, .T. ) ;
#2652 =( BOUNDED_SURFACE ( )  B_SPLINE_SURFACE ( 3, 2, ( 
 ( #8152, #20210, #20514 ),
 ( #17823, #8465, #27782 ),
 ( #29840, #3566, #20039 ),
 ( #13341, #6097, #15119 ) ),
 .UNSPECIFIED., .F., .F., .F. ) 
 B_SPLINE_SURFACE_WITH_KNOTS ( ( 4, 4 ),
 ( 3, 3 ),
 ( 0.8603049414497402347, 1.079657356097645904 ),
 ( 0.000000000000000000, 1.000000000000000000 ),
 .UNSPECIFIED. ) 
 GEOMETRIC_REPRESENTATION_ITEM ( )  RATIONAL_B_SPLINE_SURFACE ( (
 ( 1.000000000000000000, 0.8142797953134848221, 1.000000000000000000),
 ( 1.000000000000000000, 0.8057719789464390381, 1.000000000000000000),
 ( 1.000000000000000000, 0.7963243424565560336, 1.000000000000000000),
 ( 1.000000000000000000, 0.7860710104634932582, 1.000000000000000000) ) ) 
 REPRESENTATION_ITEM ( '' )  SURFACE ( )  );
#2653 = VECTOR ( 'NONE', #22802, 1000.000000000000000 ) ;
#2654 = ORIENTED_EDGE ( 'NONE', *, *, #3672, .F. ) ;
#2655 = EDGE_CURVE ( 'NONE', #18673, #13278, #9522, .T. ) ;
#2656 = DIRECTION ( 'NONE',  ( 1.000000000000000000, 1.047444401652940007E-14, 0.000000000000000000 ) ) ;
#2657 = CARTESIAN_POINT ( 'NONE',  ( 51.55144386500332132, -1.037443573994098811, -1.251214392908860829 ) ) ;
#2658 = DIRECTION ( 'NONE',  ( 0.000000000000000000, 1.000000000000000000, -0.000000000000000000 ) ) ;
#2659 = VERTEX_POINT ( 'NONE', #26120 ) ;
#2660 = DIRECTION ( 'NONE',  ( 0.000000000000000000, 1.000000000000000000, 0.000000000000000000 ) ) ;
#2661 = APPLICATION_CONTEXT ( 'automotive_design' ) ;
#2662 = VERTEX_POINT ( 'NONE', #26284 ) ;
#2663 = CARTESIAN_POINT ( 'NONE',  ( 15.45522337368515409, 0.1928884786868352297, -5.200000000471178829 ) ) ;
#2664 = CARTESIAN_POINT ( 'NONE',  ( -36.21152527658240672, -4.855742670514293202, 1.883114206442314309 ) ) ;
#2666 = CARTESIAN_POINT ( 'NONE',  ( 51.70000000000003126, -3.637377585518695611, 2.099877210782855830 ) ) ;
#2665 = CARTESIAN_POINT ( 'NONE',  ( 51.70000000000003126, -4.079448311123456961, 2.129011300494053849 ) ) ;
#2667 = VERTEX_POINT ( 'NONE', #4436 ) ;
#2668 = CARTESIAN_POINT ( 'NONE',  ( -35.85663232820584057, 3.426725943139577790, -3.937891353488711221 ) ) ;
#2669 = DIRECTION ( 'NONE',  ( 0.000000000000000000, 1.000000000000000000, 0.000000000000000000 ) ) ;
#2671 = CARTESIAN_POINT ( 'NONE',  ( 64.00000000000001421, 1.163569835200988601E-28, -2.234548056859606357E-13 ) ) ;
#2670 = FACE_OUTER_BOUND ( 'NONE', #24696, .T. ) ;
#2672 = ORIENTED_EDGE ( 'NONE', *, *, #29379, .F. ) ;
#2673 = CARTESIAN_POINT ( 'NONE',  ( -59.99999999999997158, -1.184343223768586251, -3.558065644182723197 ) ) ;
#2674 = CARTESIAN_POINT ( 'NONE',  ( 51.80000000000001137, 3.850000000000016520, -1.678541033159632434 ) ) ;
#2675 = CARTESIAN_POINT ( 'NONE',  ( -44.49999999999999289, -1.514093959731547701, 3.183260039818174292 ) ) ;
#2676 = CARTESIAN_POINT ( 'NONE',  ( -55.12499999999997158, 2.944486372867106905, -1.700000000000183364 ) ) ;
#2677 = CARTESIAN_POINT ( 'NONE',  ( -54.50000000000001421, -2.140856255279098619, -2.841089121193913325 ) ) ;
#2678 = DIRECTION ( 'NONE',  ( 0.000000000000000000, 1.000000000000000000, 0.000000000000000000 ) ) ;
#2680 = FACE_OUTER_BOUND ( 'NONE', #20214, .T. ) ;
#2679 = AXIS2_PLACEMENT_3D ( 'NONE', #9089, #10829, #20512 ) ;
#2681 = EDGE_CURVE ( 'NONE', #16826, #29056, #7594, .T. ) ;
#2682 = ORIENTED_EDGE ( 'NONE', *, *, #31061, .T. ) ;
#2683 = ADVANCED_FACE ( 'NONE', ( #19013 ), #14972, .F. ) ;
#2684 = CARTESIAN_POINT ( 'NONE',  ( 15.94709373951305409, -3.646691605040370820, 3.993181011920696299 ) ) ;
#2685 = CARTESIAN_POINT ( 'NONE',  ( 30.88580673845696722, 7.128392828669079861, -1.950000000000106315 ) ) ;
#2686 = DIRECTION ( 'NONE',  ( -0.000000000000000000, -0.000000000000000000, -1.000000000000000000 ) ) ;
#2687 = CYLINDRICAL_SURFACE ( 'NONE', #21556, 4.099999999999992539 ) ;
#2688 = EDGE_CURVE ( 'NONE', #31086, #4137, #11081, .T. ) ;
#2689 = DIRECTION ( 'NONE',  ( 0.000000000000000000, 0.000000000000000000, -1.000000000000000000 ) ) ;
#2691 = CARTESIAN_POINT ( 'NONE',  ( -45.15971931043468146, -14.70000000000001883, 1.800230794746610701E-15 ) ) ;
#2690 = CARTESIAN_POINT ( 'NONE',  ( 51.80000000000002558, 4.350000000000017408, 1.550321101314541927 ) ) ;
#2692 = VERTEX_POINT ( 'NONE', #28821 ) ;
#2693 = CARTESIAN_POINT ( 'NONE',  ( 58.73379417893125520, -1.788763080991752963, 0.5625430232375976392 ) ) ;
#2694 = ORIENTED_EDGE ( 'NONE', *, *, #17758, .F. ) ;
#2695 = DIRECTION ( 'NONE',  ( 0.000000000000000000, 1.000000000000000000, 3.491481338843133355E-15 ) ) ;
#2696 = CIRCLE ( 'NONE', #21934, 0.05000000000000012768 ) ;
#2698 = DIRECTION ( 'NONE',  ( 1.000000000000000000, -0.000000000000000000, -1.047444401652940007E-14 ) ) ;
#2697 = DIRECTION ( 'NONE',  ( -1.000000000000000000, -1.047444401652940007E-14, -0.000000000000000000 ) ) ;
#2699 = CIRCLE ( 'NONE', #20918, 3.950000000000000178 ) ;
#2700 = ORIENTED_EDGE ( 'NONE', *, *, #3749, .F. ) ;
#2701 = ORIENTED_EDGE ( 'NONE', *, *, #3718, .T. ) ;
#2702 = LINE ( 'NONE', #12342, #230 ) ;
#2703 = EDGE_LOOP ( 'NONE', ( #25204, #3417, #7605 ) ) ;
#2704 = CARTESIAN_POINT ( 'NONE',  ( -59.19999999999997442, 2.449420067797480893, 1.250136525132548693 ) ) ;
#2705 = CARTESIAN_POINT ( 'NONE',  ( 50.38154193469295450, 1.153441674035750708, 3.890342980189691158 ) ) ;
#2706 = CARTESIAN_POINT ( 'NONE',  ( -36.56242893520637693, -5.206628483174487343, -1.466363261642641191 ) ) ;
#2707 = ORIENTED_EDGE ( 'NONE', *, *, #15872, .F. ) ;
#2708 = CARTESIAN_POINT ( 'NONE',  ( 69.25000000000000000, -0.7500000000000000000, -1.988246715074083681 ) ) ;
#2709 = EDGE_CURVE ( 'NONE', #9170, #21964, #16667, .T. ) ;
#2710 = ORIENTED_EDGE ( 'NONE', *, *, #10733, .T. ) ;
#2711 = EDGE_CURVE ( 'NONE', #12883, #7683, #19205, .T. ) ;
#2712 = CARTESIAN_POINT ( 'NONE',  ( -60.13452994616204705, 3.117691453623979481, 1.799999999999798428 ) ) ;
#2713 = EDGE_CURVE ( 'NONE', #12851, #3601, #26251, .T. ) ;
#2714 = CARTESIAN_POINT ( 'NONE',  ( 53.66827364943466705, 4.678978782231800082, -2.050000000000186784 ) ) ;
#2715 = CARTESIAN_POINT ( 'NONE',  ( 58.45000000000001705, 0.8000000000000000444, 2.421260002560649660 ) ) ;
#2716 = CIRCLE ( 'NONE', #6762, 2.374999999999998668 ) ;
#2717 = DIRECTION ( 'NONE',  ( -1.000000000000000000, -0.000000000000000000, -0.000000000000000000 ) ) ;
#2718 = CARTESIAN_POINT ( 'NONE',  ( 51.80000000000001847, -4.227689052994008101, -1.125730994152045472 ) ) ;
#2719 = DIRECTION ( 'NONE',  ( 1.000000000000000000, 0.000000000000000000, 0.000000000000000000 ) ) ;
#2721 = CARTESIAN_POINT ( 'NONE',  ( -61.39878663427906247, -2.566070302374152678, -0.8397640680202698160 ) ) ;
#2720 = DIRECTION ( 'NONE',  ( -2.581436205204234499E-16, 0.9796124928211140670, 0.2008964009354147762 ) ) ;
#2722 = LINE ( 'NONE', #20309, #17045 ) ;
#2723 = CARTESIAN_POINT ( 'NONE',  ( 48.43966969621123297, 1.282137971188145320, -3.869545987293864897 ) ) ;
#2725 = CARTESIAN_POINT ( 'NONE',  ( 52.13000000000003098, -0.4999999999994542144, -1.718465885608440269 ) ) ;
#2724 = CARTESIAN_POINT ( 'NONE',  ( 15.03925126672132784, 4.683225679163376398, -2.703237727951165237 ) ) ;
#2726 = EDGE_CURVE ( 'NONE', #9046, #25236, #24063, .T. ) ;
#2727 = ORIENTED_EDGE ( 'NONE', *, *, #25782, .T. ) ;
#2728 = CARTESIAN_POINT ( 'NONE',  ( 51.99335957375618023, 4.356869014081647506, -1.476207528374383848 ) ) ;
#2729 = CARTESIAN_POINT ( 'NONE',  ( 51.77508801986071063, 3.850110376304356929, 1.503046890130784519 ) ) ;
#2731 = CARTESIAN_POINT ( 'NONE',  ( 58.75000000000000711, 1.877732920581273390, 0.6121634413844396772 ) ) ;
#2730 = DIRECTION ( 'NONE',  ( 0.000000000000000000, 0.000000000000000000, 1.000000000000000000 ) ) ;
#2732 = CARTESIAN_POINT ( 'NONE',  ( 47.02556836852575373, -4.052038242240619148, 1.950335525115682644 ) ) ;
#2733 = ORIENTED_EDGE ( 'NONE', *, *, #25922, .T. ) ;
#2734 = B_SPLINE_CURVE_WITH_KNOTS ( 'NONE', 3,
 ( #23364, #11303, #16555, #25884, #23509, #25562 ),
 .UNSPECIFIED., .F., .F.,
 ( 4, 2, 4 ),
 ( 0.000000000000000000, 0.0003974125641964907241, 0.0007948251283929814483 ),
 .UNSPECIFIED. ) ;
#2735 = CARTESIAN_POINT ( 'NONE',  ( -61.37024607392400810, -2.647295961725869784, 0.4804220770584431977 ) ) ;
#2736 = VERTEX_POINT ( 'NONE', #31190 ) ;
#2737 = CIRCLE ( 'NONE', #25485, 2.150647426004269835 ) ;
#2738 = DIRECTION ( 'NONE',  ( -1.000000000000000000, -1.293068473084537258E-16, -0.000000000000000000 ) ) ;
#2739 = ORIENTED_EDGE ( 'NONE', *, *, #19326, .F. ) ;
#2740 = VERTEX_POINT ( 'NONE', #17519 ) ;
#2741 = CARTESIAN_POINT ( 'NONE',  ( 58.66054497608038076, -0.4999999999994944599, -1.807104036850091688 ) ) ;
#2742 = ORIENTED_EDGE ( 'NONE', *, *, #13315, .T. ) ;
#2743 = CARTESIAN_POINT ( 'NONE',  ( 51.94457537908208167, 4.389362525834665796, 1.376356216334040372 ) ) ;
#2744 = CARTESIAN_POINT ( 'NONE',  ( -55.00952994616204705, 3.117691453623994580, -1.800000000000181899 ) ) ;
#2745 = VERTEX_POINT ( 'NONE', #14391 ) ;
#2746 = CARTESIAN_POINT ( 'NONE',  ( -56.22099364905387375, -3.399999999999995026, 0.9110272542656009387 ) ) ;
#2747 = CIRCLE ( 'NONE', #11346, 0.09999999999999982514 ) ;
#2748 = LINE ( 'NONE', #17317, #16749 ) ;
#2749 = AXIS2_PLACEMENT_3D ( 'NONE', #7405, #28791, #14531 ) ;
#2750 = CARTESIAN_POINT ( 'NONE',  ( 48.50000000000002132, -1.409787217987148233, 3.850000000000022737 ) ) ;
#2751 = ORIENTED_EDGE ( 'NONE', *, *, #7123, .T. ) ;
#2752 = EDGE_CURVE ( 'NONE', #8907, #6633, #2373, .T. ) ;
#2753 = CARTESIAN_POINT ( 'NONE',  ( 51.80000000000001847, -4.131056160354152240, -1.100000000000000089 ) ) ;
#2754 = CARTESIAN_POINT ( 'NONE',  ( 58.74999981196286569, -0.9033020670124441986, -1.734557215428337296 ) ) ;
#2755 = CARTESIAN_POINT ( 'NONE',  ( -35.85663232820584057, 0.9159215771349650259, 4.311190327366005270 ) ) ;
#2756 = CARTESIAN_POINT ( 'NONE',  ( 57.00000000000001421, 0.6999999999999999556, 2.452039967047845437 ) ) ;
#2757 = CARTESIAN_POINT ( 'NONE',  ( 54.40000000000001990, 0.000000000000000000, 0.000000000000000000 ) ) ;
#2758 = CIRCLE ( 'NONE', #20475, 1.875000000000001776 ) ;
#2759 = CARTESIAN_POINT ( 'NONE',  ( 51.87924854942583863, -4.254543194710165288, 1.020305229671191416 ) ) ;
#2760 = DIRECTION ( 'NONE',  ( -2.614381936396368743E-16, 0.2008964009354147762, -0.9796124928211139560 ) ) ;
#2761 = EDGE_CURVE ( 'NONE', #21492, #16699, #6541, .T. ) ;
#2762 = CARTESIAN_POINT ( 'NONE',  ( 52.45567523936536958, 8.517307475678970619, 1.943109374214545770 ) ) ;
#2763 = ORIENTED_EDGE ( 'NONE', *, *, #24226, .F. ) ;
#2764 = EDGE_LOOP ( 'NONE', ( #7716, #25036, #18191, #9218, #27487 ) ) ;
#2765 = ORIENTED_EDGE ( 'NONE', *, *, #767, .T. ) ;
#2766 = CARTESIAN_POINT ( 'NONE',  ( -57.77499999999997016, 2.796048871338436190E-15, 1.138853883557972617E-16 ) ) ;
#2767 = CARTESIAN_POINT ( 'NONE',  ( -59.65835481156722864, -3.238593381231841928, -2.874284765127021579 ) ) ;
#2769 = DIRECTION ( 'NONE',  ( 1.000000000000000000, 1.047444401652940007E-14, 0.000000000000000000 ) ) ;
#2768 = DIRECTION ( 'NONE',  ( 0.000000000000000000, 0.000000000000000000, 1.000000000000000000 ) ) ;
#2770 = ORIENTED_EDGE ( 'NONE', *, *, #10004, .F. ) ;
#2771 = AXIS2_PLACEMENT_3D ( 'NONE', #25710, #30445, #11460 ) ;
#2772 = ORIENTED_EDGE ( 'NONE', *, *, #817, .T. ) ;
#2773 = AXIS2_PLACEMENT_3D ( 'NONE', #24761, #539, #14935 ) ;
#2774 = CARTESIAN_POINT ( 'NONE',  ( 53.94302949310494455, 6.378738071910782459, -1.816235364411796116 ) ) ;
#2775 = ORIENTED_EDGE ( 'NONE', *, *, #3509, .F. ) ;
#2776 = CARTESIAN_POINT ( 'NONE',  ( 29.25706191173315673, 5.994885333997870269, -1.950000000000101652 ) ) ;
#2777 = ORIENTED_EDGE ( 'NONE', *, *, #2818, .F. ) ;
#2778 = ORIENTED_EDGE ( 'NONE', *, *, #13678, .T. ) ;
#2779 = AXIS2_PLACEMENT_3D ( 'NONE', #22887, #11146, #6100 ) ;
#2780 = CARTESIAN_POINT ( 'NONE',  ( -58.09599364905385244, 0.2309624077928971175, 3.875409454552790844 ) ) ;
#2781 = CARTESIAN_POINT ( 'NONE',  ( 51.89798357584853505, 4.350000000000017408, 1.495827530165568575 ) ) ;
#2782 = EDGE_CURVE ( 'NONE', #22168, #5779, #5526, .T. ) ;
#2783 = DIRECTION ( 'NONE',  ( 1.027984282060330001E-14, 0.000000000000000000, 1.000000000000000000 ) ) ;
#2784 = AXIS2_PLACEMENT_3D ( 'NONE', #23788, #21417, #631 ) ;
#2785 = CARTESIAN_POINT ( 'NONE',  ( -54.76905989232412963, 2.944486372867092250, 1.699999999999816769 ) ) ;
#2786 = CARTESIAN_POINT ( 'NONE',  ( 53.82520270936414875, 4.899646637710924679, -2.050000000000188116 ) ) ;
#2787 = LINE ( 'NONE', #423, #11966 ) ;
#2788 = DIRECTION ( 'NONE',  ( -1.000000000000000000, 0.000000000000000000, 1.047444401652940007E-14 ) ) ;
#2789 = AXIS2_PLACEMENT_3D ( 'NONE', #19017, #28671, #6987 ) ;
#2790 = CYLINDRICAL_SURFACE ( 'NONE', #2333, 4.849999999999999645 ) ;
#2791 = CIRCLE ( 'NONE', #17473, 4.349999999999997868 ) ;
#2792 = CARTESIAN_POINT ( 'NONE',  ( 68.00000000000004263, 0.5000000000000000000, 1.988246715072646387 ) ) ;
#2793 = VERTEX_POINT ( 'NONE', #21245 ) ;
#2794 = CARTESIAN_POINT ( 'NONE',  ( 57.05000000000001137, -0.7500000000000000000, -2.490438859776672231 ) ) ;
#2795 = CARTESIAN_POINT ( 'NONE',  ( -36.22955757456082893, -3.272340825137205478, -4.050058705652198832 ) ) ;
#2796 = CARTESIAN_POINT ( 'NONE',  ( 54.18130252701728722, 6.361998095200566361, 2.049999999999792877 ) ) ;
#2797 = AXIS2_PLACEMENT_3D ( 'NONE', #16721, #25731, #14318 ) ;
#2798 = EDGE_LOOP ( 'NONE', ( #5175, #12651, #13298, #19894 ) ) ;
#2799 = DIRECTION ( 'NONE',  ( 1.040834085586084257E-14, 0.000000000000000000, 1.000000000000000000 ) ) ;
#2800 = ORIENTED_EDGE ( 'NONE', *, *, #26083, .T. ) ;
#2801 = CIRCLE ( 'NONE', #15935, 1.474464970144730991 ) ;
#2802 = SURFACE_STYLE_FILL_AREA ( #7571 ) ;
#2803 = DIRECTION ( 'NONE',  ( 0.000000000000000000, 0.8660422822663634834, 0.4999707644721521627 ) ) ;
#2805 = CARTESIAN_POINT ( 'NONE',  ( 58.45000000000001705, 0.8000000000000000444, -2.421260002560649660 ) ) ;
#2804 = CARTESIAN_POINT ( 'NONE',  ( 58.65000000000000568, 0.8794134543724719810, 1.656314228059073912 ) ) ;
#2806 = EDGE_CURVE ( 'NONE', #23938, #13242, #2055, .T. ) ;
#2807 = ORIENTED_EDGE ( 'NONE', *, *, #28988, .F. ) ;
#2808 = CARTESIAN_POINT ( 'NONE',  ( -57.45655989232412253, -3.399999999999991029, -2.148039047887444390E-13 ) ) ;
#2809 = CARTESIAN_POINT ( 'NONE',  ( 58.75000000000000000, 1.972190280208565571, -0.1053114364790996849 ) ) ;
#2811 = DIRECTION ( 'NONE',  ( -1.000000000000000000, -0.000000000000000000, 1.047444401652940007E-14 ) ) ;
#2810 = CARTESIAN_POINT ( 'NONE',  ( 53.74996364474760924, 4.800585817144076728, 2.049999999999812417 ) ) ;
#2812 = FACE_OUTER_BOUND ( 'NONE', #24844, .T. ) ;
#2813 = CARTESIAN_POINT ( 'NONE',  ( -58.24999999999997158, 3.673546848079180638, 0.7533615035078061739 ) ) ;
#2814 = DIRECTION ( 'NONE',  ( 1.000000000000000000, 0.000000000000000000, 0.000000000000000000 ) ) ;
#2815 = AXIS2_PLACEMENT_3D ( 'NONE', #16284, #25927, #4230 ) ;
#2816 = CARTESIAN_POINT ( 'NONE',  ( -55.09599364905386665, 0.2309624077929083863, 3.875409454552789956 ) ) ;
#2817 = AXIS2_PLACEMENT_3D ( 'NONE', #301, #19643, #22172 ) ;
#2818 = EDGE_CURVE ( 'NONE', #14302, #28844, #1468, .T. ) ;
#2819 = CARTESIAN_POINT ( 'NONE',  ( 50.25000000000004263, -1.996089927834391764, 0.1250000000000018041 ) ) ;
#2820 = CARTESIAN_POINT ( 'NONE',  ( 50.30000000000001847, -4.899999999999999467, 3.950000000000022826 ) ) ;
#2821 = EDGE_CURVE ( 'NONE', #20943, #1564, #27600, .T. ) ;
#2822 = DIRECTION ( 'NONE',  ( 1.000000000000000000, -0.000000000000000000, -0.000000000000000000 ) ) ;
#2823 = EDGE_CURVE ( 'NONE', #30150, #12308, #9108, .T. ) ;
#2824 = VERTEX_POINT ( 'NONE', #30166 ) ;
#2825 = AXIS2_PLACEMENT_3D ( 'NONE', #21286, #4301, #7017 ) ;
#2826 = CIRCLE ( 'NONE', #7384, 0.1500000000000001887 ) ;
#2827 = CARTESIAN_POINT ( 'NONE',  ( 15.48609859788819954, -3.148602930107186282, 4.139959549308917630 ) ) ;
#2828 = CARTESIAN_POINT ( 'NONE',  ( 28.59102362472352965, 5.695743087063649845, -1.950000000000098321 ) ) ;
#2829 = CARTESIAN_POINT ( 'NONE',  ( 50.50000000000002132, -0.6304760106459029734, 3.950000000000022826 ) ) ;
#2830 = EDGE_CURVE ( 'NONE', #20869, #3677, #30002, .T. ) ;
#2831 = CIRCLE ( 'NONE', #16498, 1.000000000000000000 ) ;
#2832 = FACE_OUTER_BOUND ( 'NONE', #17196, .T. ) ;
#2833 = CIRCLE ( 'NONE', #3341, 2.000000000000000000 ) ;
#2834 = CARTESIAN_POINT ( 'NONE',  ( -73.85208152723558328, -2.420890761855879333E-15, 4.598101673502850081E-15 ) ) ;
#2836 = CARTESIAN_POINT ( 'NONE',  ( 31.18344400622541812, 7.296549944477567884, 1.424999999999891243 ) ) ;
#2835 = DIRECTION ( 'NONE',  ( 0.000000000000000000, 0.000000000000000000, -1.000000000000000000 ) ) ;
#2837 = ORIENTED_EDGE ( 'NONE', *, *, #20652, .T. ) ;
#2838 = DIRECTION ( 'NONE',  ( 0.000000000000000000, 0.000000000000000000, -1.000000000000000000 ) ) ;
#2839 = CIRCLE ( 'NONE', #20569, 0.1500000000000001887 ) ;
#2840 = ORIENTED_EDGE ( 'NONE', *, *, #7061, .T. ) ;
#2841 = UNCERTAINTY_MEASURE_WITH_UNIT (LENGTH_MEASURE( 1.000000000000000082E-05 ), #22345, 'distance_accuracy_value', 'NONE');
#2842 = CARTESIAN_POINT ( 'NONE',  ( 61.00000000000001421, 1.000000000000639044, 1.586072192556190252 ) ) ;
#2844 = CARTESIAN_POINT ( 'NONE',  ( 44.98443556292537693, -3.726179070414207928, -1.000000000000002220 ) ) ;
#2843 = CARTESIAN_POINT ( 'NONE',  ( 57.04458252721509126, 0.7500000000000000000, -2.421260002560649660 ) ) ;
#2845 = FACE_OUTER_BOUND ( 'NONE', #3900, .T. ) ;
#2847 = ADVANCED_FACE ( 'NONE', ( #27640 ), #4004, .T. ) ;
#2846 = AXIS2_PLACEMENT_3D ( 'NONE', #15912, #30631, #6734 ) ;
#2848 = ORIENTED_EDGE ( 'NONE', *, *, #5186, .F. ) ;
#2849 = ORIENTED_EDGE ( 'NONE', *, *, #10793, .T. ) ;
#2850 = CARTESIAN_POINT ( 'NONE',  ( -57.59585481156722864, -2.489203624310587060, 2.804704140674918467 ) ) ;
#2851 = AXIS2_PLACEMENT_3D ( 'NONE', #29246, #7559, #17219 ) ;
#2852 = AXIS2_PLACEMENT_3D ( 'NONE', #10632, #1125, #6191 ) ;
#2853 = CARTESIAN_POINT ( 'NONE',  ( 51.80000000000001137, 4.350000000000017408, -1.495827530165608321 ) ) ;
#2854 = ORIENTED_EDGE ( 'NONE', *, *, #3100, .T. ) ;
#2855 = VECTOR ( 'NONE', #4319, 1000.000000000000000 ) ;
#2856 = EDGE_CURVE ( 'NONE', #8076, #4056, #458, .T. ) ;
#2857 = CARTESIAN_POINT ( 'NONE',  ( 60.75000000000001421, 0.7500000000006363798, -1.718465885608440047 ) ) ;
#2858 = CARTESIAN_POINT ( 'NONE',  ( -55.54792740578360366, -2.256877952708263191, 2.542931754211924300 ) ) ;
#2859 = CARTESIAN_POINT ( 'NONE',  ( -36.63359589171323449, -5.330414537250521612, -0.9106291984479789603 ) ) ;
#2860 = ORIENTED_EDGE ( 'NONE', *, *, #14964, .F. ) ;
#2861 = CARTESIAN_POINT ( 'NONE',  ( 0.000000000000000000, 0.000000000000000000, 0.000000000000000000 ) ) ;
#2862 = FACE_OUTER_BOUND ( 'NONE', #8637, .T. ) ;
#2863 = AXIS2_PLACEMENT_3D ( 'NONE', #26528, #4836, #7540 ) ;
#2864 = EDGE_CURVE ( 'NONE', #16804, #25369, #20220, .T. ) ;
#2865 = EDGE_CURVE ( 'NONE', #6165, #5500, #8545, .T. ) ;
#2866 = ORIENTED_EDGE ( 'NONE', *, *, #3749, .T. ) ;
#2867 = AXIS2_PLACEMENT_3D ( 'NONE', #30258, #21098, #8709 ) ;
#2868 = CARTESIAN_POINT ( 'NONE',  ( -59.69702994616202574, -2.078460969082631227, -3.600000000000218137 ) ) ;
#2869 = VECTOR ( 'NONE', #28675, 1000.000000000000000 ) ;
#2870 = CARTESIAN_POINT ( 'NONE',  ( 52.11563210330034224, 3.836792880204552336, -2.050000000000181455 ) ) ;
#2871 = CARTESIAN_POINT ( 'NONE',  ( 48.43940831342823117, -1.279117291415095448, -3.870058441400159754 ) ) ;
#2872 = CARTESIAN_POINT ( 'NONE',  ( 51.90000000000001279, 1.734723475976807094E-15, 0.000000000000000000 ) ) ;
#2873 = CIRCLE ( 'NONE', #17554, 2.985355339059319046 ) ;
#2874 = CIRCLE ( 'NONE', #24613, 0.1000000000000000472 ) ;
#2875 = CYLINDRICAL_SURFACE ( 'NONE', #30172, 2.000000000000000000 ) ;
#2876 = MECHANICAL_DESIGN_GEOMETRIC_PRESENTATION_REPRESENTATION (  '', ( #17530 ), #347 ) ;
#2878 = CARTESIAN_POINT ( 'NONE',  ( -61.35350676116485857, -2.546188506968221521, -0.8003206670636398012 ) ) ;
#2877 = CARTESIAN_POINT ( 'NONE',  ( 50.55258015808398397, -0.05176326469654482509, -1.177580158083963324 ) ) ;
#2879 = CIRCLE ( 'NONE', #26641, 0.04999999999999969746 ) ;
#2880 = DIRECTION ( 'NONE',  ( 1.000000000000000000, 1.047444401652940007E-14, 0.000000000000000000 ) ) ;
#2881 = CARTESIAN_POINT ( 'NONE',  ( 54.48476976571165409, -0.001523517289327013143, -4.328047699026194017 ) ) ;
#2882 = EDGE_LOOP ( 'NONE', ( #21093, #25984, #3642, #25836 ) ) ;
#2883 = DIRECTION ( 'NONE',  ( -1.000000000000000000, -0.000000000000000000, -0.000000000000000000 ) ) ;
#2884 = CARTESIAN_POINT ( 'NONE',  ( -35.85663232820583346, -5.377732432866659806, -0.5657657256215629094 ) ) ;
#2885 = AXIS2_PLACEMENT_3D ( 'NONE', #24703, #175, #26916 ) ;
#2887 = DIRECTION ( 'NONE',  ( -0.9480661539417394312, 0.3180732113053816867, 0.000000000000000000 ) ) ;
#2886 = CARTESIAN_POINT ( 'NONE',  ( 16.07512358269928399, 2.917650619476306328, -4.554978966839664523 ) ) ;
#2888 = CARTESIAN_POINT ( 'NONE',  ( 47.54437363841991271, -4.350642226022881864, 1.494686490729194572 ) ) ;
#2889 = EDGE_CURVE ( 'NONE', #3831, #19690, #27262, .T. ) ;
#2890 = ORIENTED_EDGE ( 'NONE', *, *, #2709, .F. ) ;
#2891 = CARTESIAN_POINT ( 'NONE',  ( -61.36631426390781030, -2.644259247411960168, 0.4770650455704195658 ) ) ;
#2892 = AXIS2_PLACEMENT_3D ( 'NONE', #5034, #24660, #17090 ) ;
#2893 = ADVANCED_FACE ( 'NONE', ( #10846 ), #8019, .T. ) ;
#2894 = CONICAL_SURFACE ( 'NONE', #25675, 1.487500000000000933, 0.7853981633974481680 ) ;
#2895 = ORIENTED_EDGE ( 'NONE', *, *, #11678, .F. ) ;
#2896 = ADVANCED_FACE ( 'NONE', ( #3432 ), #10591, .F. ) ;
#2897 = CARTESIAN_POINT ( 'NONE',  ( 15.18463186935387910, -5.377732432866779710, 0.5657657256210123498 ) ) ;
#2898 = ORIENTED_EDGE ( 'NONE', *, *, #6137, .T. ) ;
#2899 = ORIENTED_EDGE ( 'NONE', *, *, #16827, .F. ) ;
#2900 = CARTESIAN_POINT ( 'NONE',  ( 15.03925126672132784, 4.683225679163368405, -2.703237727951182112 ) ) ;
#2901 = VERTEX_POINT ( 'NONE', #27328 ) ;
#2902 = CARTESIAN_POINT ( 'NONE',  ( 34.19605798823444331, 8.191999290087634833, 1.949999999999880940 ) ) ;
#2903 = VECTOR ( 'NONE', #1376, 1000.000000000000000 ) ;
#2904 = CARTESIAN_POINT ( 'NONE',  ( -61.07202994616202574, 2.078460969082674747, -3.600000000000208367 ) ) ;
#2905 = EDGE_LOOP ( 'NONE', ( #26280, #1404, #23342, #680 ) ) ;
#2906 = CARTESIAN_POINT ( 'NONE',  ( -44.49999999999997868, 6.542789527549899840E-15, -1.397091617737396343E-15 ) ) ;
#2907 = CIRCLE ( 'NONE', #28164, 2.800000000000000266 ) ;
#2908 = AXIS2_PLACEMENT_3D ( 'NONE', #15482, #4479, #26174 ) ;
#2909 = FACE_OUTER_BOUND ( 'NONE', #16028, .T. ) ;
#2910 = B_SPLINE_CURVE_WITH_KNOTS ( 'NONE', 3,
 ( #24331, #2638, #20054, #12280, #14809, #17211 ),
 .UNSPECIFIED., .F., .F.,
 ( 4, 2, 4 ),
 ( 0.000000000000000000, 0.0001701207528151775234, 0.0003402415056303550469 ),
 .UNSPECIFIED. ) ;
#2911 = DIRECTION ( 'NONE',  ( -1.000000000000000000, -0.000000000000000000, 1.047444401652940007E-14 ) ) ;
#2912 = ORIENTED_EDGE ( 'NONE', *, *, #24728, .T. ) ;
#2913 = CARTESIAN_POINT ( 'NONE',  ( 51.78359321857947606, -4.158733306197476942, -1.045116725612200259 ) ) ;
#2914 = B_SPLINE_CURVE_WITH_KNOTS ( 'NONE', 3,
 ( #22658, #17582, #24989, #27524, #29909, #952, #9988, #27055, #19655, #27226, #10604, #3007, #10444, #22333, #470, #12497 ),
 .UNSPECIFIED., .F., .F.,
 ( 4, 2, 2, 2, 2, 2, 2, 4 ),
 ( 4.367276169273258306E-17, 0.0003166453355160177481, 0.0003958066693950119258, 0.0004353873363345080118, 0.0004452825030693815318, 0.0004551776698042549977, 0.0004749680032740019836, 0.0006332906710319628546 ),
 .UNSPECIFIED. ) ;
#2915 = FACE_OUTER_BOUND ( 'NONE', #2370, .T. ) ;
#2916 = DIRECTION ( 'NONE',  ( 0.000000000000000000, -0.9996898646859344595, -0.02490330187381124133 ) ) ;
#2917 = AXIS2_PLACEMENT_3D ( 'NONE', #6284, #15934, #25594 ) ;
#2918 = DIRECTION ( 'NONE',  ( 1.000000000000000000, -0.000000000000000000, -0.000000000000000000 ) ) ;
#2919 = CARTESIAN_POINT ( 'NONE',  ( 57.02528775048638465, 0.7434661330690420789, 2.425538622349843632 ) ) ;
#2920 = CIRCLE ( 'NONE', #28712, 1.975000000000001865 ) ;
#2921 = CIRCLE ( 'NONE', #6978, 1.899999999999999911 ) ;
#2923 = DIRECTION ( 'NONE',  ( 1.000000000000000000, 1.047444401652940007E-14, 0.000000000000000000 ) ) ;
#2922 = SURFACE_STYLE_FILL_AREA ( #16873 ) ;
#2924 = CARTESIAN_POINT ( 'NONE',  ( 58.66595318830262329, -0.4999999999993857136, 1.807217177072697245 ) ) ;
#2925 = DIRECTION ( 'NONE',  ( 1.000000000000000000, 0.000000000000000000, 0.000000000000000000 ) ) ;
#2926 = CIRCLE ( 'NONE', #17094, 1.625000000000000444 ) ;
#2927 = CARTESIAN_POINT ( 'NONE',  ( 41.48619405472010868, -151.3359592902261852, 1.549999999999835953 ) ) ;
#2928 = CARTESIAN_POINT ( 'NONE',  ( 52.16611735465140498, 8.588510181886395145, 1.949999998429079895 ) ) ;
#2929 = EDGE_LOOP ( 'NONE', ( #4413, #1004, #26925, #14132, #17816, #15391 ) ) ;
#2930 = EDGE_CURVE ( 'NONE', #27818, #20905, #21739, .T. ) ;
#2931 = VERTEX_POINT ( 'NONE', #1349 ) ;
#2932 = ORIENTED_EDGE ( 'NONE', *, *, #610, .F. ) ;
#2933 = EDGE_CURVE ( 'NONE', #22181, #14808, #797, .T. ) ;
#2934 = DIRECTION ( 'NONE',  ( 1.000000000000000000, 1.047444401652940007E-14, 0.000000000000000000 ) ) ;
#2935 = CARTESIAN_POINT ( 'NONE',  ( -60.54792740578359656, -1.073804522883517576, -3.225979517392334905 ) ) ;
#2937 = DIRECTION ( 'NONE',  ( 0.000000000000000000, -1.000000000000000000, -3.491481338843252079E-15 ) ) ;
#2936 = FACE_OUTER_BOUND ( 'NONE', #18568, .T. ) ;
#2938 = VERTEX_POINT ( 'NONE', #11020 ) ;
#2939 = ORIENTED_EDGE ( 'NONE', *, *, #22956, .F. ) ;
#2940 = CARTESIAN_POINT ( 'NONE',  ( 54.15683185445048764, 5.684290329229592764, -2.050000000000188560 ) ) ;
#2941 = CIRCLE ( 'NONE', #21682, 4.100000000000022737 ) ;
#2942 = ORIENTED_EDGE ( 'NONE', *, *, #3426, .F. ) ;
#2943 = CARTESIAN_POINT ( 'NONE',  ( 22.09275828236361150, 6.785783592403105580, -1.950000000000076783 ) ) ;
#2944 = EDGE_LOOP ( 'NONE', ( #6028, #13857, #28987 ) ) ;
#2945 = CARTESIAN_POINT ( 'NONE',  ( 31.77414890219379373, 7.582826004857478708, -1.950000000000077671 ) ) ;
#2946 = EDGE_LOOP ( 'NONE', ( #26559, #27622, #13768, #9867, #4918 ) ) ;
#2947 = DIRECTION ( 'NONE',  ( 3.491481338843133355E-15, 0.000000000000000000, 1.000000000000000000 ) ) ;
#2948 = FACE_OUTER_BOUND ( 'NONE', #7691, .T. ) ;
#2949 = EDGE_CURVE ( 'NONE', #30858, #5493, #3451, .T. ) ;
#2950 = CARTESIAN_POINT ( 'NONE',  ( 15.44631504820156387, -5.012449653004652284, -1.400819699606176583 ) ) ;
#2951 = CARTESIAN_POINT ( 'NONE',  ( -56.01905989232412963, -2.944486372867088697, 1.699999999999789679 ) ) ;
#2952 = CARTESIAN_POINT ( 'NONE',  ( 53.05417955289645704, 8.376364939874980209, -2.050000000000184563 ) ) ;
#2953 = DIRECTION ( 'NONE',  ( 3.016910393003118404E-15, 1.776356839400249479E-15, 1.000000000000000000 ) ) ;
#2954 = DIRECTION ( 'NONE',  ( 0.000000000000000000, 0.000000000000000000, 1.000000000000000000 ) ) ;
#2955 = DIRECTION ( 'NONE',  ( 5.167928589571388008E-15, -0.4531102586341528293, -0.8914544820238951006 ) ) ;
#2956 = PRODUCT_DEFINITION ( 'UNKNOWN', '', #17169, #15507 ) ;
#2957 = AXIS2_PLACEMENT_3D ( 'NONE', #19950, #27379, #27855 ) ;
#2958 = CIRCLE ( 'NONE', #10540, 0.4576450603546999840 ) ;
#2959 = CARTESIAN_POINT ( 'NONE',  ( 51.80000000000001847, 1.029992063861229212E-15, -4.375000000000002665 ) ) ;
#2960 =( BOUNDED_CURVE ( )  B_SPLINE_CURVE ( 2, ( #17855, #15155, #22614 ),
 .UNSPECIFIED., .F., .T. ) 
 B_SPLINE_CURVE_WITH_KNOTS ( ( 3, 3 ),
 ( 0.6944444444444445308, 0.6961765869809276586 ),
 .UNSPECIFIED. ) 
 CURVE ( )  GEOMETRIC_REPRESENTATION_ITEM ( )  RATIONAL_B_SPLINE_CURVE ( ( 0.9330127018922194093, 0.9330127018922194093, 0.9353569697113865988 ) ) 
 REPRESENTATION_ITEM ( '' )  );
#2961 = CARTESIAN_POINT ( 'NONE',  ( 51.19148447764912646, -0.9872860527319672341, 1.295557643792433433 ) ) ;
#2962 = ORIENTED_EDGE ( 'NONE', *, *, #25304, .T. ) ;
#2963 = CARTESIAN_POINT ( 'NONE',  ( -77.28999999999996362, -0.4498604391086740151, -0.01120648584320975590 ) ) ;
#2964 = CARTESIAN_POINT ( 'NONE',  ( 51.59739104186229497, -1.010292945602101256, -1.272765950230260623 ) ) ;
#2965 = CARTESIAN_POINT ( 'NONE',  ( 54.35699702479112716, 6.713389762748565914, 2.043118800226060294 ) ) ;
#2966 = EDGE_LOOP ( 'NONE', ( #7230, #4325, #17494, #23908, #15032, #23931, #24621, #3742, #16342, #6386, #7783, #411, #1237, #24829, #29363, #13803 ) ) ;
#2967 = EDGE_CURVE ( 'NONE', #15088, #12969, #19693, .T. ) ;
#2968 = CARTESIAN_POINT ( 'NONE',  ( -60.59999999999997300, 2.524216908331986975, 0.06288083723137545544 ) ) ;
#2969 = ORIENTED_EDGE ( 'NONE', *, *, #27825, .T. ) ;
#2970 = ADVANCED_FACE ( 'NONE', ( #20839 ), #16151, .T. ) ;
#2971 = DIRECTION ( 'NONE',  ( 1.000000000000000000, 1.047444401652940007E-14, 0.000000000000000000 ) ) ;
#2972 = DIRECTION ( 'NONE',  ( -1.000000000000000000, 0.000000000000000000, 0.000000000000000000 ) ) ;
#2974 = CARTESIAN_POINT ( 'NONE',  ( 27.72148966843209550, 5.417328426838181166, 1.424999999999903233 ) ) ;
#2973 = CARTESIAN_POINT ( 'NONE',  ( 22.04321716858594371, 7.679566743993215816, 1.424999999999923661 ) ) ;
#2975 = EDGE_CURVE ( 'NONE', #11640, #26805, #3884, .T. ) ;
#2976 = ORIENTED_EDGE ( 'NONE', *, *, #26055, .F. ) ;
#2977 = B_SPLINE_CURVE_WITH_KNOTS ( 'NONE', 3,
 ( #12007, #7245, #4867, #12160, #21842, #19447 ),
 .UNSPECIFIED., .F., .F.,
 ( 4, 2, 4 ),
 ( 0.000000000000000000, 0.0001000270069610858788, 0.0002000540139221717575 ),
 .UNSPECIFIED. ) ;
#2978 = CARTESIAN_POINT ( 'NONE',  ( 60.88861521483879358, -0.6775725165974680886, -1.477731239195208879 ) ) ;
#2979 = LINE ( 'NONE', #9792, #28702 ) ;
#2980 = ORIENTED_EDGE ( 'NONE', *, *, #7161, .T. ) ;
#2982 = DIRECTION ( 'NONE',  ( 0.000000000000000000, 0.000000000000000000, -1.000000000000000000 ) ) ;
#2981 = DIRECTION ( 'NONE',  ( 0.000000000000000000, -0.2008964009354147484, 0.9796124928211139560 ) ) ;
#2983 = VERTEX_POINT ( 'NONE', #11648 ) ;
#2984 = CARTESIAN_POINT ( 'NONE',  ( -58.18749999999997158, 3.238593381231845481, 2.874284765127021579 ) ) ;
#2985 = CARTESIAN_POINT ( 'NONE',  ( 57.03612573316699041, -0.7785448249619018046, 1.733167030474859205 ) ) ;
#2986 = CARTESIAN_POINT ( 'NONE',  ( 16.10667815269232861, -3.062358472872038107, -4.459001320275592484 ) ) ;
#2987 = CIRCLE ( 'NONE', #21207, 4.299999999999954525 ) ;
#2988 = LINE ( 'NONE', #10262, #6885 ) ;
#2989 = DIRECTION ( 'NONE',  ( 0.000000000000000000, 0.000000000000000000, 1.000000000000000000 ) ) ;
#2990 = PRODUCT_DEFINITION_SHAPE ( 'NONE', 'NONE',  #27331 ) ;
#2991 = LINE ( 'NONE', #26890, #21480 ) ;
#2992 = CARTESIAN_POINT ( 'NONE',  ( 47.00000000000002132, -3.726179070414207928, 1.710435481158852244 ) ) ;
#2993 = ORIENTED_EDGE ( 'NONE', *, *, #13490, .T. ) ;
#2994 = CARTESIAN_POINT ( 'NONE',  ( 15.87128154250933321, -2.562020839648921910, 4.763023844700866150 ) ) ;
#2995 = AXIS2_PLACEMENT_3D ( 'NONE', #6423, #20993, #16391 ) ;
#2996 = CARTESIAN_POINT ( 'NONE',  ( 52.20711756518982583, 0.7500000000005468959, -1.718465885608440269 ) ) ;
#2997 = DIRECTION ( 'NONE',  ( 3.384826294588897856E-15, 0.000000000000000000, 1.000000000000000000 ) ) ;
#2998 = CARTESIAN_POINT ( 'NONE',  ( -35.85663232820582635, 4.804073783693455724, -2.042134687550313910 ) ) ;
#2999 = CARTESIAN_POINT ( 'NONE',  ( 61.25000000000003553, -0.9840188032644283656, 1.660129320693359167 ) ) ;
#3000 = CARTESIAN_POINT ( 'NONE',  ( 49.00000000000004974, 1.401298464324817071E-42, 2.824999999999485922 ) ) ;
#3001 = ORIENTED_EDGE ( 'NONE', *, *, #8441, .F. ) ;
#3002 = CONICAL_SURFACE ( 'NONE', #10584, 4.375000000000000000, 0.06758856876739828545 ) ;
#3003 = EDGE_CURVE ( 'NONE', #833, #28572, #20711, .T. ) ;
#3004 = DIRECTION ( 'NONE',  ( 1.000000000000000000, 0.000000000000000000, -0.000000000000000000 ) ) ;
#3005 = EDGE_LOOP ( 'NONE', ( #9050, #29255, #21577, #14217 ) ) ;
#3006 = CARTESIAN_POINT ( 'NONE',  ( 51.64837794009021366, -0.8283786772106966900, -1.688958810662479104 ) ) ;
#3008 = CYLINDRICAL_SURFACE ( 'NONE', #6532, 0.9999999999999995559 ) ;
#3007 = CARTESIAN_POINT ( 'NONE',  ( -54.48229591105965142, -2.371389875144092496, -2.684526205802663767 ) ) ;
#3009 = EDGE_CURVE ( 'NONE', #5897, #24423, #18693, .T. ) ;
#3010 = ORIENTED_EDGE ( 'NONE', *, *, #20548, .T. ) ;
#3011 = ORIENTED_EDGE ( 'NONE', *, *, #943, .T. ) ;
#3012 = PLANE ( 'NONE',  #15879 ) ;
#3013 = CARTESIAN_POINT ( 'NONE',  ( 47.19776093000137962, -3.901712759401290143, 1.540267080487876861 ) ) ;
#3014 = VERTEX_POINT ( 'NONE', #23217 ) ;
#3016 = CARTESIAN_POINT ( 'NONE',  ( -59.19766939034450104, 2.421524988789188093, 1.250136525132548693 ) ) ;
#3015 = CARTESIAN_POINT ( 'NONE',  ( -59.00952994616203284, -3.117691453623963938, -1.800000000000220757 ) ) ;
#3017 = DIRECTION ( 'NONE',  ( 1.000000000000000000, 3.054025858079668409E-16, -2.042474015755241579E-16 ) ) ;
#3018 = CARTESIAN_POINT ( 'NONE',  ( -36.31440869660544024, -4.928592478219097295, -1.658905555082604621 ) ) ;
#3019 = EDGE_CURVE ( 'NONE', #20216, #10008, #6581, .T. ) ;
#3020 = CARTESIAN_POINT ( 'NONE',  ( -71.44781903063172024, -1.379665415900875831E-15, 2.906523147574707464E-15 ) ) ;
#3021 = VERTEX_POINT ( 'NONE', #13687 ) ;
#3022 = AXIS2_PLACEMENT_3D ( 'NONE', #18836, #9497, #13885 ) ;
#3023 = AXIS2_PLACEMENT_3D ( 'NONE', #1575, #1906, #30541 ) ;
#3024 = CARTESIAN_POINT ( 'NONE',  ( -57.88452994616205416, 3.117691453623979481, 1.799999999999806422 ) ) ;
#3025 = CARTESIAN_POINT ( 'NONE',  ( 52.80835374156198014, 4.037528258991556207, -2.050000000000183675 ) ) ;
#3026 = CARTESIAN_POINT ( 'NONE',  ( -63.82928932188132620, 2.699162634652023662, 0.06723891505929291412 ) ) ;
#3027 = CARTESIAN_POINT ( 'NONE',  ( 15.29954477411524039, -1.123735554575206574, 5.289358692618363555 ) ) ;
#3028 = EDGE_CURVE ( 'NONE', #28557, #11230, #27764, .T. ) ;
#3029 = CARTESIAN_POINT ( 'NONE',  ( 51.73129885173067066, -4.259946762565045120, -1.000000153509809531 ) ) ;
#3030 = AXIS2_PLACEMENT_3D ( 'NONE', #29194, #4499, #7509 ) ;
#3031 = CARTESIAN_POINT ( 'NONE',  ( -59.69999999999997442, 8.366749974758454467E-15, -2.120534355533670266E-13 ) ) ;
#3033 = CARTESIAN_POINT ( 'NONE',  ( -61.35554497119343864, -2.549885958390812668, -0.8029968850693790516 ) ) ;
#3032 = CARTESIAN_POINT ( 'NONE',  ( -62.09999999999997300, -0.005353951483533918657, 0.2149229472152393294 ) ) ;
#3034 = CARTESIAN_POINT ( 'NONE',  ( 51.17957687186119387, 0.9671124184268959922, -1.523623459118158552 ) ) ;
#3035 = CARTESIAN_POINT ( 'NONE',  ( 69.25000000000001421, 4.557543281186736018E-17, -7.253552481446610839E-13 ) ) ;
#3037 = DIRECTION ( 'NONE',  ( 0.000000000000000000, 0.000000000000000000, 1.000000000000000000 ) ) ;
#3036 = CARTESIAN_POINT ( 'NONE',  ( 54.47883572522132312, -0.001215825626373222409, -4.337530305537235620 ) ) ;
#3038 = ORIENTED_EDGE ( 'NONE', *, *, #18261, .F. ) ;
#3039 = EDGE_CURVE ( 'NONE', #28320, #17715, #15129, .T. ) ;
#3040 = AXIS2_PLACEMENT_3D ( 'NONE', #29692, #20375, #13211 ) ;
#3041 = DIRECTION ( 'NONE',  ( 1.000000000000000000, 3.053848253006669023E-16, -2.042510438544995415E-16 ) ) ;
#3042 = ADVANCED_FACE ( 'NONE', ( #1648, #18627 ), #18463, .T. ) ;
#3043 = CARTESIAN_POINT ( 'NONE',  ( -36.89831264271881395, -5.226279933021941382, -1.394410282272816382 ) ) ;
#3045 = CARTESIAN_POINT ( 'NONE',  ( 51.87760527554365808, 3.845134623358581472, 1.423141017617783444 ) ) ;
#3044 = CARTESIAN_POINT ( 'NONE',  ( 15.61552784268241822, 2.776541361170906885, -4.646985486732077675 ) ) ;
#3047 = EDGE_CURVE ( 'NONE', #21976, #3728, #25735, .T. ) ;
#3046 = CARTESIAN_POINT ( 'NONE',  ( -58.12499999999996447, 2.944486372867111346, -1.700000000000185585 ) ) ;
#3048 = VERTEX_POINT ( 'NONE', #28268 ) ;
#3049 = DIRECTION ( 'NONE',  ( 0.000000000000000000, -1.224646799147343593E-16, 1.000000000000000000 ) ) ;
#3050 = CARTESIAN_POINT ( 'NONE',  ( 68.00000000000002842, 1.401298464324817071E-42, -7.122621931239993559E-13 ) ) ;
#3051 = ORIENTED_EDGE ( 'NONE', *, *, #29412, .F. ) ;
#3052 = CARTESIAN_POINT ( 'NONE',  ( 15.03925126672133139, -5.377732432866647372, 0.5657657256215454789 ) ) ;
#3053 = ORIENTED_EDGE ( 'NONE', *, *, #30454, .F. ) ;
#3054 = ORIENTED_EDGE ( 'NONE', *, *, #28349, .T. ) ;
#3055 = CARTESIAN_POINT ( 'NONE',  ( 16.00221665700882312, 4.939398376933317181, -2.210903708596424710 ) ) ;
#3056 = EDGE_LOOP ( 'NONE', ( #24773, #10858, #16742, #13020 ) ) ;
#3057 = AXIS2_PLACEMENT_3D ( 'NONE', #23501, #8930, #28259 ) ;
#3058 = CARTESIAN_POINT ( 'NONE',  ( 30.65165540517411813, 6.989120292443193883, 1.949999999999893152 ) ) ;
#3059 = CARTESIAN_POINT ( 'NONE',  ( -60.57202994616203995, -4.156921938165296204, -2.298664652687300067E-13 ) ) ;
#3060 = ORIENTED_EDGE ( 'NONE', *, *, #4821, .T. ) ;
#3061 = CARTESIAN_POINT ( 'NONE',  ( 54.48476976571165409, -0.001523517289377870247, 4.328047699026194017 ) ) ;
#3062 = DIRECTION ( 'NONE',  ( 0.000000000000000000, -1.000000000000000000, 0.000000000000000000 ) ) ;
#3063 = CARTESIAN_POINT ( 'NONE',  ( 23.33428888190691453, 6.022557145544392476, 1.949999999999984190 ) ) ;
#3064 = VERTEX_POINT ( 'NONE', #13827 ) ;
#3065 = CARTESIAN_POINT ( 'NONE',  ( 51.75285304771053774, -4.172892586174061336, -1.014428651009326554 ) ) ;
#3066 = CARTESIAN_POINT ( 'NONE',  ( 54.13382992866385024, 5.521407779354435164, -2.050000000000187672 ) ) ;
#3067 = DIRECTION ( 'NONE',  ( 0.000000000000000000, -0.2008964009354147484, 0.9796124928211139560 ) ) ;
#3068 = CARTESIAN_POINT ( 'NONE',  ( 51.70000000000003126, -4.020776289669855785, 2.234582293948397691 ) ) ;
#3069 = EDGE_CURVE ( 'NONE', #25469, #1935, #2831, .T. ) ;
#3070 = CARTESIAN_POINT ( 'NONE',  ( 51.16540481435728793, 0.9540520100826064276, 1.477289350867987405 ) ) ;
#3071 = ADVANCED_FACE ( 'NONE', ( #18782 ), #13940, .T. ) ;
#3073 = FACE_OUTER_BOUND ( 'NONE', #29067, .T. ) ;
#3072 = CARTESIAN_POINT ( 'NONE',  ( -36.22909104983144601, -3.722832355337217791, 3.938244298533509991 ) ) ;
#3074 = TOROIDAL_SURFACE ( 'NONE', #21799, 2.299325721147392088, 0.05000000000000000278 ) ;
#3075 = CARTESIAN_POINT ( 'NONE',  ( 51.34441612831281532, 1.002608958138276440, 1.395204572094387085 ) ) ;
#3076 = DIRECTION ( 'NONE',  ( 0.000000000000000000, 0.000000000000000000, -1.000000000000000000 ) ) ;
#3077 = CARTESIAN_POINT ( 'NONE',  ( 58.72419296898062413, 1.357170036000971081, -1.293880926823457456 ) ) ;
#3078 = CARTESIAN_POINT ( 'NONE',  ( 52.41172327503544182, 8.636713207008101634, -2.050000000000181455 ) ) ;
#3079 = ORIENTED_EDGE ( 'NONE', *, *, #6579, .T. ) ;
#3080 = CARTESIAN_POINT ( 'NONE',  ( 51.45655683570191741, -0.9591657938390835136, 1.468576096419531574 ) ) ;
#3081 = ORIENTED_EDGE ( 'NONE', *, *, #1365, .F. ) ;
#3082 = VERTEX_POINT ( 'NONE', #21327 ) ;
#3083 = CARTESIAN_POINT ( 'NONE',  ( -62.08544523815352534, -2.505505003946113973, -0.3131916526553849556 ) ) ;
#3084 = CARTESIAN_POINT ( 'NONE',  ( -58.11042740578360366, 3.725040285533370632, -1.239922660687675871 ) ) ;
#3086 = CARTESIAN_POINT ( 'NONE',  ( -60.84484350713346146, -2.494647975071613732, 0.8490225916460741873 ) ) ;
#3085 = DIRECTION ( 'NONE',  ( 0.000000000000000000, 0.2793919678926571892, -0.9601771338024398528 ) ) ;
#3087 = ORIENTED_EDGE ( 'NONE', *, *, #20145, .T. ) ;
#3088 = ORIENTED_EDGE ( 'NONE', *, *, #25651, .T. ) ;
#3089 = CARTESIAN_POINT ( 'NONE',  ( 54.07867252728983942, 6.687441468603865680, -2.033313965204277540 ) ) ;
#3090 = ORIENTED_EDGE ( 'NONE', *, *, #19574, .T. ) ;
#3091 = CARTESIAN_POINT ( 'NONE',  ( 51.44193764627932808, 0.9752197701250188144, -1.304631266258923006 ) ) ;
#3092 = ORIENTED_EDGE ( 'NONE', *, *, #18636, .F. ) ;
#3093 = CARTESIAN_POINT ( 'NONE',  ( 26.92903764425373581, 5.249711979700405706, -2.050000000000161915 ) ) ;
#3094 = ORIENTED_EDGE ( 'NONE', *, *, #7320, .F. ) ;
#3095 = DIRECTION ( 'NONE',  ( -0.000000000000000000, 1.000000000000000000, 1.224646799147353207E-16 ) ) ;
#3096 = VERTEX_POINT ( 'NONE', #9274 ) ;
#3097 = CARTESIAN_POINT ( 'NONE',  ( 15.74504787372189085, -5.074157625981885467, -1.874066637979881822 ) ) ;
#3098 = CARTESIAN_POINT ( 'NONE',  ( -59.58155989232410832, -1.962990915244706924, -3.400000000000217515 ) ) ;
#3099 = CARTESIAN_POINT ( 'NONE',  ( 53.93929004300591856, 7.474130129650688126, -2.050000000000187228 ) ) ;
#3100 = EDGE_CURVE ( 'NONE', #20522, #3896, #4349, .T. ) ;
#3101 = CARTESIAN_POINT ( 'NONE',  ( 47.86868016046713592, -3.937842567657670489, -1.145831922971770611 ) ) ;
#3102 = ADVANCED_FACE ( 'NONE', ( #16561 ), #9433, .T. ) ;
#3103 = DIRECTION ( 'NONE',  ( -1.000000000000000000, -0.000000000000000000, 3.491481338843133355E-15 ) ) ;
#3104 = ADVANCED_FACE ( 'NONE', ( #4517 ), #13166, .T. ) ;
#3105 = FACE_OUTER_BOUND ( 'NONE', #9254, .T. ) ;
#3106 = FACE_OUTER_BOUND ( 'NONE', #3671, .T. ) ;
#3107 = CARTESIAN_POINT ( 'NONE',  ( -58.59585481156723574, 3.673546848079181970, 0.7533615035078067290 ) ) ;
#3108 = CARTESIAN_POINT ( 'NONE',  ( 57.00000000000001421, -0.7500000000000000000, 3.499999999999999556 ) ) ;
#3109 = AXIS2_PLACEMENT_3D ( 'NONE', #8983, #13862, #18657 ) ;
#3110 = CARTESIAN_POINT ( 'NONE',  ( -35.85663232820584057, 3.056483311920880297, -4.206888370749704897 ) ) ;
#3111 = EDGE_LOOP ( 'NONE', ( #5349, #1535, #31123, #17405 ) ) ;
#3112 = B_SPLINE_CURVE_WITH_KNOTS ( 'NONE', 3,
 ( #19978, #15222, #3034, #22054 ),
 .UNSPECIFIED., .F., .F.,
 ( 4, 4 ),
 ( 2.168404344971008868E-19, 0.0001476506082772737762 ),
 .UNSPECIFIED. ) ;
#3113 = DIRECTION ( 'NONE',  ( -1.000000000000000000, -3.054025858079668409E-16, 2.042474015755241579E-16 ) ) ;
#3114 = CARTESIAN_POINT ( 'NONE',  ( -36.92443669619772351, -3.051830235923030266, -4.466755975380271693 ) ) ;
#3115 = CARTESIAN_POINT ( 'NONE',  ( 54.27563121892215747, 6.003154427583493380, 2.049999999999808420 ) ) ;
#3116 = EDGE_LOOP ( 'NONE', ( #8128, #12278, #22121, #22936 ) ) ;
#3117 = EDGE_CURVE ( 'NONE', #24431, #23786, #25591, .T. ) ;
#3118 = FACE_OUTER_BOUND ( 'NONE', #13555, .T. ) ;
#3119 = EDGE_LOOP ( 'NONE', ( #8561, #10506, #21653, #15777 ) ) ;
#3120 =( REPRESENTATION_RELATIONSHIP ('NONE','NONE', #7047, #25673 ) REPRESENTATION_RELATIONSHIP_WITH_TRANSFORMATION ( #2196 )SHAPE_REPRESENTATION_RELATIONSHIP( ) );
#3121 = CARTESIAN_POINT ( 'NONE',  ( -77.29999999999998295, 0.2599193648183395489, 0.006474858487196258165 ) ) ;
#3122 = CARTESIAN_POINT ( 'NONE',  ( 51.25000000000001421, 5.368152558471320595E-13, 3.111507638930570854E-58 ) ) ;
#3124 = CARTESIAN_POINT ( 'NONE',  ( 58.65000000000000568, 1.394635017528131904, 1.253243060178682144 ) ) ;
#3123 = CARTESIAN_POINT ( 'NONE',  ( -59.29999999999997584, 0.6177564328764025836, -3.012308415424925556 ) ) ;
#3125 = VERTEX_POINT ( 'NONE', #18106 ) ;
#3126 = ORIENTED_EDGE ( 'NONE', *, *, #29024, .F. ) ;
#3127 = B_SPLINE_CURVE_WITH_KNOTS ( 'NONE', 3,
 ( #6196, #5725, #15547, #20465, #20315, #1129, #18246, #25025, #29945, #8411, #25352, #10782, #25200, #15844, #25496, #3808 ),
 .UNSPECIFIED., .F., .F.,
 ( 4, 2, 2, 2, 2, 2, 2, 4 ),
 ( 0.000000000000000000, 0.0004351083927046398795, 0.0008702167854092797590, 0.001740433570818559518, 0.002175541963523200048, 0.002610650356227840578, 0.003045758748932481542, 0.003480867141637122072 ),
 .UNSPECIFIED. ) ;
#3128 = CARTESIAN_POINT ( 'NONE',  ( -57.58155989232413674, -1.962990915244744006, 3.399999999999780087 ) ) ;
#3129 = CARTESIAN_POINT ( 'NONE',  ( -77.28999999999996362, 0.4398635404618077005, 0.01095745282448230135 ) ) ;
#3130 = AXIS2_PLACEMENT_3D ( 'NONE', #13486, #23470, #9230 ) ;
#3131 = VERTEX_POINT ( 'NONE', #3984 ) ;
#3133 = CARTESIAN_POINT ( 'NONE',  ( -54.45487361440510909, -1.499999999999999556, -4.029888335921975262 ) ) ;
#3132 = PLANE ( 'NONE',  #8991 ) ;
#3134 = DIRECTION ( 'NONE',  ( -1.000000000000000000, 0.000000000000000000, 3.491481338843133355E-15 ) ) ;
#3135 = EDGE_LOOP ( 'NONE', ( #3562, #28766, #24879, #14573 ) ) ;
#3136 = CARTESIAN_POINT ( 'NONE',  ( -57.49999999999997158, 3.673546848079180638, 0.7533615035078060629 ) ) ;
#3137 = DIRECTION ( 'NONE',  ( 3.002035892788117459E-16, -0.9996898646859343485, -0.02490330187381124480 ) ) ;
#3138 = CIRCLE ( 'NONE', #8681, 1.000000000000000000 ) ;
#3139 = AXIS2_PLACEMENT_3D ( 'NONE', #20012, #12399, #7980 ) ;
#3140 = CARTESIAN_POINT ( 'NONE',  ( -54.99999999999997868, -2.489203624310585283, 2.804704140674916690 ) ) ;
#3141 = CARTESIAN_POINT ( 'NONE',  ( 57.00000000000001421, -0.6999999999999999556, -1.820027472320129736 ) ) ;
#3142 = DIRECTION ( 'NONE',  ( 0.000000000000000000, 0.02490330187380866006, -0.9996898646859344595 ) ) ;
#3143 = DIRECTION ( 'NONE',  ( 1.000000000000000000, 0.000000000000000000, -0.000000000000000000 ) ) ;
#3144 = ORIENTED_EDGE ( 'NONE', *, *, #9670, .T. ) ;
#3145 = EDGE_CURVE ( 'NONE', #23000, #3568, #6893, .T. ) ;
#3146 =( BOUNDED_CURVE ( )  B_SPLINE_CURVE ( 3, ( #15173, #10115, #24825, #12941 ),
 .UNSPECIFIED., .F., .T. ) 
 B_SPLINE_CURVE_WITH_KNOTS ( ( 4, 4 ),
 ( 1.358646995387534862, 1.449211172151202653 ),
 .UNSPECIFIED. ) 
 CURVE ( )  GEOMETRIC_REPRESENTATION_ITEM ( )  RATIONAL_B_SPLINE_CURVE ( ( 1.000000000000000000, 0.9993166276053078168, 0.9993166276053078168, 1.000000000000000000 ) ) 
 REPRESENTATION_ITEM ( '' )  );
#3147 = CARTESIAN_POINT ( 'NONE',  ( 15.44631504820161716, 3.231775792180334061, 4.079530926931304258 ) ) ;
#3148 = CARTESIAN_POINT ( 'NONE',  ( -60.62613029541262222, -2.511626612308461404, 0.9750051806848812896 ) ) ;
#3149 = CARTESIAN_POINT ( 'NONE',  ( 51.70000000000001705, -0.1421112804877788793, -1.100000000000000089 ) ) ;
#3150 = CARTESIAN_POINT ( 'NONE',  ( -59.40362242792826919, 3.375967812128700452, 1.250136525132546916 ) ) ;
#3151 = CARTESIAN_POINT ( 'NONE',  ( 22.20323573143550178, 7.488806638634509127, 2.049999999999922107 ) ) ;
#3152 = ORIENTED_EDGE ( 'NONE', *, *, #27235, .F. ) ;
#3153 = EDGE_CURVE ( 'NONE', #28946, #22153, #13621, .T. ) ;
#3154 = PLANE ( 'NONE',  #15838 ) ;
#3155 = ORIENTED_EDGE ( 'NONE', *, *, #26129, .T. ) ;
#3156 = PRODUCT_DEFINITION_CONTEXT ( 'detailed design', #26971, 'design' ) ;
#3157 = FACE_OUTER_BOUND ( 'NONE', #26227, .T. ) ;
#3159 = CARTESIAN_POINT ( 'NONE',  ( 58.75000000000002132, -0.4999999999991823207, -1.863080903343696137 ) ) ;
#3158 = DIRECTION ( 'NONE',  ( 0.000000000000000000, 0.000000000000000000, 1.000000000000000000 ) ) ;
#3160 = ORIENTED_EDGE ( 'NONE', *, *, #20049, .T. ) ;
#3161 = ORIENTED_EDGE ( 'NONE', *, *, #3819, .F. ) ;
#3162 = CARTESIAN_POINT ( 'NONE',  ( 58.45000000000001705, 0.7500000000000000000, -2.421260002560649660 ) ) ;
#3163 = DIRECTION ( 'NONE',  ( -1.000000000000000000, 0.000000000000000000, 0.000000000000000000 ) ) ;
#3164 = ORIENTED_EDGE ( 'NONE', *, *, #4179, .F. ) ;
#3166 = CARTESIAN_POINT ( 'NONE',  ( 51.80000000000001847, -4.137078223593629644, 1.088692053889325217 ) ) ;
#3165 = CARTESIAN_POINT ( 'NONE',  ( -56.63452994616203284, 2.093608279459369510E-14, -3.600000000000201261 ) ) ;
#3167 = CARTESIAN_POINT ( 'NONE',  ( -54.48542740578361077, 0.7887156198831670739, -3.845940847736174728 ) ) ;
#3168 = AXIS2_PLACEMENT_3D ( 'NONE', #2141, #16570, #18944 ) ;
#3169 = CARTESIAN_POINT ( 'NONE',  ( 51.80000000000001847, -3.726179070414207928, -1.710435481158852467 ) ) ;
#3170 = CARTESIAN_POINT ( 'NONE',  ( 0.000000000000000000, 0.000000000000000000, 0.000000000000000000 ) ) ;
#3171 = CARTESIAN_POINT ( 'NONE',  ( -61.34999999999997300, -2.600201727571727517, 0.4583662226975599441 ) ) ;
#3172 =( NAMED_UNIT ( * ) PLANE_ANGLE_UNIT ( ) SI_UNIT ( $, .RADIAN. ) );
#3173 = ORIENTED_EDGE ( 'NONE', *, *, #13867, .T. ) ;
#3174 = EDGE_CURVE ( 'NONE', #16870, #31166, #2344, .T. ) ;
#3175 = CARTESIAN_POINT ( 'NONE',  ( -57.32202994616202574, 2.078460969082674747, -3.600000000000194600 ) ) ;
#3176 = CARTESIAN_POINT ( 'NONE',  ( -39.16187796471576377, -1.705048840508494473E-14, 0.000000000000000000 ) ) ;
#3177 = CARTESIAN_POINT ( 'NONE',  ( -56.45655989232411542, 1.962990915244759771, -3.400000000000185540 ) ) ;
#3179 = ADVANCED_FACE ( 'NONE', ( #15717 ), #6358, .T. ) ;
#3178 = CARTESIAN_POINT ( 'NONE',  ( -54.49999999999999289, -1.400000000000006795, 3.959797974644449603 ) ) ;
#3180 = CARTESIAN_POINT ( 'NONE',  ( 51.89999993196679640, -4.241636233590472926, -1.073352279313352087 ) ) ;
#3181 = DIRECTION ( 'NONE',  ( 1.000000000000000000, 0.000000000000000000, -3.491481338843133355E-15 ) ) ;
#3183 = CYLINDRICAL_SURFACE ( 'NONE', #23527, 0.1500000000000001887 ) ;
#3182 = CARTESIAN_POINT ( 'NONE',  ( -63.82928932188132620, 6.399178848011186396E-16, 2.550935903222500290E-15 ) ) ;
#3184 = VECTOR ( 'NONE', #14103, 1000.000000000000000 ) ;
#3185 = DIRECTION ( 'NONE',  ( 0.000000000000000000, -0.9663289263986323263, -0.2573099415204678220 ) ) ;
#3186 = CARTESIAN_POINT ( 'NONE',  ( 15.32752150720753725, -2.228039998204434102, 4.927410888447834481 ) ) ;
#3188 = FACE_OUTER_BOUND ( 'NONE', #26019, .T. ) ;
#3187 = DIRECTION ( 'NONE',  ( -1.000000000000000000, -1.047444401652940007E-14, -0.000000000000000000 ) ) ;
#3189 = EDGE_LOOP ( 'NONE', ( #5675, #9137, #1698, #24754 ) ) ;
#3190 = CARTESIAN_POINT ( 'NONE',  ( -59.09999999999998010, 2.308634493194285486, 1.301040651491358169 ) ) ;
#3191 = DIRECTION ( 'NONE',  ( 1.000000000000000000, 0.000000000000000000, 0.000000000000000000 ) ) ;
#3193 = DIRECTION ( 'NONE',  ( 1.000000000000000000, 1.047444401652940007E-14, 0.000000000000000000 ) ) ;
#3192 = CARTESIAN_POINT ( 'NONE',  ( 15.95705409078441583, 2.672993279333413241, -4.702725322014949860 ) ) ;
#3194 = CARTESIAN_POINT ( 'NONE',  ( 47.44420282665343080, -4.328226263800974749, 1.560066312054830151 ) ) ;
#3195 = ORIENTED_EDGE ( 'NONE', *, *, #11695, .F. ) ;
#3196 = CARTESIAN_POINT ( 'NONE',  ( -61.39623369212913673, -2.653156182710691535, 0.4999952066012984808 ) ) ;
#3197 = CARTESIAN_POINT ( 'NONE',  ( -60.59999999999997300, -2.431313162469589173, -1.066416437073405499 ) ) ;
#3198 = VERTEX_POINT ( 'NONE', #8266 ) ;
#3199 = DIRECTION ( 'NONE',  ( 0.000000000000000000, 1.000000000000000000, 0.000000000000000000 ) ) ;
#3200 = ORIENTED_EDGE ( 'NONE', *, *, #23820, .F. ) ;
#3201 = EDGE_CURVE ( 'NONE', #3677, #20124, #24572, .T. ) ;
#3202 = ORIENTED_EDGE ( 'NONE', *, *, #25541, .T. ) ;
#3203 = CARTESIAN_POINT ( 'NONE',  ( 15.59140265158955430, 5.360483378448146041, -0.7132926830812214014 ) ) ;
#3204 = EDGE_LOOP ( 'NONE', ( #12274, #24194, #26446, #18263, #22081 ) ) ;
#3205 =( NAMED_UNIT ( * ) PLANE_ANGLE_UNIT ( ) SI_UNIT ( $, .RADIAN. ) );
#3206 = CARTESIAN_POINT ( 'NONE',  ( 34.56702326949726256, 8.213851659285209550, 1.949999999999879385 ) ) ;
#3207 = CARTESIAN_POINT ( 'NONE',  ( -60.50952994616203284, -3.117691453623963938, -1.800000000000225864 ) ) ;
#3208 = VERTEX_POINT ( 'NONE', #13307 ) ;
#3209 = CARTESIAN_POINT ( 'NONE',  ( 54.49932581792542408, -0.002837702349018913269, 4.287546236934917765 ) ) ;
#3210 = ORIENTED_EDGE ( 'NONE', *, *, #25069, .F. ) ;
#3211 = AXIS2_PLACEMENT_3D ( 'NONE', #5499, #20080, #29257 ) ;
#3212 = DIRECTION ( 'NONE',  ( 0.000000000000000000, -1.000000000000000000, 0.000000000000000000 ) ) ;
#3213 = AXIS2_PLACEMENT_3D ( 'NONE', #19230, #16692, #27261 ) ;
#3214 = CARTESIAN_POINT ( 'NONE',  ( 24.21299357973638067, 5.692280404211449429, 2.049999999999915001 ) ) ;
#3215 = ORIENTED_EDGE ( 'NONE', *, *, #27783, .F. ) ;
#3216 = EDGE_CURVE ( 'NONE', #23636, #23889, #18934, .T. ) ;
#3217 = B_SPLINE_CURVE_WITH_KNOTS ( 'NONE', 3,
 ( #3981, #7155, #13936, #23935 ),
 .UNSPECIFIED., .F., .F.,
 ( 4, 4 ),
 ( 0.1946945739040590595, 0.4911851874284507424 ),
 .UNSPECIFIED. ) ;
#3218 = CARTESIAN_POINT ( 'NONE',  ( -54.49999999999996447, 2.023778652682504319E-14, -3.400000000000193978 ) ) ;
#3219 = EDGE_CURVE ( 'NONE', #6099, #11926, #15951, .T. ) ;
#3220 = CARTESIAN_POINT ( 'NONE',  ( 58.75000000000001421, 0.6121634413844194711, -1.877732920580865050 ) ) ;
#3221 = DIRECTION ( 'NONE',  ( -1.000000000000000000, 0.000000000000000000, 0.000000000000000000 ) ) ;
#3223 = EDGE_CURVE ( 'NONE', #171, #9260, #10953, .T. ) ;
#3222 = CARTESIAN_POINT ( 'NONE',  ( 56.97542489291938494, -0.7477441023849552559, -1.746698826563745977 ) ) ;
#3224 = LINE ( 'NONE', #22548, #7435 ) ;
#3226 = DIRECTION ( 'NONE',  ( 2.459562394685749209E-16, -0.9510565162951544194, 0.3090169943749447312 ) ) ;
#3225 = DIRECTION ( 'NONE',  ( 0.000000000000000000, 0.000000000000000000, 1.000000000000000000 ) ) ;
#3227 = CARTESIAN_POINT ( 'NONE',  ( 51.80000000000003979, 2.428612866367529932E-14, 4.199999999999811884 ) ) ;
#3228 = CARTESIAN_POINT ( 'NONE',  ( -59.69999155897362186, 2.119262223567999648, 1.750121904846017262 ) ) ;
#3229 = CARTESIAN_POINT ( 'NONE',  ( 33.47623932017462778, 1.734723475976807094E-15, 0.000000000000000000 ) ) ;
#3230 = EDGE_CURVE ( 'NONE', #23119, #11471, #5677, .T. ) ;
#3231 = CARTESIAN_POINT ( 'NONE',  ( 48.30000000000001847, -0.6462379109120514054, 4.048750000000023164 ) ) ;
#3232 = AXIS2_PLACEMENT_3D ( 'NONE', #3050, #824, #8112 ) ;
#3233 = ORIENTED_EDGE ( 'NONE', *, *, #28271, .F. ) ;
#3234 = CARTESIAN_POINT ( 'NONE',  ( -59.69931151237160805, -2.442379059721019541, -1.238141110944712242 ) ) ;
#3235 = ORIENTED_EDGE ( 'NONE', *, *, #30579, .F. ) ;
#3236 = VERTEX_POINT ( 'NONE', #27428 ) ;
#3237 = CARTESIAN_POINT ( 'NONE',  ( -62.09716160983483491, -2.507809103222365721, -0.2941402757104731314 ) ) ;
#3238 = CARTESIAN_POINT ( 'NONE',  ( -57.42292740578360366, 2.256877952708269408, -2.542931754211925188 ) ) ;
#3240 = CARTESIAN_POINT ( 'NONE',  ( -61.39878663427906957, -2.604700304447900017, 0.7109548583936591282 ) ) ;
#3239 = CYLINDRICAL_SURFACE ( 'NONE', #2422, 3.750000000000000444 ) ;
#3241 = ORIENTED_EDGE ( 'NONE', *, *, #8062, .F. ) ;
#3242 = ADVANCED_FACE ( 'NONE', ( #832 ), #825, .T. ) ;
#3243 = ORIENTED_EDGE ( 'NONE', *, *, #24868, .F. ) ;
#3244 = AXIS2_PLACEMENT_3D ( 'NONE', #7705, #29712, #19762 ) ;
#3245 = CARTESIAN_POINT ( 'NONE',  ( 50.80000000000001847, -4.417905791132255899, -1.285520503972919615 ) ) ;
#3246 = ORIENTED_EDGE ( 'NONE', *, *, #22066, .T. ) ;
#3247 = CARTESIAN_POINT ( 'NONE',  ( 51.38214458811555829, 1.084857585946179315, -1.209959298770756808 ) ) ;
#3248 = ORIENTED_EDGE ( 'NONE', *, *, #7501, .F. ) ;
#3249 = CARTESIAN_POINT ( 'NONE',  ( 31.50816695980852700, 7.454773700473188214, -2.050000000000237854 ) ) ;
#3250 = ADVANCED_FACE ( 'NONE', ( #5739 ), #28634, .T. ) ;
#3251 = CARTESIAN_POINT ( 'NONE',  ( 50.75360625943719839, 0.3719558471750604722, -1.344678919698701014 ) ) ;
#3252 = CARTESIAN_POINT ( 'NONE',  ( 51.31572262954153985, -0.7526089581371979698, -1.996089927833914146 ) ) ;
#3253 = VECTOR ( 'NONE', #9511, 1000.000000000000000 ) ;
#3254 = CARTESIAN_POINT ( 'NONE',  ( 15.68751737981906125, -5.024465639091984848, -2.007392901578175515 ) ) ;
#3255 = EDGE_CURVE ( 'NONE', #7825, #25236, #31157, .T. ) ;
#3257 = CARTESIAN_POINT ( 'NONE',  ( -60.89405989232410121, 2.944486372867106461, -1.700000000000203348 ) ) ;
#3256 = AXIS2_PLACEMENT_3D ( 'NONE', #9828, #19494, #5079 ) ;
#3259 = ADVANCED_FACE ( 'NONE', ( #6674 ), #9921, .T. ) ;
#3258 = FACE_OUTER_BOUND ( 'NONE', #23705, .T. ) ;
#3260 = CARTESIAN_POINT ( 'NONE',  ( 58.64999999999999147, 1.793030239489902478, 0.5493518053835514392 ) ) ;
#3261 = DIRECTION ( 'NONE',  ( 1.000000000000000000, 3.053848253006669023E-16, -2.042510438544995415E-16 ) ) ;
#3262 = CARTESIAN_POINT ( 'NONE',  ( 58.75000000000000711, 0.8948927608033926395, 1.760622601997029912 ) ) ;
#3263 = DIRECTION ( 'NONE',  ( 0.000000000000000000, 0.000000000000000000, 1.000000000000000000 ) ) ;
#3264 = AXIS2_PLACEMENT_3D ( 'NONE', #8768, #18933, #21165 ) ;
#3265 = LINE ( 'NONE', #22761, #28622 ) ;
#3266 = CARTESIAN_POINT ( 'NONE',  ( -44.49999999999997868, -2.624185894800571628, -0.06537116741875388659 ) ) ;
#3267 = CARTESIAN_POINT ( 'NONE',  ( -36.14504829323105639, 1.093755498983955521, 5.295967089285810836 ) ) ;
#3268 = ORIENTED_EDGE ( 'NONE', *, *, #2681, .T. ) ;
#3269 = PRESENTATION_LAYER_ASSIGNMENT (  '', '', ( #26026 ) ) ;
#3270 = AXIS2_PLACEMENT_3D ( 'NONE', #13221, #20700, #30471 ) ;
#3271 = CARTESIAN_POINT ( 'NONE',  ( 51.70000000000002416, 2.428612866367529932E-14, -1.805095852181900386E-13 ) ) ;
#3272 = CARTESIAN_POINT ( 'NONE',  ( 54.28362898602030384, 5.641750290588808170, 1.990863471608376845 ) ) ;
#3273 = VERTEX_POINT ( 'NONE', #11421 ) ;
#3274 = DIRECTION ( 'NONE',  ( -1.047444401652940007E-14, 0.000000000000000000, -1.000000000000000000 ) ) ;
#3275 = ORIENTED_EDGE ( 'NONE', *, *, #27382, .F. ) ;
#3276 = CARTESIAN_POINT ( 'NONE',  ( 69.20000000000001705, -0.5000000000000000000, -1.988246715074081017 ) ) ;
#3277 = VECTOR ( 'NONE', #14339, 1000.000000000000000 ) ;
#3278 = LINE ( 'NONE', #12924, #23405 ) ;
#3280 = CARTESIAN_POINT ( 'NONE',  ( 51.77510471295143901, -3.758556366959755035, -1.867213167016891218 ) ) ;
#3279 = CARTESIAN_POINT ( 'NONE',  ( 51.36025231009421788, -4.327031471043523148, 1.563408443048849072 ) ) ;
#3281 = ORIENTED_EDGE ( 'NONE', *, *, #20931, .F. ) ;
#3282 = EDGE_CURVE ( 'NONE', #29056, #11687, #30129, .T. ) ;
#3283 = CARTESIAN_POINT ( 'NONE',  ( 60.75000000000002132, -0.4999999999993638977, -1.718465885608440047 ) ) ;
#3284 = ADVANCED_FACE ( 'NONE', ( #9371 ), #19229, .F. ) ;
#3285 = DIRECTION ( 'NONE',  ( 0.000000000000000000, 0.000000000000000000, 1.000000000000000000 ) ) ;
#3286 = ORIENTED_EDGE ( 'NONE', *, *, #1652, .T. ) ;
#3288 = FACE_OUTER_BOUND ( 'NONE', #18600, .T. ) ;
#3287 = CARTESIAN_POINT ( 'NONE',  ( 53.96142581635486124, 5.170113101904351360, 2.049999999999811529 ) ) ;
#3289 = AXIS2_PLACEMENT_3D ( 'NONE', #995, #664, #22701 ) ;
#3290 = ADVANCED_FACE ( 'NONE', ( #7008 ), #1751, .T. ) ;
#3291 = ORIENTED_EDGE ( 'NONE', *, *, #3449, .F. ) ;
#3292 = ORIENTED_EDGE ( 'NONE', *, *, #2244, .T. ) ;
#3293 = CARTESIAN_POINT ( 'NONE',  ( 50.59602332238209499, -0.1408342061598474859, 1.212874140286674285 ) ) ;
#3294 = DIRECTION ( 'NONE',  ( 1.000000000000000000, 3.054025858079668409E-16, -2.042474015755241579E-16 ) ) ;
#3295 = CARTESIAN_POINT ( 'NONE',  ( 65.00000000000002842, 1.401298464324817071E-42, -6.808388610744111684E-13 ) ) ;
#3296 = CARTESIAN_POINT ( 'NONE',  ( -54.74999999999997868, -1.184343223768585140, -3.558065644182724085 ) ) ;
#3297 = CARTESIAN_POINT ( 'NONE',  ( -59.69999999999998153, 0.3248756580930906579, -3.465281767758778386 ) ) ;
#3298 = CARTESIAN_POINT ( 'NONE',  ( -54.63452994616206126, -3.117691453623976816, 1.799999999999793765 ) ) ;
#3300 = ORIENTED_EDGE ( 'NONE', *, *, #17085, .T. ) ;
#3299 = VECTOR ( 'NONE', #11724, 1000.000000000000000 ) ;
#3301 = CARTESIAN_POINT ( 'NONE',  ( 15.03925126672132961, -2.686240680702166816, 4.475885388010711452 ) ) ;
#3302 = AXIS2_PLACEMENT_3D ( 'NONE', #5119, #10037, #14771 ) ;
#3303 = CARTESIAN_POINT ( 'NONE',  ( -55.42292740578360366, -3.330682475591782765, -0.6830477631804120486 ) ) ;
#3304 = CIRCLE ( 'NONE', #9890, 3.020710678118645909 ) ;
#3305 = CARTESIAN_POINT ( 'NONE',  ( -58.24005354137801049, -3.399999999999994138, 0.9110272542655853956 ) ) ;
#3306 = CARTESIAN_POINT ( 'NONE',  ( -58.44702994616205416, -2.078460969082659648, 3.599999999999782929 ) ) ;
#3307 = CARTESIAN_POINT ( 'NONE',  ( -36.22818246778668794, 0.6967302926296138343, 5.374298406428920316 ) ) ;
#3308 = CARTESIAN_POINT ( 'NONE',  ( 31.84510612492130122, 7.726745150394289219, 2.049999999999887468 ) ) ;
#3309 = ORIENTED_EDGE ( 'NONE', *, *, #7693, .F. ) ;
#3310 = FACE_OUTER_BOUND ( 'NONE', #19501, .T. ) ;
#3311 = EDGE_LOOP ( 'NONE', ( #22876, #22227, #28198, #5471, #29228, #20446, #8081, #17588 ) ) ;
#3312 = CYLINDRICAL_SURFACE ( 'NONE', #2957, 0.4500000000000001221 ) ;
#3314 = CARTESIAN_POINT ( 'NONE',  ( 58.74160516400043264, -1.258299259018153204, 1.390091577293904423 ) ) ;
#3313 = CARTESIAN_POINT ( 'NONE',  ( 15.41586008885044734, -3.272294129011796837, -4.050092634494051325 ) ) ;
#3315 = AXIS2_PLACEMENT_3D ( 'NONE', #5512, #20406, #10110 ) ;
#3316 = VERTEX_POINT ( 'NONE', #26311 ) ;
#3317 = CIRCLE ( 'NONE', #2815, 4.000000000000000000 ) ;
#3318 = VERTEX_POINT ( 'NONE', #11256 ) ;
#3319 = FACE_OUTER_BOUND ( 'NONE', #18096, .T. ) ;
#3320 = EDGE_CURVE ( 'NONE', #1882, #9827, #2230, .T. ) ;
#3321 = CIRCLE ( 'NONE', #4304, 0.1499999999999999667 ) ;
#3322 = CARTESIAN_POINT ( 'NONE',  ( 27.62808879389202588, 5.849836810644521989, 1.424999999999903011 ) ) ;
#3323 = EDGE_LOOP ( 'NONE', ( #11808, #25670, #7534, #21347 ) ) ;
#3325 = CARTESIAN_POINT ( 'NONE',  ( 51.25000000000001421, 1.100000000000537215, -1.196087371390568643 ) ) ;
#3324 = CARTESIAN_POINT ( 'NONE',  ( -56.88452994616205416, -3.117691453623976816, 1.799999999999785993 ) ) ;
#3326 = CARTESIAN_POINT ( 'NONE',  ( 52.20711756518982583, 0.7500000000005468959, -1.996089927833914146 ) ) ;
#3327 = AXIS2_PLACEMENT_3D ( 'NONE', #8358, #1086, #13252 ) ;
#3328 = CARTESIAN_POINT ( 'NONE',  ( -35.98994760229851408, -4.804073784580272566, -2.042134692980068333 ) ) ;
#3329 = APPLICATION_PROTOCOL_DEFINITION ( 'draft international standard', 'automotive_design', 1998, #12352 ) ;
#3330 = AXIS2_PLACEMENT_3D ( 'NONE', #8769, #23215, #6259 ) ;
#3331 = CARTESIAN_POINT ( 'NONE',  ( -59.29999999999998295, -2.410361377416136541, 2.431279660458814718 ) ) ;
#3332 =( BOUNDED_CURVE ( )  B_SPLINE_CURVE ( 2, ( #7629, #10156, #18939, #19824, #645, #29455, #29319, #12361, #12673 ),
 .UNSPECIFIED., .F., .T. ) 
 B_SPLINE_CURVE_WITH_KNOTS ( ( 3, 2, 2, 2, 3 ),
 ( 0.3611111111111111605, 0.3703703703703703498, 0.3888888888888888951, 0.4074074074074073848, 0.4166666666666666852 ),
 .UNSPECIFIED. ) 
 CURVE ( )  GEOMETRIC_REPRESENTATION_ITEM ( )  RATIONAL_B_SPLINE_CURVE ( ( 0.9330127018922194093, 0.9330127018922197424, 1.000000000000000000, 0.8660254037844387076, 1.000000000000000000, 0.8660254037844387076, 1.000000000000000000, 0.9330127018922191873, 0.9330127018922194093 ) ) 
 REPRESENTATION_ITEM ( '' )  );
#3333 = SURFACE_SIDE_STYLE ('',( #10618 ) ) ;
#3334 = PRESENTATION_LAYER_ASSIGNMENT (  '', '', ( #9426 ) ) ;
#3335 = ORIENTED_EDGE ( 'NONE', *, *, #15472, .F. ) ;
#3336 = EDGE_CURVE ( 'NONE', #7185, #19715, #17395, .T. ) ;
#3337 = CARTESIAN_POINT ( 'NONE',  ( -54.39999999999997726, -4.766731106216463600E-14, -1.831402436016377855E-13 ) ) ;
#3338 = CARTESIAN_POINT ( 'NONE',  ( 51.80000000000001137, 8.700707106781294442, -2.050000000000180123 ) ) ;
#3339 = CARTESIAN_POINT ( 'NONE',  ( 48.48122134030800368, -1.391940262981015586, -3.850000000000022293 ) ) ;
#3340 = CARTESIAN_POINT ( 'NONE',  ( 15.61033468494287746, -0.4841707035674406301, 5.391286593723129350 ) ) ;
#3341 = AXIS2_PLACEMENT_3D ( 'NONE', #22217, #9855, #5248 ) ;
#3342 = CIRCLE ( 'NONE', #15485, 0.1500000000000001887 ) ;
#3343 = CARTESIAN_POINT ( 'NONE',  ( -55.02900635094608361, 3.400000000000004352, 0.9110272542656342454 ) ) ;
#3344 = VECTOR ( 'NONE', #22872, 1000.000000000000000 ) ;
#3346 = CARTESIAN_POINT ( 'NONE',  ( 58.66118217212486741, -1.815481606354510724, -0.4689659288411509031 ) ) ;
#3345 = CARTESIAN_POINT ( 'NONE',  ( -35.85663232820584057, 5.086913985776147840, -1.171642053949061513 ) ) ;
#3347 = AXIS2_PLACEMENT_3D ( 'NONE', #20804, #18424, #27765 ) ;
#3348 = CARTESIAN_POINT ( 'NONE',  ( 58.75000000000002132, 6.153735859711025284E-13, 3.111507638930570854E-58 ) ) ;
#3349 = CARTESIAN_POINT ( 'NONE',  ( 52.07304482952998370, 3.932152442337120579, -2.045338529774464398 ) ) ;
#3350 = CIRCLE ( 'NONE', #20045, 1.000000000000000000 ) ;
#3352 = CARTESIAN_POINT ( 'NONE',  ( -59.67193011664021185, 2.054846984738300186, 1.719925937563907548 ) ) ;
#3351 = CARTESIAN_POINT ( 'NONE',  ( 50.50000000000002132, 5.291762632692320630E-13, 3.111507638930570854E-58 ) ) ;
#3353 = EDGE_LOOP ( 'NONE', ( #29832, #4972, #15380, #12265 ) ) ;
#3354 = CARTESIAN_POINT ( 'NONE',  ( 47.00000000000002132, -3.826179070414207573, 1.000000000000000222 ) ) ;
#3355 = AXIS2_PLACEMENT_3D ( 'NONE', #15910, #20841, #25418 ) ;
#3356 = DIRECTION ( 'NONE',  ( -1.000000000000000000, 0.000000000000000000, 0.000000000000000000 ) ) ;
#3357 = CARTESIAN_POINT ( 'NONE',  ( 16.10705563471230306, 3.051830235923028933, -4.466755975380259258 ) ) ;
#3358 = CARTESIAN_POINT ( 'NONE',  ( 57.05000000000001137, 0.7500000000000000000, 2.421260002560653213 ) ) ;
#3359 = ORIENTED_EDGE ( 'NONE', *, *, #29768, .T. ) ;
#3360 = CARTESIAN_POINT ( 'NONE',  ( 51.87416143049284045, 8.598705507415683513, 2.049999999999819522 ) ) ;
#3361 = DIRECTION ( 'NONE',  ( -1.000000000000000000, -3.053848253006669023E-16, 2.042510438544995415E-16 ) ) ;
#3362 = EDGE_CURVE ( 'NONE', #11262, #1256, #1313, .T. ) ;
#3363 = EDGE_LOOP ( 'NONE', ( #2146, #10642, #5548, #30651 ) ) ;
#3364 = TOROIDAL_SURFACE ( 'NONE', #18041, 4.600000000000000533, 0.4999999999999996669 ) ;
#3365 = CARTESIAN_POINT ( 'NONE',  ( 15.59055531549693896, -4.755763096844272120, 2.574151833883791873 ) ) ;
#3366 = EDGE_CURVE ( 'NONE', #10988, #5143, #15953, .T. ) ;
#3367 = ORIENTED_EDGE ( 'NONE', *, *, #18412, .F. ) ;
#3368 = AXIS2_PLACEMENT_3D ( 'NONE', #2691, #14860, #9679 ) ;
#3369 = CARTESIAN_POINT ( 'NONE',  ( 16.00221665700882667, 2.696520634775366076, -4.691964194339891314 ) ) ;
#3370 = DIRECTION ( 'NONE',  ( 0.000000000000000000, 0.000000000000000000, 1.000000000000000000 ) ) ;
#3371 = ORIENTED_EDGE ( 'NONE', *, *, #24152, .T. ) ;
#3372 = CIRCLE ( 'NONE', #19641, 0.4500000000000001221 ) ;
#3373 = DIRECTION ( 'NONE',  ( 1.000000000000000000, 9.742518634817235071E-17, 4.338815227941366087E-17 ) ) ;
#3374 = CARTESIAN_POINT ( 'NONE',  ( -61.13452994616202574, 2.093608279459375190E-14, -3.600000000000216804 ) ) ;
#3375 = ORIENTED_EDGE ( 'NONE', *, *, #24341, .T. ) ;
#3376 = CIRCLE ( 'NONE', #16531, 1.000000000000000000 ) ;
#3377 = CARTESIAN_POINT ( 'NONE',  ( 56.98303665332567647, 0.7553445069156616842, -1.743428900644034885 ) ) ;
#3378 = DIRECTION ( 'NONE',  ( 2.265029845352616032E-44, -1.000000000000000000, -3.491481338843140061E-15 ) ) ;
#3379 = AXIS2_PLACEMENT_3D ( 'NONE', #21214, #25929, #6046 ) ;
#3380 = CARTESIAN_POINT ( 'NONE',  ( 22.10122560051324569, 7.779108733371196571, 2.049999999999922551 ) ) ;
#3381 = ORIENTED_EDGE ( 'NONE', *, *, #30108, .T. ) ;
#3382 = VECTOR ( 'NONE', #15294, 1000.000000000000000 ) ;
#3383 = EDGE_CURVE ( 'NONE', #16857, #7964, #4085, .T. ) ;
#3384 = CARTESIAN_POINT ( 'NONE',  ( -58.56249999999997868, -1.962990915244731793, 3.399999999999783640 ) ) ;
#3385 = CIRCLE ( 'NONE', #26136, 0.2500000000000000000 ) ;
#3386 = CARTESIAN_POINT ( 'NONE',  ( 58.66122331388464772, 0.5173534011644945751, -1.802520131073004128 ) ) ;
#3387 = DIRECTION ( 'NONE',  ( 1.047444401652940007E-14, 0.000000000000000000, 1.000000000000000000 ) ) ;
#3388 = DIRECTION ( 'NONE',  ( 1.000000000000000000, 3.053848253006669023E-16, -2.042510438544995415E-16 ) ) ;
#3389 = CARTESIAN_POINT ( 'NONE',  ( 57.00059118976931671, -0.7088470050679284151, 2.446935707828179485 ) ) ;
#3391 = CARTESIAN_POINT ( 'NONE',  ( 51.50000000000002132, 1.163569835200988601E-28, -1.798112889504214751E-13 ) ) ;
#3390 = CARTESIAN_POINT ( 'NONE',  ( -54.49999999999999289, -1.400000000000007017, 3.959797974644449603 ) ) ;
#3392 = AXIS2_PLACEMENT_3D ( 'NONE', #1487, #24248, #4922 ) ;
#3393 = ADVANCED_FACE ( 'NONE', ( #2025 ), #30995, .T. ) ;
#3394 = AXIS2_PLACEMENT_3D ( 'NONE', #26527, #30818, #28442 ) ;
#3395 = CARTESIAN_POINT ( 'NONE',  ( 50.46999119548826940, -1.140870969100513888, -3.938727831757874664 ) ) ;
#3396 = CARTESIAN_POINT ( 'NONE',  ( -59.59999999999997300, 2.337126060168390307, -1.249136413240100607 ) ) ;
#3397 = CARTESIAN_POINT ( 'NONE',  ( -55.49999999999997868, -1.184343223768582698, -3.558065644182725418 ) ) ;
#3398 = CARTESIAN_POINT ( 'NONE',  ( 58.64999999999999858, 1.394635017529600951, -1.253243060177047452 ) ) ;
#3400 = CARTESIAN_POINT ( 'NONE',  ( 51.90000000000001279, -1.084202172485504434E-16, 4.374999999999999112 ) ) ;
#3399 = AXIS2_PLACEMENT_3D ( 'NONE', #25028, #25355, #821 ) ;
#3401 = ORIENTED_EDGE ( 'NONE', *, *, #5205, .T. ) ;
#3402 = B_SPLINE_CURVE_WITH_KNOTS ( 'NONE', 3,
 ( #976, #29934, #8243, #17908, #2207, #13912, #2059, #14088, #20913, #28348, #11721, #19185, #16316, #18858, #13754, #23608 ),
 .UNSPECIFIED., .F., .F.,
 ( 4, 3, 3, 3, 3, 4 ),
 ( 0.000000000000000000, 8.780272313934440255E-06, 2.643179650512019594E-05, 4.557815634108688274E-05, 6.564640436636450416E-05, 8.596378008536510913E-05 ),
 .UNSPECIFIED. ) ;
#3403 = DIRECTION ( 'NONE',  ( 0.000000000000000000, -0.8381322357052107819, 0.5454670984319629490 ) ) ;
#3404 = CIRCLE ( 'NONE', #21120, 0.05000000000000012768 ) ;
#3405 = ORIENTED_EDGE ( 'NONE', *, *, #17202, .T. ) ;
#3406 = VECTOR ( 'NONE', #5662, 1000.000000000000000 ) ;
#3407 = EDGE_CURVE ( 'NONE', #17261, #15970, #6471, .T. ) ;
#3408 = ORIENTED_EDGE ( 'NONE', *, *, #16789, .F. ) ;
#3409 = VECTOR ( 'NONE', #11236, 1000.000000000000000 ) ;
#3410 = CIRCLE ( 'NONE', #10509, 3.598079936076698182 ) ;
#3411 = DIRECTION ( 'NONE',  ( 3.384826294588897856E-15, 0.000000000000000000, 1.000000000000000000 ) ) ;
#3412 = CARTESIAN_POINT ( 'NONE',  ( -56.98542740578360366, -3.725040285533364859, 1.239922660687675204 ) ) ;
#3414 = CARTESIAN_POINT ( 'NONE',  ( 51.80000000000001847, -4.131056160354152240, 1.099999999999999867 ) ) ;
#3413 = CARTESIAN_POINT ( 'NONE',  ( -56.18749999999997158, -3.925981830489445379, -2.137374967025826226E-13 ) ) ;
#3415 = EDGE_CURVE ( 'NONE', #2006, #26664, #24196, .T. ) ;
#3416 = ORIENTED_EDGE ( 'NONE', *, *, #119, .T. ) ;
#3417 = ORIENTED_EDGE ( 'NONE', *, *, #15374, .T. ) ;
#3418 = CARTESIAN_POINT ( 'NONE',  ( -55.84585481156723574, -1.184343223768586029, -3.558065644182725862 ) ) ;
#3419 = VERTEX_POINT ( 'NONE', #14051 ) ;
#3420 = CARTESIAN_POINT ( 'NONE',  ( 51.74859327566192491, 3.850496488340269696, -1.443897952417738439 ) ) ;
#3421 = VERTEX_POINT ( 'NONE', #16433 ) ;
#3422 = CARTESIAN_POINT ( 'NONE',  ( 22.79271333219223550, 6.591595603790847413, -2.050000000000079758 ) ) ;
#3423 = CARTESIAN_POINT ( 'NONE',  ( 34.50000000000001421, 0.000000000000000000, 0.000000000000000000 ) ) ;
#3424 = TOROIDAL_SURFACE ( 'NONE', #29206, 1.375000000000001332, 0.2500000000000000000 ) ;
#3425 = CIRCLE ( 'NONE', #28180, 1.000000000000000000 ) ;
#3426 = EDGE_CURVE ( 'NONE', #17938, #27064, #28745, .T. ) ;
#3427 = CARTESIAN_POINT ( 'NONE',  ( -44.49999999999996447, -1.399999999999981037, -3.363870538531656518 ) ) ;
#3428 = CARTESIAN_POINT ( 'NONE',  ( -59.95655989232412963, 1.962990915244722245, 3.399999999999794742 ) ) ;
#3429 = CARTESIAN_POINT ( 'NONE',  ( 47.38487367463270061, -3.877460150898551561, 1.337636034593590484 ) ) ;
#3430 = CARTESIAN_POINT ( 'NONE',  ( 47.10000000000000853, -3.550773357292059007, -2.049880134335985815 ) ) ;
#3431 = AXIS2_PLACEMENT_3D ( 'NONE', #18805, #23390, #28448 ) ;
#3432 = FACE_OUTER_BOUND ( 'NONE', #1176, .T. ) ;
#3433 = CARTESIAN_POINT ( 'NONE',  ( 69.00000000000005684, 1.401298464324817071E-42, 3.949999999999278089 ) ) ;
#3435 = CARTESIAN_POINT ( 'NONE',  ( 51.30892234234251248, -4.380148595134231826, 1.408962902656405891 ) ) ;
#3434 = CARTESIAN_POINT ( 'NONE',  ( 47.00000000000002132, -3.726179070414207928, 1.100000000000000311 ) ) ;
#3436 = EDGE_CURVE ( 'NONE', #12157, #30563, #302, .T. ) ;
#3437 = CARTESIAN_POINT ( 'NONE',  ( 58.45000000000001705, -0.8000000000000000444, 2.421260002560649660 ) ) ;
#3438 = CARTESIAN_POINT ( 'NONE',  ( -35.85663232820584057, 1.123735532908288315, 5.289358697221541838 ) ) ;
#3439 = EDGE_LOOP ( 'NONE', ( #9222, #4212, #12728, #14863 ) ) ;
#3440 = AXIS2_PLACEMENT_3D ( 'NONE', #13751, #28344, #29282 ) ;
#3441 = AXIS2_PLACEMENT_3D ( 'NONE', #11042, #25912, #16112 ) ;
#3442 = CARTESIAN_POINT ( 'NONE',  ( 68.95000000000007390, 1.401298464324817071E-42, 3.949999999999278089 ) ) ;
#3443 = CARTESIAN_POINT ( 'NONE',  ( 54.22840347875643374, 6.361164334018160282, 2.049999999999810640 ) ) ;
#3444 = VERTEX_POINT ( 'NONE', #25614 ) ;
#3445 = EDGE_CURVE ( 'NONE', #29950, #14808, #22443, .T. ) ;
#3446 = CARTESIAN_POINT ( 'NONE',  ( -59.19999999999996732, -2.580747833305891970, -0.9498634748674686934 ) ) ;
#3447 = AXIS2_PLACEMENT_3D ( 'NONE', #29247, #7845, #5019 ) ;
#3448 = EDGE_LOOP ( 'NONE', ( #24740, #30646, #21922, #14424 ) ) ;
#3449 = EDGE_CURVE ( 'NONE', #11045, #19715, #20242, .T. ) ;
#3450 = CARTESIAN_POINT ( 'NONE',  ( 51.80000048029783244, 4.021162535479849254, 2.019963026417355589 ) ) ;
#3451 = B_SPLINE_CURVE_WITH_KNOTS ( 'NONE', 3,
 ( #10380, #27946, #25101, #20064, #896, #6261, #5639 ),
 .UNSPECIFIED., .F., .F.,
 ( 4, 3, 4 ),
 ( 0.000000000000000000, 3.139320973900864084E-05, 4.461998577547471821E-05 ),
 .UNSPECIFIED. ) ;
#3452 = CARTESIAN_POINT ( 'NONE',  ( -54.22085481156724285, 2.489203624310592833, -2.804704140674919799 ) ) ;
#3454 = DIRECTION ( 'NONE',  ( -0.000000000000000000, 0.9875000000000001554, -0.1576190026614806561 ) ) ;
#3453 = CYLINDRICAL_SURFACE ( 'NONE', #24127, 2.125000000000048850 ) ;
#3455 = EDGE_CURVE ( 'NONE', #12058, #12009, #19040, .T. ) ;
#3456 = ORIENTED_EDGE ( 'NONE', *, *, #21208, .T. ) ;
#3457 = CARTESIAN_POINT ( 'NONE',  ( 57.00000000000001421, -0.6999999999999999556, -1.820027472320129736 ) ) ;
#3458 = VERTEX_POINT ( 'NONE', #1545 ) ;
#3460 = DIRECTION ( 'NONE',  ( 0.000000000000000000, 0.000000000000000000, 1.000000000000000000 ) ) ;
#3459 = CARTESIAN_POINT ( 'NONE',  ( -44.49999999999999289, -1.400000000000004574, 3.363870538531273269 ) ) ;
#3461 = CYLINDRICAL_SURFACE ( 'NONE', #23554, 0.1000000000000000472 ) ;
#3462 = ORIENTED_EDGE ( 'NONE', *, *, #9789, .T. ) ;
#3463 = FACE_OUTER_BOUND ( 'NONE', #23795, .T. ) ;
#3464 = CARTESIAN_POINT ( 'NONE',  ( 58.75000000000000711, 1.652371589363942794, -1.066009655021259883 ) ) ;
#3465 = CARTESIAN_POINT ( 'NONE',  ( -61.58692253671846828, -2.595286993531995545, -0.5015316826422865359 ) ) ;
#3466 = CARTESIAN_POINT ( 'NONE',  ( 51.78364358464227024, -0.9002346248696042608, 1.360127766454835685 ) ) ;
#3467 = CIRCLE ( 'NONE', #25191, 0.1000000000000000472 ) ;
#3468 = ORIENTED_EDGE ( 'NONE', *, *, #15966, .T. ) ;
#3469 = PRESENTATION_LAYER_ASSIGNMENT (  '', '', ( #21708 ) ) ;
#3470 = EDGE_CURVE ( 'NONE', #11984, #12035, #23081, .T. ) ;
#3471 = CARTESIAN_POINT ( 'NONE',  ( -60.62155403265821718, -2.510184553012070552, 0.9710796741145765187 ) ) ;
#3473 = EDGE_CURVE ( 'NONE', #9481, #8076, #3850, .T. ) ;
#3472 = DIRECTION ( 'NONE',  ( 0.000000000000000000, 0.000000000000000000, -1.000000000000000000 ) ) ;
#3474 = CARTESIAN_POINT ( 'NONE',  ( -57.25952994616203995, 3.117691453623998576, -1.800000000000181899 ) ) ;
#3475 = CARTESIAN_POINT ( 'NONE',  ( 58.72204580543430552, -1.874996463825583826, 0.02257357450724356909 ) ) ;
#3476 = CARTESIAN_POINT ( 'NONE',  ( 22.07280086217095061, 8.086143481909148889, 2.049999999999922995 ) ) ;
#3477 = ORIENTED_EDGE ( 'NONE', *, *, #7992, .F. ) ;
#3478 = DIRECTION ( 'NONE',  ( -1.000000000000000000, -3.053848253006669023E-16, 2.042510438544995415E-16 ) ) ;
#3479 = ORIENTED_EDGE ( 'NONE', *, *, #29405, .F. ) ;
#3480 = UNCERTAINTY_MEASURE_WITH_UNIT (LENGTH_MEASURE( 1.000000000000000082E-05 ), #21645, 'distance_accuracy_value', 'NONE');
#3482 = CARTESIAN_POINT ( 'NONE',  ( 61.25000000000002132, 6.415596960124259844E-13, 3.111507638930570854E-58 ) ) ;
#3481 = DIRECTION ( 'NONE',  ( 0.000000000000000000, 1.000000000000000000, 3.491481338843130594E-15 ) ) ;
#3483 = ADVANCED_FACE ( 'NONE', ( #18351 ), #13401, .F. ) ;
#3484 = ORIENTED_EDGE ( 'NONE', *, *, #14885, .T. ) ;
#3485 = ORIENTED_EDGE ( 'NONE', *, *, #29057, .T. ) ;
#3486 = DIRECTION ( 'NONE',  ( 0.000000000000000000, 0.000000000000000000, 1.000000000000000000 ) ) ;
#3487 =( GEOMETRIC_REPRESENTATION_CONTEXT ( 3 ) GLOBAL_UNCERTAINTY_ASSIGNED_CONTEXT ( ( #19948 ) ) GLOBAL_UNIT_ASSIGNED_CONTEXT ( ( #5741, #3205, #13168 ) ) REPRESENTATION_CONTEXT ( 'NONE', 'WORKASPACE' ) );
#3488 = CIRCLE ( 'NONE', #9586, 3.675000000000029132 ) ;
#3489 = DIRECTION ( 'NONE',  ( -1.163827112947670229E-15, 0.9428090415820664649, 0.3333333333333248771 ) ) ;
#3490 = VERTEX_POINT ( 'NONE', #11208 ) ;
#3492 = CARTESIAN_POINT ( 'NONE',  ( 58.75000000000000711, 1.022750809560622143, 1.571497941947222365 ) ) ;
#3491 = CARTESIAN_POINT ( 'NONE',  ( -59.82202994616204705, -4.156921938165296204, -2.272478542645976661E-13 ) ) ;
#3493 =( BOUNDED_CURVE ( )  B_SPLINE_CURVE ( 2, ( #6525, #27899, #25515, #8722, #25834, #20939, #30569, #23169, #8880, #13472, #28220, #16185, #8578, #1453, #4141, #13778, #23461, #11111, #11423, #18728, #21113, #30751, #8427, #6067, #15720, #3673, #13309, #23001, #10956, #20644, #18260, #15499, #20422, #25311, #30047, #27690, #19943, #15183, #24685, #10893, #20272, #5840, #8212, #17880, #18206, #25156, #3474, #22944, #29902, #8362, #12956, #27371, #15024, #12791, #22471, #17730, #20582, #13114, #12641, #18044, #3621, #10740, #30217, #7897, #6009, #3306, #27515, #5682, #22649, #22803, #8064, #15663, #29578, #945, #15332, #24981, #8524, #10595, #1090, #17573, #5531, #5363, #3150 ),
 .UNSPECIFIED., .F., .T. ) 
 B_SPLINE_CURVE_WITH_KNOTS ( ( 3, 2, 2, 2, 2, 2, 2, 2, 2, 2, 2, 2, 2, 2, 2, 2, 2, 2, 2, 2, 2, 2, 2, 2, 2, 2, 2, 2, 2, 2, 2, 2, 2, 2, 2, 2, 2, 2, 2, 2, 2, 3 ),
 ( 0.01191687898796012397, 0.01851851851851851749, 0.03703703703703703498, 0.05555555555555555941, 0.07407407407407406996, 0.09259259259259258745, 0.1111111111111111049, 0.1296296296296296224, 0.1481481481481481399, 0.1666666666666666574, 0.1851851851851851749, 0.2037037037037037202, 0.2222222222222222099, 0.2407407407407407274, 0.2592592592592593004, 0.2777777777777777901, 0.2962962962962962798, 0.3148148148148148251, 0.3333333333333333148, 0.3518518518518518601, 0.3703703703703703498, 0.3888888888888888951, 0.4074074074074073293, 0.4259259259259259855, 0.4444444444444444198, 0.4629629629629629650, 0.4814814814814814548, 0.5000000000000000000, 0.5185185185185184897, 0.5370370370370370905, 0.5555555555555555802, 0.5740740740740740700, 0.5925925925925925597, 0.6111111111111111605, 0.6296296296296296502, 0.6481481481481481399, 0.6666666666666666297, 0.6851851851851852304, 0.7037037037037037202, 0.7222222222222220989, 0.7407407407407408106, 0.7438073466758352570 ),
 .UNSPECIFIED. ) 
 CURVE ( )  GEOMETRIC_REPRESENTATION_ITEM ( )  RATIONAL_B_SPLINE_CURVE ( ( 0.9385312603869460091, 0.9522395925147686402, 1.000000000000000000, 0.8660254037844387076, 1.000000000000000000, 0.8660254037844387076, 1.000000000000000000, 0.8660254037844387076, 1.000000000000000000, 0.8660254037844387076, 1.000000000000000000, 0.8660254037844387076, 1.000000000000000000, 0.8660254037844387076, 1.000000000000000000, 0.8660254037844387076, 1.000000000000000000, 0.8660254037844387076, 1.000000000000000000, 0.8660254037844387076, 1.000000000000000000, 0.8660254037844387076, 1.000000000000000000, 0.8660254037844387076, 1.000000000000000000, 0.8660254037844387076, 1.000000000000000000, 0.8660254037844387076, 1.000000000000000000, 0.8660254037844387076, 1.000000000000000000, 0.8660254037844387076, 1.000000000000000000, 0.8660254037844387076, 1.000000000000000000, 0.8660254037844387076, 1.000000000000000000, 0.8660254037844387076, 1.000000000000000000, 0.8660254037844387076, 1.000000000000000000, 0.8660254037844387076, 1.000000000000000000, 0.8660254037844387076, 1.000000000000000000, 0.8660254037844387076, 1.000000000000000000, 0.8660254037844387076, 1.000000000000000000, 0.8660254037844387076, 1.000000000000000000, 0.8660254037844387076, 1.000000000000000000, 0.8660254037844387076, 1.000000000000000000, 0.8660254037844387076, 1.000000000000000000, 0.8660254037844387076, 1.000000000000000000, 0.8660254037844387076, 1.000000000000000000, 0.8660254037844387076, 1.000000000000000000, 0.8660254037844387076, 1.000000000000000000, 0.8660254037844387076, 1.000000000000000000, 0.8660254037844387076, 1.000000000000000000, 0.8660254037844387076, 1.000000000000000000, 0.8660254037844387076, 1.000000000000000000, 0.8660254037844387076, 1.000000000000000000, 0.8660254037844387076, 1.000000000000000000, 0.8660254037844387076, 1.000000000000000000, 0.8660254037844387076, 1.000000000000000000, 0.9778142462370478238, 0.9629762686038090269 ) ) 
 REPRESENTATION_ITEM ( '' )  );
#3494 = CARTESIAN_POINT ( 'NONE',  ( -56.11042740578360366, -2.936324665650200672, -2.606018187048498191 ) ) ;
#3495 = CARTESIAN_POINT ( 'NONE',  ( 51.90000000000001279, -4.227689052994015206, 1.125730994152046582 ) ) ;
#3496 = CARTESIAN_POINT ( 'NONE',  ( 0.000000000000000000, 0.000000000000000000, 0.000000000000000000 ) ) ;
#3497 = CARTESIAN_POINT ( 'NONE',  ( 53.81457038983117513, 5.799118250651475570, -1.689328355159275041 ) ) ;
#3498 = ORIENTED_EDGE ( 'NONE', *, *, #15692, .T. ) ;
#3499 = CARTESIAN_POINT ( 'NONE',  ( -60.32202994616201863, 2.078460969082674747, -3.600000000000205258 ) ) ;
#3500 = CARTESIAN_POINT ( 'NONE',  ( 53.89553379148907197, 6.017104844469305824, -1.708828125785526675 ) ) ;
#3501 = FACE_OUTER_BOUND ( 'NONE', #19557, .T. ) ;
#3502 = CARTESIAN_POINT ( 'NONE',  ( 15.67083574136752233, 0.3995010896672199774, 5.397102918580290343 ) ) ;
#3503 = EDGE_CURVE ( 'NONE', #26503, #9408, #20882, .T. ) ;
#3504 = PRODUCT_DEFINITION_FORMATION_WITH_SPECIFIED_SOURCE ( 'ANY', '', #16726, .NOT_KNOWN. ) ;
#3505 = EDGE_CURVE ( 'NONE', #3662, #19199, #24031, .T. ) ;
#3506 = DIRECTION ( 'NONE',  ( 1.000000000000000000, 0.000000000000000000, -1.047444401652940007E-14 ) ) ;
#3507 = CIRCLE ( 'NONE', #16677, 0.09999999999999983902 ) ;
#3509 = EDGE_CURVE ( 'NONE', #20749, #22845, #219, .T. ) ;
#3508 = FACE_OUTER_BOUND ( 'NONE', #29871, .T. ) ;
#3510 = DIRECTION ( 'NONE',  ( 0.000000000000000000, 0.000000000000000000, 1.000000000000000000 ) ) ;
#3511 = CARTESIAN_POINT ( 'NONE',  ( -60.59999999999998010, -2.408745774756101188, -1.060314564156378037 ) ) ;
#3513 = DIRECTION ( 'NONE',  ( -1.000000000000000000, 1.219044193948983948E-29, -3.491481338843133355E-15 ) ) ;
#3512 = CARTESIAN_POINT ( 'NONE',  ( 58.75000000000002132, -0.4999999999991823207, -1.863080903343696137 ) ) ;
#3514 = ORIENTED_EDGE ( 'NONE', *, *, #2244, .F. ) ;
#3515 = CARTESIAN_POINT ( 'NONE',  ( 50.40741710815419196, -1.342093792059618762, -3.874237195466570416 ) ) ;
#3516 = CARTESIAN_POINT ( 'NONE',  ( 36.50000000000002132, 0.000000000000000000, 0.000000000000000000 ) ) ;
#3518 = CARTESIAN_POINT ( 'NONE',  ( 51.80000000000001847, 2.428612866367529932E-14, -1.808587333520743709E-13 ) ) ;
#3517 = FACE_OUTER_BOUND ( 'NONE', #4297, .T. ) ;
#3519 = CARTESIAN_POINT ( 'NONE',  ( -54.44999999999997442, -1.500000000000000222, -3.300094695611020867 ) ) ;
#3520 = ORIENTED_EDGE ( 'NONE', *, *, #566, .T. ) ;
#3521 = CARTESIAN_POINT ( 'NONE',  ( 52.48739568812350598, 8.621481665389278959, 2.049999999999817302 ) ) ;
#3522 = DIRECTION ( 'NONE',  ( 1.168655815394902336E-14, 0.000000000000000000, 1.000000000000000000 ) ) ;
#3523 = EDGE_CURVE ( 'NONE', #27109, #7871, #8782, .T. ) ;
#3524 =( BOUNDED_CURVE ( )  B_SPLINE_CURVE ( 3, ( #10140, #17268, #321, #9689 ),
 .UNSPECIFIED., .F., .T. ) 
 B_SPLINE_CURVE_WITH_KNOTS ( ( 4, 4 ),
 ( 1.982313172862383510, 2.241731514487931065 ),
 .UNSPECIFIED. ) 
 CURVE ( )  GEOMETRIC_REPRESENTATION_ITEM ( )  RATIONAL_B_SPLINE_CURVE ( ( 1.000000000000000000, 0.9943997021150918769, 0.9943997021150918769, 1.000000000000000000 ) ) 
 REPRESENTATION_ITEM ( '' )  );
#3525 = VECTOR ( 'NONE', #13585, 1000.000000000000000 ) ;
#3526 = EDGE_LOOP ( 'NONE', ( #19588, #28740, #24, #29141 ) ) ;
#3527 = DIRECTION ( 'NONE',  ( 0.000000000000000000, 0.000000000000000000, 1.000000000000000000 ) ) ;
#3528 = EDGE_LOOP ( 'NONE', ( #415, #8028, #2607, #19594 ) ) ;
#3529 = B_SPLINE_CURVE_WITH_KNOTS ( 'NONE', 3,
 ( #28835, #26448, #17738, #27523, #15192, #1240, #5689, #15339, #25463, #29755 ),
 .UNSPECIFIED., .F., .F.,
 ( 4, 2, 2, 2, 4 ),
 ( 0.000000000000000000, 0.0004363777631660871827, 0.0006545666447491323191, 0.0007636610855406580044, 0.0008727555263321836896 ),
 .UNSPECIFIED. ) ;
#3530 = DIRECTION ( 'NONE',  ( -3.198643159535995633E-15, -0.9356455129756995337, -0.3529411764705844834 ) ) ;
#3531 = DIRECTION ( 'NONE',  ( 1.000000000000000000, 0.000000000000000000, -1.047444401652940007E-14 ) ) ;
#3532 = VERTEX_POINT ( 'NONE', #19444 ) ;
#3533 = CARTESIAN_POINT ( 'NONE',  ( 33.39017613691037667, 8.099518147537066781, 1.949999999999883382 ) ) ;
#3534 = CIRCLE ( 'NONE', #29310, 0.09999999999999986677 ) ;
#3535 = CARTESIAN_POINT ( 'NONE',  ( -59.82202994616204705, -4.156921938165296204, -2.272478542645976661E-13 ) ) ;
#3536 = VECTOR ( 'NONE', #28101, 1000.000000000000000 ) ;
#3537 = ORIENTED_EDGE ( 'NONE', *, *, #6553, .T. ) ;
#3538 = DIRECTION ( 'NONE',  ( -1.000000000000000000, -0.000000000000000000, -0.000000000000000000 ) ) ;
#3539 = ORIENTED_EDGE ( 'NONE', *, *, #159, .F. ) ;
#3540 = TOROIDAL_SURFACE ( 'NONE', #21756, 0.2600000000000000089, 0.01000000000000000021 ) ;
#3541 = CARTESIAN_POINT ( 'NONE',  ( -57.81249999999998579, -1.962990915244731793, 3.399999999999786304 ) ) ;
#3542 = CARTESIAN_POINT ( 'NONE',  ( -62.09999999999997300, 1.168016602258162478E-15, 2.197726754101795588E-15 ) ) ;
#3543 = DIRECTION ( 'NONE',  ( 1.000000000000000000, 0.000000000000000000, -8.673617379884989994E-15 ) ) ;
#3544 = PLANE ( 'NONE',  #8895 ) ;
#3545 = CARTESIAN_POINT ( 'NONE',  ( -59.29999999999997584, 0.7533615035078071731, -3.673546848079177529 ) ) ;
#3546 = EDGE_CURVE ( 'NONE', #3048, #28401, #4252, .T. ) ;
#3548 = CARTESIAN_POINT ( 'NONE',  ( 49.05000000000002558, 1.401298464324817071E-42, -5.137714790107672405E-13 ) ) ;
#3547 = DIRECTION ( 'NONE',  ( 1.000000000000000000, 0.000000000000000000, -3.491481338843133355E-15 ) ) ;
#3549 = CARTESIAN_POINT ( 'NONE',  ( -73.89999999999997726, -2.435524336289708093E-15, 4.607889071584891164E-15 ) ) ;
#3550 = CARTESIAN_POINT ( 'NONE',  ( -59.62735476476905205, 2.346806195053369848, -1.237686616523536287 ) ) ;
#3551 = CARTESIAN_POINT ( 'NONE',  ( -55.47099364905386665, -0.2309624077929001984, -3.875409454552789956 ) ) ;
#3552 = CARTESIAN_POINT ( 'NONE',  ( 58.75000000000000711, 1.394635017529601617, -1.253243060177046564 ) ) ;
#3553 = LINE ( 'NONE', #30130, #21611 ) ;
#3554 = CIRCLE ( 'NONE', #1024, 2.000000000000000000 ) ;
#3555 = VERTEX_POINT ( 'NONE', #9779 ) ;
#3556 = CARTESIAN_POINT ( 'NONE',  ( 50.46953806735880477, -1.143620537822792826, 3.937943076466138059 ) ) ;
#3557 = CARTESIAN_POINT ( 'NONE',  ( -36.81959771849335539, 0.5763363385013660078, -5.380853831843024793 ) ) ;
#3558 = TOROIDAL_SURFACE ( 'NONE', #21783, 1.850000000000000089, 0.05000000000000000278 ) ;
#3559 = ORIENTED_EDGE ( 'NONE', *, *, #15795, .T. ) ;
#3561 = EDGE_CURVE ( 'NONE', #4172, #28052, #431, .T. ) ;
#3560 = B_SPLINE_CURVE_WITH_KNOTS ( 'NONE', 3,
 ( #26754, #15323, #27033, #5518, #15009, #29277, #5344, #10419, #20101, #29736, #2677, #29563, #17104, #5197, #5053, #14707, #8051, #9963 ),
 .UNSPECIFIED., .F., .F.,
 ( 4, 2, 2, 2, 2, 2, 2, 2, 4 ),
 ( 0.000000000000000000, 0.0007653146945936880252, 0.001530629389187376050, 0.002295944083781063967, 0.003061258778374752101, 0.003826573472968439801, 0.004591888167562127067, 0.005357202862155815634, 0.006122517556749502467 ),
 .UNSPECIFIED. ) ;
#3562 = ORIENTED_EDGE ( 'NONE', *, *, #16812, .F. ) ;
#3563 = LINE ( 'NONE', #19876, #12364 ) ;
#3564 = DIRECTION ( 'NONE',  ( 3.491481338843133355E-15, -0.000000000000000000, 1.000000000000000000 ) ) ;
#3566 = CARTESIAN_POINT ( 'NONE',  ( -59.49223166990491762, 2.264560344927355917, 1.390271221205179986 ) ) ;
#3565 = CARTESIAN_POINT ( 'NONE',  ( -58.62499999999998579, -3.920666489018310435E-15, 3.399999999999791189 ) ) ;
#3567 = VERTEX_POINT ( 'NONE', #26866 ) ;
#3568 = VERTEX_POINT ( 'NONE', #19300 ) ;
#3569 = CARTESIAN_POINT ( 'NONE',  ( 58.64999999999999858, 1.877732920581272058, 0.6121634413844395661 ) ) ;
#3570 = ORIENTED_EDGE ( 'NONE', *, *, #10028, .T. ) ;
#3571 = CARTESIAN_POINT ( 'NONE',  ( -59.19999999999996732, 2.580747833305914618, -0.9498634748674507078 ) ) ;
#3572 = VERTEX_POINT ( 'NONE', #6946 ) ;
#3573 = CARTESIAN_POINT ( 'NONE',  ( 60.81468257897371643, 0.5000000000006363798, 1.863080903344385586 ) ) ;
#3574 = CARTESIAN_POINT ( 'NONE',  ( -61.82615520548803545, -2.629528139897267192, 0.2842755848553404352 ) ) ;
#3575 = CARTESIAN_POINT ( 'NONE',  ( -59.18749999999995737, -3.399999999999991029, -2.288065396424332102E-13 ) ) ;
#3576 = DIRECTION ( 'NONE',  ( -1.000000000000000000, -2.586136946169074517E-16, 0.000000000000000000 ) ) ;
#3577 = CARTESIAN_POINT ( 'NONE',  ( -58.20655989232411542, -3.925981830489445379, -2.207870066386390016E-13 ) ) ;
#3578 = CARTESIAN_POINT ( 'NONE',  ( -57.78335481156722864, 3.238593381231847257, 2.874284765127023356 ) ) ;
#3579 = CARTESIAN_POINT ( 'NONE',  ( 58.65000038048046349, 1.383507098107668476, 1.265626441016067805 ) ) ;
#3580 = AXIS2_PLACEMENT_3D ( 'NONE', #9514, #2367, #14708 ) ;
#3581 = EDGE_CURVE ( 'NONE', #25173, #20006, #30037, .T. ) ;
#3582 = CARTESIAN_POINT ( 'NONE',  ( -44.49999999999997868, 0.7497673985144576170, 0.01867747640535713169 ) ) ;
#3584 = DIRECTION ( 'NONE',  ( 1.000000000000000000, 1.047444401652940007E-14, -0.000000000000000000 ) ) ;
#3583 = CARTESIAN_POINT ( 'NONE',  ( -57.22499999999997300, 0.9241234443029104906, -4.506217466977124886 ) ) ;
#3585 = CARTESIAN_POINT ( 'NONE',  ( -57.77499999999997016, 2.796048871338436190E-15, 1.138853883557972617E-16 ) ) ;
#3586 = CARTESIAN_POINT ( 'NONE',  ( -60.49999999999995737, -0.7328781032566554776, 3.573665542649864246 ) ) ;
#3587 = FACE_OUTER_BOUND ( 'NONE', #26256, .T. ) ;
#3588 = EDGE_LOOP ( 'NONE', ( #25622, #30153, #8301, #3200 ) ) ;
#3589 = CARTESIAN_POINT ( 'NONE',  ( 54.29903166994490959, 6.002871265136678680, 2.049999999999811529 ) ) ;
#3590 = ORIENTED_EDGE ( 'NONE', *, *, #9432, .T. ) ;
#3591 = EDGE_CURVE ( 'NONE', #17195, #20006, #12005, .T. ) ;
#3592 = CARTESIAN_POINT ( 'NONE',  ( 51.69999999178978101, -3.608818513796484773, 1.949335135736226299 ) ) ;
#3593 = ORIENTED_EDGE ( 'NONE', *, *, #14187, .T. ) ;
#3594 = FACE_OUTER_BOUND ( 'NONE', #30267, .T. ) ;
#3595 = CYLINDRICAL_SURFACE ( 'NONE', #8231, 0.1500000000000001887 ) ;
#3597 = DIRECTION ( 'NONE',  ( -2.614375865348240525E-16, 0.2008964009354147762, -0.9796124928211140670 ) ) ;
#3596 = CARTESIAN_POINT ( 'NONE',  ( 51.80000000000001137, 4.175664755576646847, -1.929721184274108436 ) ) ;
#3598 = VERTEX_POINT ( 'NONE', #24198 ) ;
#3599 = CARTESIAN_POINT ( 'NONE',  ( -61.39999999999998437, -2.565822298769830478, -0.8405688140393350327 ) ) ;
#3600 = CARTESIAN_POINT ( 'NONE',  ( 57.04540039768303217, -0.7500000000000000000, -1.778341924377873751 ) ) ;
#3601 = VERTEX_POINT ( 'NONE', #28936 ) ;
#3603 = SPHERICAL_SURFACE ( 'NONE', #30210, 0.05000000000000000278 ) ;
#3602 = FACE_OUTER_BOUND ( 'NONE', #13881, .T. ) ;
#3604 = DIRECTION ( 'NONE',  ( -0.9993908270190956511, 0.03489949670250096919, 3.491481338843132961E-15 ) ) ;
#3605 = EDGE_LOOP ( 'NONE', ( #28850, #1164, #16168, #20608, #16024, #7000, #4024, #15605, #10838, #27110, #3468, #15958, #18199, #1781, #6627, #26607, #3570, #20339, #27784, #23267, #6999, #2962, #26412, #22336, #26949, #4513, #20403, #28216, #3090, #10562 ) ) ;
#3606 = DIRECTION ( 'NONE',  ( 1.000000000000000000, 3.053848253006669023E-16, -2.042510438544995415E-16 ) ) ;
#3607 = ADVANCED_FACE ( 'NONE', ( #24484 ), #22978, .T. ) ;
#3608 = CARTESIAN_POINT ( 'NONE',  ( 58.75000000000000711, 1.655311165517640459, -1.077297519404307957 ) ) ;
#3609 = CARTESIAN_POINT ( 'NONE',  ( -36.40793637698146057, -3.917775493694432676, 3.727542820438226379 ) ) ;
#3610 = DIRECTION ( 'NONE',  ( 1.000000000000000000, -1.805490781531896312E-17, 1.716160222047132579E-16 ) ) ;
#3611 = CARTESIAN_POINT ( 'NONE',  ( 51.89360908398616345, -0.6611756245529596399, 1.497563819582714340 ) ) ;
#3612 = VERTEX_POINT ( 'NONE', #2504 ) ;
#3613 = AXIS2_PLACEMENT_3D ( 'NONE', #12614, #27820, #22444 ) ;
#3614 = CIRCLE ( 'NONE', #25350, 2.750000000000000000 ) ;
#3615 = EDGE_CURVE ( 'NONE', #11521, #24734, #17914, .T. ) ;
#3616 = CARTESIAN_POINT ( 'NONE',  ( 16.07512358269928399, 3.430438802933705400, 4.182416543699213562 ) ) ;
#3617 = EDGE_CURVE ( 'NONE', #10094, #29651, #30529, .T. ) ;
#3618 = ADVANCED_FACE ( 'NONE', ( #26554 ), #5059, .T. ) ;
#3619 = DIRECTION ( 'NONE',  ( 0.000000000000000000, 1.000000000000000000, 0.000000000000000000 ) ) ;
#3620 = CARTESIAN_POINT ( 'NONE',  ( -58.26905989232412253, -2.944486372867094914, 1.699999999999771472 ) ) ;
#3621 = CARTESIAN_POINT ( 'NONE',  ( -58.13452994616202574, 3.813458051520598461E-14, -3.600000000000206146 ) ) ;
#3622 = CARTESIAN_POINT ( 'NONE',  ( 58.74160516400041843, -1.872695119588361212, 0.09319124196129820181 ) ) ;
#3623 = CARTESIAN_POINT ( 'NONE',  ( 48.50000000000354561, 1.426739617988885822, -3.843749999997122746 ) ) ;
#3624 = ORIENTED_EDGE ( 'NONE', *, *, #18111, .F. ) ;
#3625 = AXIS2_PLACEMENT_3D ( 'NONE', #24149, #3221, #27759 ) ;
#3626 = DIRECTION ( 'NONE',  ( 0.000000000000000000, -1.000000000000000000, 0.000000000000000000 ) ) ;
#3627 = VERTEX_POINT ( 'NONE', #2340 ) ;
#3628 = CARTESIAN_POINT ( 'NONE',  ( -59.11195455104547136, 2.468319916663101576, -0.9648999906351578559 ) ) ;
#3629 = FACE_OUTER_BOUND ( 'NONE', #22604, .T. ) ;
#3630 = ORIENTED_EDGE ( 'NONE', *, *, #23122, .F. ) ;
#3631 = VERTEX_POINT ( 'NONE', #19614 ) ;
#3632 = CARTESIAN_POINT ( 'NONE',  ( 47.00000000000002132, 2.264383216608037083E-15, -4.275000000000000355 ) ) ;
#3633 = AXIS2_PLACEMENT_3D ( 'NONE', #8691, #3956, #30242 ) ;
#3634 = LINE ( 'NONE', #18223, #6547 ) ;
#3636 = DIRECTION ( 'NONE',  ( -0.9993908270190957621, 0.03489949670250106634, 3.490838185622846777E-15 ) ) ;
#3635 = DIRECTION ( 'NONE',  ( -1.000000000000000000, 1.219044193948983948E-29, -3.491481338843133355E-15 ) ) ;
#3637 = CARTESIAN_POINT ( 'NONE',  ( -59.61042740578360366, 3.725040285533370632, -1.239922660687675204 ) ) ;
#3638 = EDGE_CURVE ( 'NONE', #4925, #7153, #27006, .T. ) ;
#3639 = CARTESIAN_POINT ( 'NONE',  ( -71.44999999999998863, -0.3062499654112579295, 1.493338310920507839 ) ) ;
#3640 = CARTESIAN_POINT ( 'NONE',  ( -59.39944685111014877, 2.372743686651884953, 1.252203205371202666 ) ) ;
#3641 = EDGE_CURVE ( 'NONE', #4765, #17711, #21687, .T. ) ;
#3642 = ORIENTED_EDGE ( 'NONE', *, *, #566, .F. ) ;
#3643 = CARTESIAN_POINT ( 'NONE',  ( -60.25952994616203284, 3.117691453623994580, -1.800000000000200329 ) ) ;
#3644 = CARTESIAN_POINT ( 'NONE',  ( 53.25508263676793064, 8.249290793645352338, -2.050000000000185452 ) ) ;
#3645 = DIRECTION ( 'NONE',  ( 1.000000000000000000, 1.047444401652940007E-14, 0.000000000000000000 ) ) ;
#3646 = DIRECTION ( 'NONE',  ( 0.000000000000000000, 0.9996898646859344595, 0.02490330187381124480 ) ) ;
#3647 = EDGE_CURVE ( 'NONE', #8649, #19299, #20456, .T. ) ;
#3648 = CARTESIAN_POINT ( 'NONE',  ( -54.39999999999996305, -1.433333333333312254, -4.054078878803088593 ) ) ;
#3650 = CARTESIAN_POINT ( 'NONE',  ( 58.65000000000004121, -1.834410884275005094, -0.3880228184670952429 ) ) ;
#3649 = DIRECTION ( 'NONE',  ( 1.000000000000000000, 1.047444401652940007E-14, 0.000000000000000000 ) ) ;
#3651 = DIRECTION ( 'NONE',  ( 1.000000000000000000, -0.000000000000000000, -1.047444401652940007E-14 ) ) ;
#3652 = LINE ( 'NONE', #10480, #21571 ) ;
#3654 = CARTESIAN_POINT ( 'NONE',  ( -44.59999999999997300, -4.766731106216475591E-14, -1.489237264809750408E-13 ) ) ;
#3653 = CARTESIAN_POINT ( 'NONE',  ( -35.85663232820584767, 3.817150320980521983, -2.203324261490877678 ) ) ;
#3655 = EDGE_LOOP ( 'NONE', ( #7297, #5658, #2596, #6910 ) ) ;
#3656 = CARTESIAN_POINT ( 'NONE',  ( 50.37844020491943553, -1.181909706220196643, -3.885998080850099790 ) ) ;
#3657 =( BOUNDED_SURFACE ( )  B_SPLINE_SURFACE ( 3, 2, ( 
 ( #14406, #26451, #31038 ),
 ( #9360, #28513, #11735 ),
 ( #18870, #9537, #30736 ),
 ( #6816, #16481, #21731 ),
 ( #28683, #9043, #16327 ),
 ( #21262, #28836, #18717 ),
 ( #26140, #16810, #19197 ),
 ( #4278, #6997, #28360 ),
 ( #12055, #11884, #4128 ),
 ( #4449, #11408, #16659 ),
 ( #19025, #26300, #6665 ),
 ( #28980, #14099, #21099 ),
 ( #4601, #14258, #23928 ),
 ( #7147, #9209, #24078 ),
 ( #1738, #2392, #22 ),
 ( #25820, #9684, #30893 ) ),
 .UNSPECIFIED., .F., .F., .T. ) 
 B_SPLINE_SURFACE_WITH_KNOTS ( ( 4, 2, 2, 2, 2, 2, 2, 4 ),
 ( 3, 3 ),
 ( 0.001780502285214233737, 0.002558945925323762895, 0.002753556835351145347, 0.002948167745378527799, 0.003337389565433292269, 0.003726611385488056739, 0.004115833205542821643, 0.004894276845652350584 ),
 ( 0.000000000000000000, 1.000000000000000000 ),
 .UNSPECIFIED. ) 
 GEOMETRIC_REPRESENTATION_ITEM ( )  RATIONAL_B_SPLINE_SURFACE ( (
 ( 1.000000000000000000, 0.9418517008537257151, 1.000000000000000000),
 ( 1.000000000000000000, 0.9417987965884543344, 1.000000000000000000),
 ( 1.000000000000000000, 0.9418198861734828897, 1.000000000000000000),
 ( 1.000000000000000000, 0.9434060303845416273, 1.000000000000000000),
 ( 1.000000000000000000, 0.9437939819948035769, 1.000000000000000000),
 ( 1.000000000000000000, 0.9445989566712962304, 1.000000000000000000),
 ( 1.000000000000000000, 0.9450169930049948652, 1.000000000000000000),
 ( 1.000000000000000000, 0.9461610507673405834, 1.000000000000000000),
 ( 1.000000000000000000, 0.9467217966426996201, 1.000000000000000000),
 ( 1.000000000000000000, 0.9467345476124578996, 1.000000000000000000),
 ( 1.000000000000000000, 0.9461964028052806119, 1.000000000000000000),
 ( 1.000000000000000000, 0.9446801822474001353, 1.000000000000000000),
 ( 1.000000000000000000, 0.9437582546536619210, 1.000000000000000000),
 ( 1.000000000000000000, 0.9418129560295545044, 1.000000000000000000),
 ( 1.000000000000000000, 0.9418016889777601763, 1.000000000000000000),
 ( 1.000000000000000000, 0.9418517008537246049, 1.000000000000000000) ) ) 
 REPRESENTATION_ITEM ( '' )  SURFACE ( )  );
#3658 = DIRECTION ( 'NONE',  ( 0.000000000000000000, 0.000000000000000000, -1.000000000000000000 ) ) ;
#3660 = CARTESIAN_POINT ( 'NONE',  ( -44.49999999999997868, 8.366749974758366115E-15, -1.867384948185803131E-13 ) ) ;
#3659 = CARTESIAN_POINT ( 'NONE',  ( 58.74160516400053211, 1.833004249033624022, 0.3946733352257345007 ) ) ;
#3661 = CARTESIAN_POINT ( 'NONE',  ( 61.25000000000003553, -0.9999999999993586242, -1.586072192556190252 ) ) ;
#3662 = VERTEX_POINT ( 'NONE', #25703 ) ;
#3663 = CARTESIAN_POINT ( 'NONE',  ( 51.87770073550464645, 8.700057942179276083, 2.049999999999819522 ) ) ;
#3664 = CARTESIAN_POINT ( 'NONE',  ( -60.64271989919366490, -2.460423958995413773, -1.111508252306596001 ) ) ;
#3665 = ORIENTED_EDGE ( 'NONE', *, *, #21632, .T. ) ;
#3666 = CARTESIAN_POINT ( 'NONE',  ( -61.39999999999998437, -2.624491116890564690, -0.6340712715164679159 ) ) ;
#3667 = ORIENTED_EDGE ( 'NONE', *, *, #24173, .T. ) ;
#3668 = ADVANCED_FACE ( 'NONE', ( #23025 ), #6795, .F. ) ;
#3669 = LINE ( 'NONE', #20478, #23016 ) ;
#3670 = DIRECTION ( 'NONE',  ( 4.275831445896958607E-31, 1.000000000000000000, 1.224646799147353207E-16 ) ) ;
#3671 = EDGE_LOOP ( 'NONE', ( #25294, #8373, #6957, #3275 ) ) ;
#3672 = EDGE_CURVE ( 'NONE', #1297, #13242, #18947, .T. ) ;
#3673 = CARTESIAN_POINT ( 'NONE',  ( -55.94702994616203995, -2.078460969082627230, -3.600000000000206590 ) ) ;
#3674 = CARTESIAN_POINT ( 'NONE',  ( -59.14405989232412963, -3.920666489018302546E-15, 3.399999999999788969 ) ) ;
#3675 = ORIENTED_EDGE ( 'NONE', *, *, #11181, .F. ) ;
#3676 = EDGE_CURVE ( 'NONE', #29895, #7647, #26502, .T. ) ;
#3677 = VERTEX_POINT ( 'NONE', #13654 ) ;
#3678 = CARTESIAN_POINT ( 'NONE',  ( -57.43749999999996447, 1.962990915244749557, -3.400000000000195310 ) ) ;
#3679 = CARTESIAN_POINT ( 'NONE',  ( 58.66120520918180858, 0.4851952615770047106, -1.811135157337470991 ) ) ;
#3680 = CARTESIAN_POINT ( 'NONE',  ( -61.58695197172909275, -2.498609834268938901, 0.3746267610600896858 ) ) ;
#3681 = AXIS2_PLACEMENT_3D ( 'NONE', #11928, #26491, #30935 ) ;
#3682 = CARTESIAN_POINT ( 'NONE',  ( -60.54999999999995453, 1.948556695721332102E-15, 6.806719277278738347E-16 ) ) ;
#3683 = CARTESIAN_POINT ( 'NONE',  ( -73.89999999999997726, -2.435524336289708093E-15, 4.607889071584891164E-15 ) ) ;
#3684 = EDGE_CURVE ( 'NONE', #12841, #8007, #3758, .T. ) ;
#3686 = DIRECTION ( 'NONE',  ( -0.7313537016191670181, -0.6819983600625023623, 2.468850131082252722E-15 ) ) ;
#3685 = DIRECTION ( 'NONE',  ( 0.000000000000000000, 0.000000000000000000, 1.000000000000000000 ) ) ;
#3687 = B_SPLINE_CURVE_WITH_KNOTS ( 'NONE', 3,
 ( #13294, #23303, #30735, #20925 ),
 .UNSPECIFIED., .F., .F.,
 ( 4, 4 ),
 ( 0.000000000000000000, 3.288265101740379156E-05 ),
 .UNSPECIFIED. ) ;
#3688 = CARTESIAN_POINT ( 'NONE',  ( 51.12687253673779253, 0.9194130538826106314, 1.491219977510798156 ) ) ;
#3689 = DIRECTION ( 'NONE',  ( 1.000000000000000000, 1.047444401652940007E-14, 0.000000000000000000 ) ) ;
#3690 = CARTESIAN_POINT ( 'NONE',  ( 58.65838214097816206, -1.640356269755633534, -0.9083679987359125629 ) ) ;
#3691 = DIRECTION ( 'NONE',  ( 0.000000000000000000, 0.000000000000000000, 1.000000000000000000 ) ) ;
#3692 = CARTESIAN_POINT ( 'NONE',  ( -59.29999999999994031, 1.532064702718639593, 3.305310576859302518 ) ) ;
#3693 = ORIENTED_EDGE ( 'NONE', *, *, #3581, .F. ) ;
#3694 = CARTESIAN_POINT ( 'NONE',  ( -59.48573950359912743, 3.423031164920794289, -1.114835254188495162 ) ) ;
#3695 = CARTESIAN_POINT ( 'NONE',  ( 58.65000000000003411, -1.022750809560422747, 1.571497941946552457 ) ) ;
#3696 = EDGE_LOOP ( 'NONE', ( #5415, #9753, #3060, #1213, #6279, #28375 ) ) ;
#3697 = LINE ( 'NONE', #25864, #15408 ) ;
#3698 = AXIS2_PLACEMENT_3D ( 'NONE', #5324, #17852, #27489 ) ;
#3699 = CARTESIAN_POINT ( 'NONE',  ( 61.22030551133023835, 0.7785732690203674977, -1.430137637026578146 ) ) ;
#3701 = CARTESIAN_POINT ( 'NONE',  ( 51.75857864376271067, -3.767600426651517509, -1.000000000000000000 ) ) ;
#3700 = CARTESIAN_POINT ( 'NONE',  ( -56.81249999999997158, -1.962990915244707368, -3.400000000000208633 ) ) ;
#3702 = ORIENTED_EDGE ( 'NONE', *, *, #28456, .F. ) ;
#3703 = AXIS2_PLACEMENT_3D ( 'NONE', #27561, #15705, #6053 ) ;
#3704 = ORIENTED_EDGE ( 'NONE', *, *, #16126, .F. ) ;
#3705 = CARTESIAN_POINT ( 'NONE',  ( 51.60751284041730713, -4.291463206565929944, -1.660299764304736359 ) ) ;
#3706 = ORIENTED_EDGE ( 'NONE', *, *, #27001, .T. ) ;
#3707 = EDGE_CURVE ( 'NONE', #2009, #10802, #17415, .T. ) ;
#3708 = DIRECTION ( 'NONE',  ( 1.000000000000000000, 1.047444401652940007E-14, 0.000000000000000000 ) ) ;
#3709 = ORIENTED_EDGE ( 'NONE', *, *, #4981, .F. ) ;
#3710 = CARTESIAN_POINT ( 'NONE',  ( 22.09542497983174414, 7.445411299648926118, -2.050000000000211209 ) ) ;
#3711 = CARTESIAN_POINT ( 'NONE',  ( -60.59999999999997300, 1.626093840209163176E-15, 1.891350188320046374E-15 ) ) ;
#3712 = CARTESIAN_POINT ( 'NONE',  ( -62.09999999999997300, 1.168016602258162478E-15, 2.197726754101795588E-15 ) ) ;
#3713 = ORIENTED_EDGE ( 'NONE', *, *, #27923, .F. ) ;
#3714 = CARTESIAN_POINT ( 'NONE',  ( 51.80000000000001847, 1.521694824349937303, 3.995005614707771269 ) ) ;
#3715 = CARTESIAN_POINT ( 'NONE',  ( -60.64405989232412253, -3.920666489018283614E-15, 3.399999999999783640 ) ) ;
#3716 = CARTESIAN_POINT ( 'NONE',  ( 47.73617949479463363, -3.930543434675368264, 1.171429914303333764 ) ) ;
#3717 = CARTESIAN_POINT ( 'NONE',  ( 58.72200624034169891, 1.310319377727330536, 1.341335979947728241 ) ) ;
#3718 = EDGE_CURVE ( 'NONE', #2667, #9046, #25996, .T. ) ;
#3719 = DIRECTION ( 'NONE',  ( -1.000000000000000000, 0.000000000000000000, 1.047444401652940007E-14 ) ) ;
#3720 = CARTESIAN_POINT ( 'NONE',  ( 54.15675781068899397, 5.684314874070254042, -2.050000000000189004 ) ) ;
#3722 = CYLINDRICAL_SURFACE ( 'NONE', #15409, 3.399999999999999911 ) ;
#3721 = CARTESIAN_POINT ( 'NONE',  ( 51.13989201884552926, -0.9305404255924549783, 1.499649012356545130 ) ) ;
#3723 = VECTOR ( 'NONE', #6519, 1000.000000000000000 ) ;
#3724 = AXIS2_PLACEMENT_3D ( 'NONE', #19466, #21704, #14378 ) ;
#3725 = DIRECTION ( 'NONE',  ( -1.000000000000000000, -3.053848253006669023E-16, 2.042510438544995415E-16 ) ) ;
#3726 = CARTESIAN_POINT ( 'NONE',  ( 64.99999999999997158, -1.025519176787267142E-28, -3.500000000000680345 ) ) ;
#3727 = DIRECTION ( 'NONE',  ( 0.000000000000000000, 0.000000000000000000, 1.000000000000000000 ) ) ;
#3728 = VERTEX_POINT ( 'NONE', #25534 ) ;
#3729 = CARTESIAN_POINT ( 'NONE',  ( 54.15683185445048764, 5.684290329229592764, -2.050000000000188560 ) ) ;
#3730 = EDGE_LOOP ( 'NONE', ( #15344, #21220, #10138, #18219 ) ) ;
#3731 = CARTESIAN_POINT ( 'NONE',  ( -59.38263816597098099, 3.123852333407923787, -1.389329043195103752 ) ) ;
#3732 = ORIENTED_EDGE ( 'NONE', *, *, #2379, .T. ) ;
#3733 = CARTESIAN_POINT ( 'NONE',  ( 53.89553379148921408, 6.017104844469294278, 2.049999999999811973 ) ) ;
#3734 = CARTESIAN_POINT ( 'NONE',  ( -55.59585481156724285, 3.673546848079182414, 0.7533615035078059519 ) ) ;
#3736 = CARTESIAN_POINT ( 'NONE',  ( -54.49999999999997868, -1.550000000000000044, 3.332135201338624508 ) ) ;
#3735 = DIRECTION ( 'NONE',  ( -1.000000000000000000, -3.053848253006669023E-16, 2.042510438544995169E-16 ) ) ;
#3737 = ORIENTED_EDGE ( 'NONE', *, *, #10619, .F. ) ;
#3738 = ORIENTED_EDGE ( 'NONE', *, *, #8941, .F. ) ;
#3739 = CARTESIAN_POINT ( 'NONE',  ( 31.46405049521009545, 7.544521452532235273, -2.050000000000109956 ) ) ;
#3740 = EDGE_CURVE ( 'NONE', #9407, #8968, #3755, .T. ) ;
#3741 = CARTESIAN_POINT ( 'NONE',  ( 57.04073536323585358, -0.7493370604887438224, -1.778939771162194372 ) ) ;
#3742 = ORIENTED_EDGE ( 'NONE', *, *, #4272, .T. ) ;
#3744 = DIRECTION ( 'NONE',  ( 0.000000000000000000, -0.9996898646859344595, -0.02490330187381133153 ) ) ;
#3743 = CYLINDRICAL_SURFACE ( 'NONE', #21161, 0.09999999999999982514 ) ;
#3745 = DIRECTION ( 'NONE',  ( 1.000000000000000000, 0.000000000000000000, 0.000000000000000000 ) ) ;
#3746 = VERTEX_POINT ( 'NONE', #17693 ) ;
#3747 = AXIS2_PLACEMENT_3D ( 'NONE', #6171, #15818, #20750 ) ;
#3748 = CARTESIAN_POINT ( 'NONE',  ( -36.11187263677958015, 5.068523420888933373, -1.228242390833621300 ) ) ;
#3749 = EDGE_CURVE ( 'NONE', #28771, #23537, #16905, .T. ) ;
#3750 = CARTESIAN_POINT ( 'NONE',  ( 58.75000000000000000, 1.571497941947157972, -1.022750809561051133 ) ) ;
#3751 = DIRECTION ( 'NONE',  ( 1.000000000000000000, 0.000000000000000000, -3.491481338843133355E-15 ) ) ;
#3752 = CARTESIAN_POINT ( 'NONE',  ( -44.49999999999997868, 8.366749974758269874E-15, -1.589829192029513996E-13 ) ) ;
#3753 = CARTESIAN_POINT ( 'NONE',  ( -67.88621053311027254, 1.613288973786557223, 0.04018868625473467210 ) ) ;
#3754 = CIRCLE ( 'NONE', #5797, 0.1000000000000000472 ) ;
#3755 = CIRCLE ( 'NONE', #12825, 0.4400000000000000577 ) ;
#3756 = EDGE_CURVE ( 'NONE', #19802, #25428, #26431, .T. ) ;
#3757 = DIRECTION ( 'NONE',  ( 1.000000000000000000, 3.054025858079668409E-16, -2.042474015755241579E-16 ) ) ;
#3758 = B_SPLINE_CURVE_WITH_KNOTS ( 'NONE', 3,
 ( #29393, #6233, #24803, #23336 ),
 .UNSPECIFIED., .F., .F.,
 ( 4, 4 ),
 ( 0.000000000000000000, 1.000000000000000000 ),
 .UNSPECIFIED. ) ;
#3759 = CARTESIAN_POINT ( 'NONE',  ( -55.04792740578361077, 3.330682475591790315, 0.6830477631804110494 ) ) ;
#3760 = CARTESIAN_POINT ( 'NONE',  ( 53.61178450975653220, 7.592125988483584997, -1.856626124458810256 ) ) ;
#3761 = CIRCLE ( 'NONE', #4786, 0.1000000000000000472 ) ;
#3762 = EDGE_CURVE ( 'NONE', #23733, #27840, #7293, .T. ) ;
#3763 = DIRECTION ( 'NONE',  ( 1.000000000000000000, 1.047444401652940007E-14, 0.000000000000000000 ) ) ;
#3764 = LINE ( 'NONE', #8670, #25720 ) ;
#3765 = DIRECTION ( 'NONE',  ( 0.000000000000000000, 0.000000000000000000, 1.000000000000000000 ) ) ;
#3766 = ORIENTED_EDGE ( 'NONE', *, *, #3617, .T. ) ;
#3767 = CARTESIAN_POINT ( 'NONE',  ( 58.72200624034164207, 1.612834625125591614, 0.9564954546397232971 ) ) ;
#3768 = VERTEX_POINT ( 'NONE', #2963 ) ;
#3769 = CARTESIAN_POINT ( 'NONE',  ( 51.45655683570191741, -0.9591657938390834026, 1.611094652690528095 ) ) ;
#3771 = PLANE ( 'NONE',  #6068 ) ;
#3770 = CARTESIAN_POINT ( 'NONE',  ( 48.40000000000002700, 0.6462379109121008103, 4.048750000000028493 ) ) ;
#3772 = EDGE_LOOP ( 'NONE', ( #12572, #6493, #29764, #21015 ) ) ;
#3773 = ORIENTED_EDGE ( 'NONE', *, *, #24286, .T. ) ;
#3774 = CARTESIAN_POINT ( 'NONE',  ( 53.91574522235882228, 6.672251602522421443, 1.774295301432037286 ) ) ;
#3775 = ADVANCED_FACE ( 'NONE', ( #12608 ), #29038, .T. ) ;
#3776 = DIRECTION ( 'NONE',  ( 0.000000000000000000, 0.000000000000000000, 1.000000000000000000 ) ) ;
#3777 = SHAPE_REPRESENTATION ( 'Cap', ( #9018 ), #25221 ) ;
#3779 = CARTESIAN_POINT ( 'NONE',  ( 58.65000000000000568, 1.022750809560621699, 1.571497941947222587 ) ) ;
#3778 = DIRECTION ( 'NONE',  ( 1.000000000000000000, 0.000000000000000000, 0.000000000000000000 ) ) ;
#3780 = EDGE_CURVE ( 'NONE', #1641, #22580, #15100, .T. ) ;
#3781 = ORIENTED_EDGE ( 'NONE', *, *, #12654, .T. ) ;
#3782 = CARTESIAN_POINT ( 'NONE',  ( -56.48542740578359656, 2.936324665650207333, 2.606018187048499080 ) ) ;
#3783 = ADVANCED_FACE ( 'NONE', ( #8603 ), #13837, .T. ) ;
#3784 = CIRCLE ( 'NONE', #16427, 3.200000000000000178 ) ;
#3785 = DIRECTION ( 'NONE',  ( 1.000000000000000000, 0.000000000000000000, 0.000000000000000000 ) ) ;
#3786 = APPLICATION_PROTOCOL_DEFINITION ( 'draft international standard', 'automotive_design', 1998, #22700 ) ;
#3787 = DIRECTION ( 'NONE',  ( 1.000000000000000000, 1.047444401652940007E-14, 0.000000000000000000 ) ) ;
#3788 = CIRCLE ( 'NONE', #25024, 0.05000000000000009298 ) ;
#3789 = ORIENTED_EDGE ( 'NONE', *, *, #20362, .F. ) ;
#3790 = EDGE_CURVE ( 'NONE', #11190, #29758, #4787, .T. ) ;
#3791 = CARTESIAN_POINT ( 'NONE',  ( -61.13452994616202574, 2.093608279459375190E-14, -3.600000000000216804 ) ) ;
#3792 = AXIS2_PLACEMENT_3D ( 'NONE', #25874, #13813, #27502 ) ;
#3793 = ORIENTED_EDGE ( 'NONE', *, *, #10433, .F. ) ;
#3794 = CARTESIAN_POINT ( 'NONE',  ( 52.10582242447213019, 8.700707108360601794, -2.050000000000181455 ) ) ;
#3795 = FACE_OUTER_BOUND ( 'NONE', #16966, .T. ) ;
#3796 = DIRECTION ( 'NONE',  ( 0.000000000000000000, -0.9996898646859343485, -0.02490330187381123786 ) ) ;
#3798 = DIRECTION ( 'NONE',  ( 0.000000000000000000, -1.000000000000000000, -4.336808689942015369E-15 ) ) ;
#3797 = CARTESIAN_POINT ( 'NONE',  ( 69.20000000000001705, 0.4500000000000000111, -1.988246715074080573 ) ) ;
#3799 = EDGE_CURVE ( 'NONE', #3728, #14710, #26024, .T. ) ;
#3800 = AXIS2_PLACEMENT_3D ( 'NONE', #1579, #9352, #28351 ) ;
#3801 = CARTESIAN_POINT ( 'NONE',  ( -54.49999999999999289, -1.400000000000007017, 4.029888335921757658 ) ) ;
#3803 = CARTESIAN_POINT ( 'NONE',  ( -62.09999999999997300, -2.722123828016836722, -0.3761544999221376195 ) ) ;
#3802 = CARTESIAN_POINT ( 'NONE',  ( 61.25000000000002132, 6.415596960124259844E-13, 3.111507638930570854E-58 ) ) ;
#3804 = CIRCLE ( 'NONE', #8860, 0.1000000000000000472 ) ;
#3805 = ORIENTED_EDGE ( 'NONE', *, *, #29545, .T. ) ;
#3806 = DIRECTION ( 'NONE',  ( 2.265029845352616032E-44, -1.000000000000000000, -3.491481338843140061E-15 ) ) ;
#3807 = EDGE_CURVE ( 'NONE', #24533, #27460, #23472, .T. ) ;
#3808 = CARTESIAN_POINT ( 'NONE',  ( -35.85663232820584057, 2.199885893005988358, -4.939696249117657700 ) ) ;
#3810 = FACE_OUTER_BOUND ( 'NONE', #12170, .T. ) ;
#3809 = DIRECTION ( 'NONE',  ( 0.000000000000000000, 0.000000000000000000, 1.000000000000000000 ) ) ;
#3811 = DIRECTION ( 'NONE',  ( 1.000000000000000000, 0.000000000000000000, -1.047444401652940007E-14 ) ) ;
#3812 = AXIS2_PLACEMENT_3D ( 'NONE', #11235, #21247, #30544 ) ;
#3813 = ORIENTED_EDGE ( 'NONE', *, *, #14851, .T. ) ;
#3814 = CARTESIAN_POINT ( 'NONE',  ( 53.75952070206893296, 7.747157889885662563, 2.049999999999812417 ) ) ;
#3815 = CARTESIAN_POINT ( 'NONE',  ( 50.25000000000000000, 1.499837071478580919, -1.323060376180706710 ) ) ;
#3816 = CIRCLE ( 'NONE', #21546, 0.1500000000000001887 ) ;
#3817 = VERTEX_POINT ( 'NONE', #30595 ) ;
#3818 = AXIS2_PLACEMENT_3D ( 'NONE', #8982, #24017, #28305 ) ;
#3819 = EDGE_CURVE ( 'NONE', #22708, #13977, #21974, .T. ) ;
#3820 = FACE_OUTER_BOUND ( 'NONE', #13623, .T. ) ;
#3821 = ORIENTED_EDGE ( 'NONE', *, *, #13783, .F. ) ;
#3822 = EDGE_CURVE ( 'NONE', #6667, #22071, #6549, .T. ) ;
#3823 = CARTESIAN_POINT ( 'NONE',  ( 15.18459684427939749, 2.199885893006011006, -4.939696249117653259 ) ) ;
#3824 = CARTESIAN_POINT ( 'NONE',  ( 47.75910361055753839, -4.379721596991718258, -1.407221449367546784 ) ) ;
#3825 = ORIENTED_EDGE ( 'NONE', *, *, #16917, .F. ) ;
#3826 = CARTESIAN_POINT ( 'NONE',  ( 24.99011192183064978, 5.348094263731223208, 1.949999999999912248 ) ) ;
#3827 = CARTESIAN_POINT ( 'NONE',  ( -57.20655989232410832, 1.962990915244748891, -3.400000000000194422 ) ) ;
#3828 = EDGE_LOOP ( 'NONE', ( #23113, #13981, #14538, #25545 ) ) ;
#3829 = ORIENTED_EDGE ( 'NONE', *, *, #25537, .F. ) ;
#3830 = VECTOR ( 'NONE', #23103, 1000.000000000000000 ) ;
#3831 = VERTEX_POINT ( 'NONE', #4160 ) ;
#3832 = TOROIDAL_SURFACE ( 'NONE', #29130, 4.600000000000000533, 0.4999999999999996669 ) ;
#3833 = CARTESIAN_POINT ( 'NONE',  ( -57.68749999999996447, -3.925981830489445379, -2.189747187108473037E-13 ) ) ;
#3834 = CARTESIAN_POINT ( 'NONE',  ( 58.65000090395037802, 0.5493607500728427961, -1.793027323413543650 ) ) ;
#3835 = CARTESIAN_POINT ( 'NONE',  ( 24.79176202108331850, 5.385922622694285344, -1.425000000000086198 ) ) ;
#3836 = AXIS2_PLACEMENT_3D ( 'NONE', #5703, #8382, #22493 ) ;
#3837 = CARTESIAN_POINT ( 'NONE',  ( 51.25000000000002842, -1.487499999999465361, 1.821662113731690703E-16 ) ) ;
#3838 = CARTESIAN_POINT ( 'NONE',  ( -54.44999999999997442, 0.000000000000000000, 0.000000000000000000 ) ) ;
#3839 = AXIS2_PLACEMENT_3D ( 'NONE', #10193, #5277, #19720 ) ;
#3840 = AXIS2_PLACEMENT_3D ( 'NONE', #13794, #18748, #6694 ) ;
#3841 = MECHANICAL_DESIGN_GEOMETRIC_PRESENTATION_REPRESENTATION (  '', ( #23098 ), #17027 ) ;
#3843 = CYLINDRICAL_SURFACE ( 'NONE', #28057, 4.600000000000036948 ) ;
#3842 = CARTESIAN_POINT ( 'NONE',  ( 15.03925126672132961, -2.686240680702127737, -4.475885388010735433 ) ) ;
#3844 = EDGE_CURVE ( 'NONE', #14189, #1752, #2699, .T. ) ;
#3845 = B_SPLINE_CURVE_WITH_KNOTS ( 'NONE', 3,
 ( #2611, #2286, #19563, #23986 ),
 .UNSPECIFIED., .F., .F.,
 ( 4, 4 ),
 ( 0.000000000000000000, 1.854844919671783956E-05 ),
 .UNSPECIFIED. ) ;
#3846 = DIRECTION ( 'NONE',  ( 0.000000000000000000, -1.000000000000000000, -3.491481338843130594E-15 ) ) ;
#3847 = EDGE_CURVE ( 'NONE', #26053, #4809, #15343, .T. ) ;
#3848 = CARTESIAN_POINT ( 'NONE',  ( -55.68749999999997158, -4.108500314926507357, 1.367561758111403680 ) ) ;
#3849 = CARTESIAN_POINT ( 'NONE',  ( 58.73371041428932671, -1.582294810366662308, -1.006219588948326304 ) ) ;
#3850 = CIRCLE ( 'NONE', #18015, 0.05000000000000012768 ) ;
#3851 = DIRECTION ( 'NONE',  ( 1.000000000000000000, -1.219044193948983948E-29, 3.491481338843133355E-15 ) ) ;
#3852 = EDGE_CURVE ( 'NONE', #207, #15867, #9041, .T. ) ;
#3853 = CARTESIAN_POINT ( 'NONE',  ( -59.29999999999996163, 0.3064839379836800104, 3.562026904852408471 ) ) ;
#3854 = ORIENTED_EDGE ( 'NONE', *, *, #23079, .F. ) ;
#3855 = CARTESIAN_POINT ( 'NONE',  ( 51.59739104186227365, 1.010292945603182169, -1.272765950230260401 ) ) ;
#3856 = VECTOR ( 'NONE', #15914, 1000.000000000000000 ) ;
#3857 =( NAMED_UNIT ( * ) PLANE_ANGLE_UNIT ( ) SI_UNIT ( $, .RADIAN. ) );
#3858 = CIRCLE ( 'NONE', #311, 0.1500000000000001887 ) ;
#3859 = ORIENTED_EDGE ( 'NONE', *, *, #30155, .T. ) ;
#3860 = CARTESIAN_POINT ( 'NONE',  ( -77.28999999999996362, -3.470778894058966809E-15, 5.300300110251643219E-15 ) ) ;
#3862 = DIRECTION ( 'NONE',  ( -0.9993908270191184107, 0.03489949670185085034, 3.491481338843133355E-15 ) ) ;
#3861 = CARTESIAN_POINT ( 'NONE',  ( -55.12499999999997158, 2.944486372867106905, -1.700000000000183364 ) ) ;
#3863 = VERTEX_POINT ( 'NONE', #11921 ) ;
#3864 = CIRCLE ( 'NONE', #30640, 4.000000000000022204 ) ;
#3865 = ORIENTED_EDGE ( 'NONE', *, *, #9634, .T. ) ;
#3866 = DIRECTION ( 'NONE',  ( 0.000000000000000000, -0.2008964009354147484, 0.9796124928211139560 ) ) ;
#3867 = ORIENTED_EDGE ( 'NONE', *, *, #8777, .T. ) ;
#3868 = AXIS2_PLACEMENT_3D ( 'NONE', #22289, #7698, #5794 ) ;
#3870 = CARTESIAN_POINT ( 'NONE',  ( 51.13585994975460380, 0.9262448312174480503, -1.518514878530177192 ) ) ;
#3869 = AXIS2_PLACEMENT_3D ( 'NONE', #11567, #28818, #21242 ) ;
#3871 = EDGE_LOOP ( 'NONE', ( #16670, #13448, #102, #26624 ) ) ;
#3872 = CARTESIAN_POINT ( 'NONE',  ( -59.59999999999997300, -2.337126060168364994, -1.249136413240117038 ) ) ;
#3873 = CYLINDRICAL_SURFACE ( 'NONE', #8606, 2.649999999999999911 ) ;
#3874 = FACE_OUTER_BOUND ( 'NONE', #21190, .T. ) ;
#3875 = EDGE_LOOP ( 'NONE', ( #1794, #15851, #2274, #3593 ) ) ;
#3876 = DIRECTION ( 'NONE',  ( 0.000000000000000000, 1.000000000000000000, 0.000000000000000000 ) ) ;
#3877 = CARTESIAN_POINT ( 'NONE',  ( 50.25000000000004263, -1.960427193528405887, -0.3958853607747112036 ) ) ;
#3878 = CARTESIAN_POINT ( 'NONE',  ( 57.05000000000001847, -0.8156862745098041323, -2.468735688885368873 ) ) ;
#3879 = AXIS2_PLACEMENT_3D ( 'NONE', #6964, #16449, #11703 ) ;
#3880 = CARTESIAN_POINT ( 'NONE',  ( 53.21917409580245817, 8.083376426877231680, -1.902110155464870944 ) ) ;
#3881 = AXIS2_PLACEMENT_3D ( 'NONE', #8290, #17959, #25235 ) ;
#3882 = CARTESIAN_POINT ( 'NONE',  ( 58.75000000000001421, 1.253243060177670509, 1.394635017528978560 ) ) ;
#3883 = CIRCLE ( 'NONE', #21613, 0.2500000000000000000 ) ;
#3884 = LINE ( 'NONE', #1812, #14636 ) ;
#3885 = VECTOR ( 'NONE', #2214, 1000.000000000000000 ) ;
#3886 = DIRECTION ( 'NONE',  ( 0.000000000000000000, 0.000000000000000000, 1.000000000000000000 ) ) ;
#3887 = CIRCLE ( 'NONE', #5403, 0.09999999999999997780 ) ;
#3888 = EDGE_CURVE ( 'NONE', #27612, #11116, #23804, .T. ) ;
#3889 = AXIS2_PLACEMENT_3D ( 'NONE', #12820, #3181, #8698 ) ;
#3890 = FACE_OUTER_BOUND ( 'NONE', #17344, .T. ) ;
#3891 = EDGE_CURVE ( 'NONE', #14560, #10413, #6245, .T. ) ;
#3892 = CARTESIAN_POINT ( 'NONE',  ( -58.97085481156723574, -3.673546848079176197, -0.7533615035078063960 ) ) ;
#3893 = AXIS2_PLACEMENT_3D ( 'NONE', #29048, #7357, #4987 ) ;
#3894 = CARTESIAN_POINT ( 'NONE',  ( 50.25000000000002842, -1.106298139390672564, 1.666164585743104443 ) ) ;
#3895 = AXIS2_PLACEMENT_3D ( 'NONE', #1810, #21168, #31105 ) ;
#3896 = VERTEX_POINT ( 'NONE', #14904 ) ;
#3897 = CARTESIAN_POINT ( 'NONE',  ( 53.96125931204732495, 5.169815675097246377, -2.050000000000188116 ) ) ;
#3898 = EDGE_LOOP ( 'NONE', ( #13346, #29072, #6953, #9318 ) ) ;
#3899 = CARTESIAN_POINT ( 'NONE',  ( 51.80000000000003268, -3.637377585518695611, 2.099877210782855830 ) ) ;
#3900 = EDGE_LOOP ( 'NONE', ( #17794, #8347, #23386, #6319 ) ) ;
#3901 = CARTESIAN_POINT ( 'NONE',  ( 51.38825337055899922, 3.875334094704443899, 2.049999999999820410 ) ) ;
#3902 = CARTESIAN_POINT ( 'NONE',  ( -56.53335481156724285, 0.8699069336946694264, -4.241846523238430144 ) ) ;
#3904 = CARTESIAN_POINT ( 'NONE',  ( -36.31414349454750123, 3.102491976071082735, 4.173461118157660188 ) ) ;
#3903 = CARTESIAN_POINT ( 'NONE',  ( 47.00000000000002132, 1.734723475976807094E-15, 4.275000000000000355 ) ) ;
#3905 = AXIS2_PLACEMENT_3D ( 'NONE', #8379, #20754, #17896 ) ;
#3906 = ORIENTED_EDGE ( 'NONE', *, *, #18111, .T. ) ;
#3907 = EDGE_LOOP ( 'NONE', ( #15999, #23196, #12657, #24000, #5776, #33 ) ) ;
#3908 = CARTESIAN_POINT ( 'NONE',  ( 24.79155133983196180, 5.500688705494902742, -2.050000000000086420 ) ) ;
#3909 = CIRCLE ( 'NONE', #18569, 0.1500000000000000777 ) ;
#3910 = EDGE_CURVE ( 'NONE', #14828, #5117, #7265, .T. ) ;
#3911 = DIRECTION ( 'NONE',  ( 1.000000000000000000, 3.054025858079668409E-16, -2.042474015755241579E-16 ) ) ;
#3912 = AXIS2_PLACEMENT_3D ( 'NONE', #16435, #13878, #18982 ) ;
#3913 = ORIENTED_EDGE ( 'NONE', *, *, #9715, .F. ) ;
#3915 = DIRECTION ( 'NONE',  ( 1.000000000000000000, 1.047444401652940007E-14, 0.000000000000000000 ) ) ;
#3914 = CARTESIAN_POINT ( 'NONE',  ( -55.95655989232413674, -3.399999999999990585, -2.144552914728849773E-13 ) ) ;
#3916 = CARTESIAN_POINT ( 'NONE',  ( 47.00000000000002842, -3.637377585518695611, 2.099877210782872261 ) ) ;
#3917 = ORIENTED_EDGE ( 'NONE', *, *, #14628, .F. ) ;
#3918 = CARTESIAN_POINT ( 'NONE',  ( -36.58361892165972762, 5.109611055794863077, -1.772889539330479547 ) ) ;
#3919 = DIRECTION ( 'NONE',  ( 0.5633368246415176861, -0.8262273428075422865, 0.000000000000000000 ) ) ;
#3920 = CIRCLE ( 'NONE', #27677, 1.874999999999998668 ) ;
#3921 = DIRECTION ( 'NONE',  ( 0.000000000000000000, 1.000000000000000000, 4.336808689942015369E-15 ) ) ;
#3922 = CARTESIAN_POINT ( 'NONE',  ( 52.20711756518982583, 0.7500000000005468959, -1.718465885608440269 ) ) ;
#3923 = AXIS2_PLACEMENT_3D ( 'NONE', #2419, #9709, #7317 ) ;
#3924 = AXIS2_PLACEMENT_3D ( 'NONE', #17146, #19518, #12672 ) ;
#3925 = CARTESIAN_POINT ( 'NONE',  ( -57.00952994616205416, -4.643455692769903542E-15, 3.599999999999796696 ) ) ;
#3926 = CARTESIAN_POINT ( 'NONE',  ( 15.30042582489668312, 4.018128186974561089, 3.618665893507494236 ) ) ;
#3927 = VECTOR ( 'NONE', #13385, 1000.000000000000000 ) ;
#3928 = AXIS2_PLACEMENT_3D ( 'NONE', #21061, #3635, #28165 ) ;
#3929 = CARTESIAN_POINT ( 'NONE',  ( -58.86042740578361077, 3.725040285533377737, -1.239922660687654554 ) ) ;
#3930 = EDGE_CURVE ( 'NONE', #12969, #26147, #10284, .T. ) ;
#3931 = TOROIDAL_SURFACE ( 'NONE', #28718, 4.000000000000022204, 0.1000000000000000056 ) ;
#3932 = CARTESIAN_POINT ( 'NONE',  ( -56.90835481156724285, -0.7533615035077978472, 3.673546848079179750 ) ) ;
#3933 = CARTESIAN_POINT ( 'NONE',  ( 51.24099374247644789, 1.086790822299315895, 1.208135181987621598 ) ) ;
#3934 = CARTESIAN_POINT ( 'NONE',  ( 53.29168147589466997, 4.961551560356480373, 1.611466093477803785 ) ) ;
#3935 = DIRECTION ( 'NONE',  ( -1.000000000000000000, 0.000000000000000000, -0.000000000000000000 ) ) ;
#3936 = ORIENTED_EDGE ( 'NONE', *, *, #5923, .F. ) ;
#3937 = CARTESIAN_POINT ( 'NONE',  ( -54.49999999999997868, 3.624999999999963585, -2.089966883537054476E-13 ) ) ;
#3938 = ORIENTED_EDGE ( 'NONE', *, *, #1166, .T. ) ;
#3939 = CARTESIAN_POINT ( 'NONE',  ( 51.87416143049284756, 8.598705507415681737, 1.976179938779733858 ) ) ;
#3941 = CARTESIAN_POINT ( 'NONE',  ( -57.72499999999997300, -0.9241234443029058276, 4.506217466977124886 ) ) ;
#3940 = CARTESIAN_POINT ( 'NONE',  ( 48.38577482684819131, 1.132063507975338945, 3.941224428058327511 ) ) ;
#3942 = ORIENTED_EDGE ( 'NONE', *, *, #19332, .F. ) ;
#3943 = CYLINDRICAL_SURFACE ( 'NONE', #1723, 5.407411300779133789 ) ;
#3944 = EDGE_CURVE ( 'NONE', #22261, #10512, #26962, .T. ) ;
#3945 = FACE_OUTER_BOUND ( 'NONE', #22403, .T. ) ;
#3947 = CARTESIAN_POINT ( 'NONE',  ( -55.40835481156723574, -0.7533615035078004007, 3.673546848079179306 ) ) ;
#3946 = CARTESIAN_POINT ( 'NONE',  ( 51.30576788583277903, -4.280519502657941899, -1.378181460054113794 ) ) ;
#3948 = EDGE_LOOP ( 'NONE', ( #3291, #7536, #24172, #10290, #12318 ) ) ;
#3949 = CARTESIAN_POINT ( 'NONE',  ( -58.48542740578359656, -3.725040285533365303, 1.239922660687675648 ) ) ;
#3950 = DIRECTION ( 'NONE',  ( -3.489354422748178582E-15, 1.218509414717996338E-16, -1.000000000000000000 ) ) ;
#3951 = CONTEXT_DEPENDENT_SHAPE_REPRESENTATION ( #10196, #10827 ) ;
#3952 = CARTESIAN_POINT ( 'NONE',  ( -59.40743313238012036, 2.395752775956333291, 1.250136525132548027 ) ) ;
#3953 = CARTESIAN_POINT ( 'NONE',  ( -54.49999999999997868, -1.549999999999999600, 4.064480286580312907 ) ) ;
#3954 = CARTESIAN_POINT ( 'NONE',  ( -60.64999999999998437, -2.458515422985869670, -1.116110171506649040 ) ) ;
#3955 = ORIENTED_EDGE ( 'NONE', *, *, #25501, .F. ) ;
#3956 = DIRECTION ( 'NONE',  ( 3.489354422748178582E-15, -1.218509414717996338E-16, 1.000000000000000000 ) ) ;
#3957 = CARTESIAN_POINT ( 'NONE',  ( -36.38012252111052902, 2.292272662152775364, -4.901537128432196688 ) ) ;
#3958 = CARTESIAN_POINT ( 'NONE',  ( 50.25000000000004263, -2.079005547593277381, 1.932245437381540134E-15 ) ) ;
#3959 = CARTESIAN_POINT ( 'NONE',  ( 50.85906935218978475, 8.675599908283860628, 2.049999999999822631 ) ) ;
#3960 = EDGE_CURVE ( 'NONE', #9996, #3746, #16638, .T. ) ;
#3962 = CARTESIAN_POINT ( 'NONE',  ( 58.65000045311414567, -1.787855644601539451, -0.5652242121843152889 ) ) ;
#3961 = CARTESIAN_POINT ( 'NONE',  ( -55.40835481156723574, -0.7533615035078004007, 3.673546848079179306 ) ) ;
#3963 = EDGE_CURVE ( 'NONE', #10732, #21532, #8309, .T. ) ;
#3964 = TOROIDAL_SURFACE ( 'NONE', #25716, 3.250821294908289971, 0.05000000000000000278 ) ;
#3965 = TOROIDAL_SURFACE ( 'NONE', #23703, 3.675000000000000711, 0.05000000000000000278 ) ;
#3966 = CARTESIAN_POINT ( 'NONE',  ( 50.35762544161294585, 8.151359338959888845, -2.050000000000174794 ) ) ;
#3968 = DIRECTION ( 'NONE',  ( 0.000000000000000000, 0.000000000000000000, 1.000000000000000000 ) ) ;
#3967 = DIRECTION ( 'NONE',  ( 1.000000000000000000, 3.053848253006669023E-16, -2.042510438544995415E-16 ) ) ;
#3969 = VERTEX_POINT ( 'NONE', #2430 ) ;
#3970 =( BOUNDED_SURFACE ( )  B_SPLINE_SURFACE ( 3, 2, ( 
 ( #8463, #18141, #27780 ),
 ( #25395, #3699, #23031 ),
 ( #10995, #25542, #13512 ),
 ( #16854, #7503, #4322 ),
 ( #21306, #19239, #28555 ),
 ( #1961, #9578, #26661 ) ),
 .UNSPECIFIED., .F., .F., .F. ) 
 B_SPLINE_SURFACE_WITH_KNOTS ( ( 4, 2, 4 ),
 ( 3, 3 ),
 ( 5.963111948670274387E-19, 0.0002090583013612447186, 0.0004181166027224888409 ),
 ( 0.000000000000000000, 1.000000000000000000 ),
 .UNSPECIFIED. ) 
 GEOMETRIC_REPRESENTATION_ITEM ( )  RATIONAL_B_SPLINE_SURFACE ( (
 ( 1.000000000000000000, 0.7071067811865358044, 1.000000000000000000),
 ( 1.000000000000000000, 0.7521684882082442236, 1.000000000000000000),
 ( 1.000000000000000000, 0.7851308282770599334, 1.000000000000000000),
 ( 1.000000000000000000, 0.8276934144745562438, 1.000000000000000000),
 ( 1.000000000000000000, 0.8364441017664440148, 1.000000000000000000),
 ( 1.000000000000000000, 0.8366600265340728981, 1.000000000000000000) ) ) 
 REPRESENTATION_ITEM ( '' )  SURFACE ( )  );
#3971 = CARTESIAN_POINT ( 'NONE',  ( -62.06697778907421537, -2.637963160708082899, -0.3297769518696585522 ) ) ;
#3972 = DIRECTION ( 'NONE',  ( 0.000000000000000000, 0.000000000000000000, -1.000000000000000000 ) ) ;
#3974 = CARTESIAN_POINT ( 'NONE',  ( -59.60675767627768096, -2.338930541566021759, -1.245993773302377816 ) ) ;
#3973 = CARTESIAN_POINT ( 'NONE',  ( 58.65263613458532888, 1.827305695291647547, 0.4205413283056451679 ) ) ;
#3975 = FACE_OUTER_BOUND ( 'NONE', #3204, .T. ) ;
#3976 = ORIENTED_EDGE ( 'NONE', *, *, #6682, .T. ) ;
#3977 = CARTESIAN_POINT ( 'NONE',  ( 53.82285890661303540, 4.901445667019300068, 2.049999999999811973 ) ) ;
#3978 = DIRECTION ( 'NONE',  ( -1.000000000000000000, -3.054025858079668409E-16, 2.042474015755241579E-16 ) ) ;
#3979 = ADVANCED_FACE ( 'NONE', ( #5107 ), #19692, .T. ) ;
#3980 = ORIENTED_EDGE ( 'NONE', *, *, #10979, .T. ) ;
#3981 = CARTESIAN_POINT ( 'NONE',  ( 51.80000048712027905, 3.919471135816211316, 2.045252759501752227 ) ) ;
#3982 = EDGE_LOOP ( 'NONE', ( #16502, #9555, #23547, #29036 ) ) ;
#3983 = CARTESIAN_POINT ( 'NONE',  ( 48.00000000000001421, -4.387164041431065975, -1.383037119376926194 ) ) ;
#3984 = CARTESIAN_POINT ( 'NONE',  ( -73.89999999999997726, -1.259609229504280004, -0.03137816036099756040 ) ) ;
#3985 = ORIENTED_EDGE ( 'NONE', *, *, #4616, .T. ) ;
#3986 = CARTESIAN_POINT ( 'NONE',  ( 24.11041436609877309, 5.625678654145607638, 1.949999999999915801 ) ) ;
#3987 = CARTESIAN_POINT ( 'NONE',  ( -56.01905989232412963, -2.944486372867088697, 1.699999999999789679 ) ) ;
#3988 = ORIENTED_EDGE ( 'NONE', *, *, #18972, .F. ) ;
#3989 = CARTESIAN_POINT ( 'NONE',  ( 56.95220615073115056, 0.7055010433615873655, -1.764201441664152270 ) ) ;
#3990 = ORIENTED_EDGE ( 'NONE', *, *, #30078, .T. ) ;
#3991 = EDGE_CURVE ( 'NONE', #8886, #28473, #21186, .T. ) ;
#3992 = EDGE_LOOP ( 'NONE', ( #21304, #17259, #23825, #18720 ) ) ;
#3993 = PRESENTATION_LAYER_ASSIGNMENT (  '', '', ( #4497 ) ) ;
#3994 = CIRCLE ( 'NONE', #4994, 0.1000000000000000472 ) ;
#3995 = CARTESIAN_POINT ( 'NONE',  ( -57.99999999999997868, 2.944486372867092250, 1.699999999999805667 ) ) ;
#3996 = CARTESIAN_POINT ( 'NONE',  ( -54.83155989232413674, 3.400000000000008349, -1.845326485282803322E-13 ) ) ;
#3997 = CARTESIAN_POINT ( 'NONE',  ( 51.80000000000002558, 4.175664755576631748, 1.929721184273780255 ) ) ;
#3998 = CARTESIAN_POINT ( 'NONE',  ( -57.45655989232412253, -3.399999999999991029, -2.148039047887444390E-13 ) ) ;
#3999 = CARTESIAN_POINT ( 'NONE',  ( 58.50000000000001421, 0.8000000000000000444, 2.421260002560650104 ) ) ;
#4000 = ADVANCED_FACE ( 'NONE', ( #9859 ), #30502, .T. ) ;
#4002 = DIRECTION ( 'NONE',  ( 1.000000000000000000, 1.047444401652940007E-14, 0.000000000000000000 ) ) ;
#4001 = CARTESIAN_POINT ( 'NONE',  ( -59.09999999999997300, 2.465712773623992327, -0.9709585562669131864 ) ) ;
#4003 = EDGE_CURVE ( 'NONE', #8546, #4409, #24941, .T. ) ;
#4004 = TOROIDAL_SURFACE ( 'NONE', #29791, 4.600000000000000533, 0.4999999999999996669 ) ;
#4005 = ADVANCED_FACE ( 'NONE', ( #26802 ), #29626, .F. ) ;
#4006 = DIRECTION ( 'NONE',  ( -1.040834085586084257E-14, 0.000000000000000000, -1.000000000000000000 ) ) ;
#4007 = CARTESIAN_POINT ( 'NONE',  ( 47.00000000000002132, -1.426739617975173013, 3.843750000000023093 ) ) ;
#4008 = CARTESIAN_POINT ( 'NONE',  ( 58.65000000000004121, -1.671477153793431647, -0.8495817349405304642 ) ) ;
#4010 = CIRCLE ( 'NONE', #21746, 0.7500000000000002220 ) ;
#4009 = CARTESIAN_POINT ( 'NONE',  ( -73.84999999999996589, -2.420255095024673698E-15, 4.597676519392165349E-15 ) ) ;
#4011 = DIRECTION ( 'NONE',  ( 3.167104333282667910E-32, -1.224646799147353207E-16, 1.000000000000000000 ) ) ;
#4012 = ORIENTED_EDGE ( 'NONE', *, *, #1082, .T. ) ;
#4014 = DIRECTION ( 'NONE',  ( 1.000000000000000000, -0.000000000000000000, -1.047444401652940007E-14 ) ) ;
#4013 = CARTESIAN_POINT ( 'NONE',  ( 58.50000000000001421, -0.8000000000000000444, -2.421260002560650104 ) ) ;
#4015 = AXIS2_PLACEMENT_3D ( 'NONE', #27264, #14906, #5582 ) ;
#4016 = ORIENTED_EDGE ( 'NONE', *, *, #22796, .F. ) ;
#4017 = FILL_AREA_STYLE_COLOUR ( '', #28031 ) ;
#4018 = CARTESIAN_POINT ( 'NONE',  ( -60.48535533905928219, 1.968299342331293196E-15, 6.674684237050104391E-16 ) ) ;
#4020 = CARTESIAN_POINT ( 'NONE',  ( 56.95349779155813508, 0.7404564066163630276, -2.492333105726597164 ) ) ;
#4019 = CARTESIAN_POINT ( 'NONE',  ( -59.06249999999995737, -1.962990915244707368, -3.400000000000216627 ) ) ;
#4021 = ORIENTED_EDGE ( 'NONE', *, *, #26922, .T. ) ;
#4022 = ORIENTED_EDGE ( 'NONE', *, *, #17072, .T. ) ;
#4023 = LINE ( 'NONE', #1789, #763 ) ;
#4024 = ORIENTED_EDGE ( 'NONE', *, *, #30577, .T. ) ;
#4025 = AXIS2_PLACEMENT_3D ( 'NONE', #13563, #15794, #28134 ) ;
#4026 = CARTESIAN_POINT ( 'NONE',  ( 58.66122797211809825, -1.632010475557796214, 0.9232791089888466862 ) ) ;
#4027 = PLANE ( 'NONE',  #23546 ) ;
#4028 = VERTEX_POINT ( 'NONE', #8563 ) ;
#4029 = PLANE ( 'NONE',  #20658 ) ;
#4030 = CARTESIAN_POINT ( 'NONE',  ( -54.39999999999999147, -1.500000000000006661, 3.959797974644449603 ) ) ;
#4031 = EDGE_CURVE ( 'NONE', #22261, #28405, #29006, .T. ) ;
#4032 = ORIENTED_EDGE ( 'NONE', *, *, #6839, .F. ) ;
#4033 = ORIENTED_EDGE ( 'NONE', *, *, #4819, .T. ) ;
#4034 = LINE ( 'NONE', #29999, #8663 ) ;
#4035 = EDGE_CURVE ( 'NONE', #29251, #7998, #6739, .T. ) ;
#4036 =( BOUNDED_SURFACE ( )  B_SPLINE_SURFACE ( 3, 2, ( 
 ( #6147, #15488, #25146 ),
 ( #12944, #3611, #1081 ),
 ( #3466, #30207, #934 ),
 ( #22638, #10731, #10586 ) ),
 .UNSPECIFIED., .F., .F., .F. ) 
 B_SPLINE_SURFACE_WITH_KNOTS ( ( 4, 4 ),
 ( 3, 3 ),
 ( 1.982313172862383066, 2.241731514487931065 ),
 ( 0.000000000000000000, 1.000000000000000000 ),
 .UNSPECIFIED. ) 
 GEOMETRIC_REPRESENTATION_ITEM ( )  RATIONAL_B_SPLINE_SURFACE ( (
 ( 1.000000000000000000, 0.8156258140602881124, 1.000000000000000000),
 ( 1.000000000000000000, 0.8356979842195455532, 1.000000000000000000),
 ( 1.000000000000000000, 0.8538860448759181265, 1.000000000000000000),
 ( 1.000000000000000000, 0.8699658093904938383, 1.000000000000000000) ) ) 
 REPRESENTATION_ITEM ( '' )  SURFACE ( )  );
#4037 = CARTESIAN_POINT ( 'NONE',  ( 51.45655683570191741, -0.9591657938390827365, -1.468576096419532018 ) ) ;
#4038 = CARTESIAN_POINT ( 'NONE',  ( -54.65835481156722864, -0.7533615035078032873, 3.673546848079177973 ) ) ;
#4039 = DIRECTION ( 'NONE',  ( 1.000000000000000000, 0.000000000000000000, -3.491481338843133355E-15 ) ) ;
#4040 = PRODUCT_DEFINITION_FORMATION_WITH_SPECIFIED_SOURCE ( 'ANY', '', #15367, .NOT_KNOWN. ) ;
#4041 = CARTESIAN_POINT ( 'NONE',  ( 15.59140265158955962, 2.334862116274945887, 4.877703086529577625 ) ) ;
#4042 = CIRCLE ( 'NONE', #19235, 0.05000000000000012768 ) ;
#4043 = CARTESIAN_POINT ( 'NONE',  ( 50.40000000000001990, 1.409787217987196861, -3.950000000000022826 ) ) ;
#4044 = CIRCLE ( 'NONE', #5043, 4.375000000000000000 ) ;
#4045 = CARTESIAN_POINT ( 'NONE',  ( 57.02678890911435872, 0.7442859487862443224, -1.783438914669892128 ) ) ;
#4047 = CARTESIAN_POINT ( 'NONE',  ( -35.85663232820584057, 4.804073783693455724, -2.042134687550314354 ) ) ;
#4046 = CARTESIAN_POINT ( 'NONE',  ( -36.25997906085271438, -2.880023619481960839, 4.335093843541793390 ) ) ;
#4048 = AXIS2_PLACEMENT_3D ( 'NONE', #16712, #31091, #18769 ) ;
#4049 = CARTESIAN_POINT ( 'NONE',  ( 51.78962428791817274, -4.157296476791675133, 1.048491968755490555 ) ) ;
#4050 = DIRECTION ( 'NONE',  ( 0.000000000000000000, -0.9996898646859343485, -0.02490330187381123786 ) ) ;
#4051 = CARTESIAN_POINT ( 'NONE',  ( 57.05000000000001847, 0.8000000000000002665, -2.421260002560650104 ) ) ;
#4052 = CARTESIAN_POINT ( 'NONE',  ( 51.39880079787599243, -0.9985449105385801882, 1.587650281084739712 ) ) ;
#4053 = ORIENTED_EDGE ( 'NONE', *, *, #15994, .T. ) ;
#4054 = EDGE_LOOP ( 'NONE', ( #4675, #20937, #29221, #22519 ) ) ;
#4055 = FACE_OUTER_BOUND ( 'NONE', #31072, .T. ) ;
#4056 = VERTEX_POINT ( 'NONE', #13006 ) ;
#4057 = CARTESIAN_POINT ( 'NONE',  ( 52.61915120152473690, 4.492597126270304386, 2.049999999999816414 ) ) ;
#4058 = CARTESIAN_POINT ( 'NONE',  ( -59.40835481156722864, 4.108500314926515351, -1.367561758111407455 ) ) ;
#4060 = CARTESIAN_POINT ( 'NONE',  ( -36.48174642953001978, 3.496282614933940991, 4.130238739723520958 ) ) ;
#4059 = CARTESIAN_POINT ( 'NONE',  ( 15.03925126672132784, 4.945493884734818657, -1.606888370749675499 ) ) ;
#4061 = ORIENTED_EDGE ( 'NONE', *, *, #28959, .T. ) ;
#4062 = ORIENTED_EDGE ( 'NONE', *, *, #9263, .T. ) ;
#4063 = DIRECTION ( 'NONE',  ( 0.000000000000000000, -0.2008964009354152203, 0.9796124928211138450 ) ) ;
#4064 = VERTEX_POINT ( 'NONE', #20627 ) ;
#4065 = CARTESIAN_POINT ( 'NONE',  ( 58.99999999999999289, 4.286263797015737088E-16, -3.000000000000618172 ) ) ;
#4066 = ORIENTED_EDGE ( 'NONE', *, *, #12586, .F. ) ;
#4068 = DIRECTION ( 'NONE',  ( -2.459562394685755126E-16, 0.9510565162951566398, -0.3090169943749383474 ) ) ;
#4067 = DIRECTION ( 'NONE',  ( 1.000000000000000000, -1.219044193948984088E-29, 3.491481338843133750E-15 ) ) ;
#4069 = CARTESIAN_POINT ( 'NONE',  ( 58.75000000000002132, 6.153735859711025284E-13, 3.111507638930570854E-58 ) ) ;
#4070 = ORIENTED_EDGE ( 'NONE', *, *, #8587, .F. ) ;
#4071 = DIRECTION ( 'NONE',  ( 0.000000000000000000, 0.9996898646859343485, 0.02490330187381123786 ) ) ;
#4072 = EDGE_CURVE ( 'NONE', #7915, #17824, #24438, .T. ) ;
#4073 = CARTESIAN_POINT ( 'NONE',  ( 58.65000045311409593, 1.830940512617971194, -0.4044292957139257183 ) ) ;
#4074 = VECTOR ( 'NONE', #19323, 1000.000000000000000 ) ;
#4075 = EDGE_CURVE ( 'NONE', #25905, #30422, #3127, .T. ) ;
#4076 = FILL_AREA_STYLE ('',( #18495 ) ) ;
#4077 = CARTESIAN_POINT ( 'NONE',  ( -35.85663232820584057, -2.686240680702151717, -4.475885388010727439 ) ) ;
#4078 = ADVANCED_FACE ( 'NONE', ( #30257 ), #23152, .T. ) ;
#4079 = CARTESIAN_POINT ( 'NONE',  ( -57.57202994616204705, -4.156921938165296204, -2.193920212522006445E-13 ) ) ;
#4080 = CARTESIAN_POINT ( 'NONE',  ( 47.00000000000002132, -3.726179070414207928, 1.710435481158852244 ) ) ;
#4081 = CARTESIAN_POINT ( 'NONE',  ( -59.29792740578359656, -2.256877952708279178, 2.542931754211911421 ) ) ;
#4082 = EDGE_CURVE ( 'NONE', #23319, #247, #678, .T. ) ;
#4083 = CARTESIAN_POINT ( 'NONE',  ( 61.00000000000001421, 1.000000000000639044, -1.586072192556190474 ) ) ;
#4084 = AXIS2_PLACEMENT_3D ( 'NONE', #24707, #26781, #4926 ) ;
#4085 = LINE ( 'NONE', #4234, #28127 ) ;
#4087 = CIRCLE ( 'NONE', #17757, 0.1000000000000000472 ) ;
#4086 = CARTESIAN_POINT ( 'NONE',  ( -36.58413561666693425, -0.1030603059131488530, 5.407440145940149989 ) ) ;
#4088 = CARTESIAN_POINT ( 'NONE',  ( 48.40134283869316789, 0.9106118309513187015, -3.923752762110599424 ) ) ;
#4089 = VERTEX_POINT ( 'NONE', #13293 ) ;
#4090 = CARTESIAN_POINT ( 'NONE',  ( -56.99999999999997158, -2.944486372867094470, 1.699999999999777689 ) ) ;
#4091 = EDGE_LOOP ( 'NONE', ( #15490, #29293 ) ) ;
#4092 = DIRECTION ( 'NONE',  ( 0.9990609829735203062, 0.04332611568077059105, -3.480798531547777782E-15 ) ) ;
#4093 = PRODUCT_RELATED_PRODUCT_CATEGORY ( 'part', '', ( #10308 ) ) ;
#4095 = CARTESIAN_POINT ( 'NONE',  ( 58.65263613458535019, -1.277852321299179916, 1.372222488448882727 ) ) ;
#4094 = DIRECTION ( 'NONE',  ( 0.000000000000000000, 0.9783524716138816135, -0.2069455031814148027 ) ) ;
#4096 = EDGE_LOOP ( 'NONE', ( #14308, #18177, #562, #6679 ) ) ;
#4097 = VERTEX_POINT ( 'NONE', #22985 ) ;
#4098 = CARTESIAN_POINT ( 'NONE',  ( -59.67987798884426809, -2.349476376206443007, -1.226921160904901109 ) ) ;
#4099 = PLANE ( 'NONE',  #10991 ) ;
#4101 = DIRECTION ( 'NONE',  ( -1.000000000000000000, -0.000000000000000000, 3.491481338843133355E-15 ) ) ;
#4100 = CARTESIAN_POINT ( 'NONE',  ( -60.75952994616205416, -4.643455692769856999E-15, 3.599999999999783373 ) ) ;
#4102 = ORIENTED_EDGE ( 'NONE', *, *, #19010, .F. ) ;
#4103 = CARTESIAN_POINT ( 'NONE',  ( -60.61042740578359656, -2.936324665650201560, -2.606018187048497303 ) ) ;
#4104 = DIRECTION ( 'NONE',  ( -3.489354422748178582E-15, 1.218509414717996338E-16, -1.000000000000000000 ) ) ;
#4105 = TOROIDAL_SURFACE ( 'NONE', #8156, 1.949999999999999956, 0.05000000000000000278 ) ;
#4106 = EDGE_CURVE ( 'NONE', #26655, #23063, #26472, .T. ) ;
#4107 = CARTESIAN_POINT ( 'NONE',  ( -61.39959699979583263, -2.624557268248721265, -0.6337974637291527991 ) ) ;
#4108 = DIRECTION ( 'NONE',  ( 1.000000000000000000, -1.219044193948983948E-29, 3.491481338843133355E-15 ) ) ;
#4109 = DIRECTION ( 'NONE',  ( 0.000000000000000000, 0.000000000000000000, 1.000000000000000000 ) ) ;
#4110 = ORIENTED_EDGE ( 'NONE', *, *, #24246, .F. ) ;
#4111 = CARTESIAN_POINT ( 'NONE',  ( 57.04037853559506743, -0.7490840064628494499, 1.779165039991060571 ) ) ;
#4112 = CARTESIAN_POINT ( 'NONE',  ( 61.23770293222991512, 0.8897917884447287262, -1.791164585742097914 ) ) ;
#4113 = CARTESIAN_POINT ( 'NONE',  ( -59.40362242792826919, 3.375967812128700452, 1.250136525132546916 ) ) ;
#4114 = DIRECTION ( 'NONE',  ( -1.000000000000000000, 0.000000000000000000, 1.047444401652940007E-14 ) ) ;
#4115 = CARTESIAN_POINT ( 'NONE',  ( 50.80000000000002558, -4.387164041431067751, 1.383037119376580693 ) ) ;
#4116 = EDGE_CURVE ( 'NONE', #3567, #26982, #21429, .T. ) ;
#4117 = VECTOR ( 'NONE', #4940, 1000.000000000000000 ) ;
#4119 = DIRECTION ( 'NONE',  ( 0.000000000000000000, 0.000000000000000000, -1.000000000000000000 ) ) ;
#4118 = CARTESIAN_POINT ( 'NONE',  ( -55.09585481156724285, -1.184343223768585807, -3.558065644182726306 ) ) ;
#4120 = CARTESIAN_POINT ( 'NONE',  ( -62.09999999999998010, -2.729213130609289717, -0.3426631772468137771 ) ) ;
#4122 = CARTESIAN_POINT ( 'NONE',  ( -59.60996874016036173, 2.024041967860128910, 1.710882463691307143 ) ) ;
#4121 = CARTESIAN_POINT ( 'NONE',  ( -44.59999999999998010, 2.650000000000008349, -1.759412204284508433E-13 ) ) ;
#4123 = VERTEX_POINT ( 'NONE', #12833 ) ;
#4124 = AXIS2_PLACEMENT_3D ( 'NONE', #22932, #4223, #27679 ) ;
#4125 = DIRECTION ( 'NONE',  ( 1.000000000000000000, 0.000000000000000000, 0.000000000000000000 ) ) ;
#4126 = DIRECTION ( 'NONE',  ( 0.000000000000000000, 0.000000000000000000, 1.000000000000000000 ) ) ;
#4128 = CARTESIAN_POINT ( 'NONE',  ( -36.31414349454749413, 4.963067629822528026, 1.552801941062302182 ) ) ;
#4127 = CARTESIAN_POINT ( 'NONE',  ( 48.30000000000001847, 2.428612866367529932E-14, 0.000000000000000000 ) ) ;
#4129 = CARTESIAN_POINT ( 'NONE',  ( 15.57907767661756182, -5.286410563980378008, 1.167394352644079092 ) ) ;
#4130 = ORIENTED_EDGE ( 'NONE', *, *, #25940, .T. ) ;
#4131 = EDGE_CURVE ( 'NONE', #30566, #16027, #1685, .T. ) ;
#4132 = ORIENTED_EDGE ( 'NONE', *, *, #25476, .F. ) ;
#4133 = CARTESIAN_POINT ( 'NONE',  ( -77.28999999999996362, -0.4398635404618146394, -0.01095745282447164494 ) ) ;
#4134 = CARTESIAN_POINT ( 'NONE',  ( 52.06628335902946247, -0.5434431642975677823, -1.996089927833914146 ) ) ;
#4135 = ORIENTED_EDGE ( 'NONE', *, *, #26385, .T. ) ;
#4136 = DIRECTION ( 'NONE',  ( -0.9993908270190957621, 0.03489949670250100389, 3.491481338843133355E-15 ) ) ;
#4137 = VERTEX_POINT ( 'NONE', #818 ) ;
#4138 = DIRECTION ( 'NONE',  ( 2.616380615828677096E-15, -0.2069455031823360380, -0.9783524716136868804 ) ) ;
#4139 = ORIENTED_EDGE ( 'NONE', *, *, #30205, .F. ) ;
#4140 = SURFACE_STYLE_FILL_AREA ( #20938 ) ;
#4141 = CARTESIAN_POINT ( 'NONE',  ( -55.25952994616203995, -3.117691453623963049, -1.800000000000208544 ) ) ;
#4142 = EDGE_CURVE ( 'NONE', #13465, #11082, #28489, .T. ) ;
#4143 = CARTESIAN_POINT ( 'NONE',  ( -58.76905989232410832, 2.023778652682509368E-14, -3.400000000000208189 ) ) ;
#4144 = ORIENTED_EDGE ( 'NONE', *, *, #18455, .F. ) ;
#4145 = EDGE_LOOP ( 'NONE', ( #29364, #13838, #21005, #17635, #3854 ) ) ;
#4146 = CIRCLE ( 'NONE', #21873, 2.649999999999999911 ) ;
#4147 = ORIENTED_EDGE ( 'NONE', *, *, #21499, .F. ) ;
#4148 = CARTESIAN_POINT ( 'NONE',  ( -55.82202994616203995, 2.078460969082674747, -3.600000000000189715 ) ) ;
#4149 = CARTESIAN_POINT ( 'NONE',  ( 58.45000000000001705, -0.7500000000000000000, -2.421260002560649660 ) ) ;
#4150 = DIRECTION ( 'NONE',  ( 1.000000000000000000, 0.000000000000000000, 0.000000000000000000 ) ) ;
#4151 = FACE_OUTER_BOUND ( 'NONE', #15246, .T. ) ;
#4152 = CARTESIAN_POINT ( 'NONE',  ( 47.05963571244991783, 8.266527678078146479, 1.949999999999835865 ) ) ;
#4153 = EDGE_CURVE ( 'NONE', #26067, #3458, #8707, .T. ) ;
#4154 =( BOUNDED_CURVE ( )  B_SPLINE_CURVE ( 2, ( #7300, #14267, #4287, #26616, #16969, #2561, #1928, #16491, #28690 ),
 .UNSPECIFIED., .F., .T. ) 
 B_SPLINE_CURVE_WITH_KNOTS ( ( 3, 2, 2, 2, 3 ),
 ( 0.2500000000000000000, 0.2592592592592592449, 0.2777777777777777901, 0.2962962962962962798, 0.3055555555555555802 ),
 .UNSPECIFIED. ) 
 CURVE ( )  GEOMETRIC_REPRESENTATION_ITEM ( )  RATIONAL_B_SPLINE_CURVE ( ( 0.9330127018922192983, 0.9330127018922194093, 1.000000000000000000, 0.8660254037844387076, 1.000000000000000000, 0.8660254037844387076, 1.000000000000000000, 0.9330127018922191873, 0.9330127018922194093 ) ) 
 REPRESENTATION_ITEM ( '' )  );
#4156 = PLANE ( 'NONE',  #30583 ) ;
#4155 = DIRECTION ( 'NONE',  ( -9.754918421198724481E-16, -0.9601771338024399638, -0.2793919678926571892 ) ) ;
#4157 = CYLINDRICAL_SURFACE ( 'NONE', #3840, 0.1000000000000000472 ) ;
#4158 = CARTESIAN_POINT ( 'NONE',  ( 69.25000000000004263, -0.4500000000000000111, 1.988246715072632620 ) ) ;
#4159 = CARTESIAN_POINT ( 'NONE',  ( 57.05000000000001847, 0.8156862745098039102, -2.468735688885368873 ) ) ;
#4160 = CARTESIAN_POINT ( 'NONE',  ( -62.09999999999997300, -2.737158043526071172, 0.2654540351181889912 ) ) ;
#4161 = ORIENTED_EDGE ( 'NONE', *, *, #27382, .T. ) ;
#4163 = CARTESIAN_POINT ( 'NONE',  ( 50.39869454013827976, -0.9107929593199907137, 3.923749358243191043 ) ) ;
#4162 = CARTESIAN_POINT ( 'NONE',  ( 48.30000000000001847, 0.6462379109120995890, -4.048750000000023164 ) ) ;
#4164 = EDGE_CURVE ( 'NONE', #1808, #1734, #22433, .T. ) ;
#4165 = CARTESIAN_POINT ( 'NONE',  ( 51.45655683570191741, -0.9591657938390835136, -1.468576096419531574 ) ) ;
#4166 = ORIENTED_EDGE ( 'NONE', *, *, #30155, .F. ) ;
#4167 = DIRECTION ( 'NONE',  ( 1.000000000000000000, 3.054025858079668409E-16, -2.042474015755241579E-16 ) ) ;
#4168 = CARTESIAN_POINT ( 'NONE',  ( -55.75952994616203995, 3.117691453623994580, -1.800000000000184563 ) ) ;
#4169 = ORIENTED_EDGE ( 'NONE', *, *, #22608, .T. ) ;
#4170 = ORIENTED_EDGE ( 'NONE', *, *, #6103, .F. ) ;
#4171 = FACE_OUTER_BOUND ( 'NONE', #19072, .T. ) ;
#4172 = VERTEX_POINT ( 'NONE', #27415 ) ;
#4173 = CARTESIAN_POINT ( 'NONE',  ( 51.13858604272871133, 1.070913481529462086, -1.222302725805713308 ) ) ;
#4174 = ADVANCED_FACE ( 'NONE', ( #985 ), #10638, .T. ) ;
#4175 = CARTESIAN_POINT ( 'NONE',  ( 64.95000000000001705, 1.401298464324817071E-42, -6.803151388735846952E-13 ) ) ;
#4176 = VERTEX_POINT ( 'NONE', #26298 ) ;
#4177 = AXIS2_PLACEMENT_3D ( 'NONE', #4133, #26874, #19622 ) ;
#4178 = LINE ( 'NONE', #13816, #20768 ) ;
#4179 = EDGE_CURVE ( 'NONE', #7044, #17335, #18893, .T. ) ;
#4180 = CARTESIAN_POINT ( 'NONE',  ( -54.47064643025908737, -2.407416487588556198, -2.678616765879081374 ) ) ;
#4181 = ORIENTED_EDGE ( 'NONE', *, *, #1277, .F. ) ;
#4182 = VERTEX_POINT ( 'NONE', #6663 ) ;
#4183 = DIRECTION ( 'NONE',  ( 3.002035892788117459E-16, -0.9996898646859343485, -0.02490330187381124133 ) ) ;
#4184 = CARTESIAN_POINT ( 'NONE',  ( -67.91948434493399134, -6.091656077594763675E-16, 3.386362506249485869E-15 ) ) ;
#4185 = CARTESIAN_POINT ( 'NONE',  ( -54.90835481156724285, 4.108500314926515351, -1.367561758111408565 ) ) ;
#4186 = ORIENTED_EDGE ( 'NONE', *, *, #4570, .F. ) ;
#4187 = FACE_OUTER_BOUND ( 'NONE', #22497, .T. ) ;
#4188 = CARTESIAN_POINT ( 'NONE',  ( 16.10660252424456473, 3.410993390446818374, 4.205682099886888459 ) ) ;
#4189 = ADVANCED_FACE ( 'NONE', ( #11733 ), #22935, .T. ) ;
#4190 = DIRECTION ( 'NONE',  ( 1.000000000000000000, 0.000000000000000000, 0.000000000000000000 ) ) ;
#4191 = CARTESIAN_POINT ( 'NONE',  ( 57.04767748491563140, 0.7500000000000049960, -1.778341924377874639 ) ) ;
#4193 = CARTESIAN_POINT ( 'NONE',  ( 58.74999999305997278, -0.9423072185570646742, 1.683452862813170636 ) ) ;
#4192 = CARTESIAN_POINT ( 'NONE',  ( -35.98952425903311791, -2.686240675664594235, 4.475885398016349548 ) ) ;
#4194 = DIRECTION ( 'NONE',  ( 0.000000000000000000, -1.000000000000000000, -0.000000000000000000 ) ) ;
#4195 = DIRECTION ( 'NONE',  ( 0.000000000000000000, 0.000000000000000000, 1.000000000000000000 ) ) ;
#4196 = DIRECTION ( 'NONE',  ( 3.489354422748178582E-15, -1.218509414717996338E-16, 1.000000000000000000 ) ) ;
#4197 = CARTESIAN_POINT ( 'NONE',  ( 54.50000000000002132, -0.003244837758135472351, 4.274998768541100169 ) ) ;
#4198 = CIRCLE ( 'NONE', #26470, 4.375000000000000000 ) ;
#4199 = VERTEX_POINT ( 'NONE', #23620 ) ;
#4200 = EDGE_CURVE ( 'NONE', #8754, #8529, #16324, .T. ) ;
#4201 = EDGE_LOOP ( 'NONE', ( #3773, #1603, #18562, #21804 ) ) ;
#4202 = ORIENTED_EDGE ( 'NONE', *, *, #18602, .F. ) ;
#4203 = CARTESIAN_POINT ( 'NONE',  ( 50.93131983953347941, -3.937842567657669157, 1.145831922971412675 ) ) ;
#4204 = VERTEX_POINT ( 'NONE', #28201 ) ;
#4205 = ADVANCED_FACE ( 'NONE', ( #16003 ), #11245, .F. ) ;
#4206 = CARTESIAN_POINT ( 'NONE',  ( 51.74548155811471162, 3.822334312940638412, 2.049999999999816414 ) ) ;
#4207 = CARTESIAN_POINT ( 'NONE',  ( -56.40835481156723574, 4.108500314926515351, -1.367561758111408343 ) ) ;
#4209 = CARTESIAN_POINT ( 'NONE',  ( -36.23324115033521764, 2.840672495176659318, 4.363684107482471930 ) ) ;
#4208 = DIRECTION ( 'NONE',  ( 0.000000000000000000, -1.000000000000000000, 0.000000000000000000 ) ) ;
#4210 = ORIENTED_EDGE ( 'NONE', *, *, #23209, .T. ) ;
#4211 = FACE_OUTER_BOUND ( 'NONE', #7307, .T. ) ;
#4212 = ORIENTED_EDGE ( 'NONE', *, *, #29857, .F. ) ;
#4213 = DIRECTION ( 'NONE',  ( 1.000000000000000000, -1.219044193948983948E-29, 3.491481338843133355E-15 ) ) ;
#4214 = ORIENTED_EDGE ( 'NONE', *, *, #17708, .T. ) ;
#4216 = CARTESIAN_POINT ( 'NONE',  ( -60.49999999999997868, 1.656632322739229403E-15, 1.870925083934595927E-15 ) ) ;
#4215 = DIRECTION ( 'NONE',  ( 0.000000000000000000, 0.9996898646859344595, 0.02490330187381124480 ) ) ;
#4217 = EDGE_CURVE ( 'NONE', #5230, #29912, #9561, .T. ) ;
#4218 = ORIENTED_EDGE ( 'NONE', *, *, #2634, .T. ) ;
#4219 = CARTESIAN_POINT ( 'NONE',  ( 57.05000000000001137, -0.7794871794871797155, 1.732743413496401930 ) ) ;
#4220 = ADVANCED_FACE ( 'NONE', ( #13762 ), #4276, .T. ) ;
#4221 = CARTESIAN_POINT ( 'NONE',  ( 58.75000018803716273, 1.882836145343370404, -0.4533061784665026739 ) ) ;
#4222 = CARTESIAN_POINT ( 'NONE',  ( -59.41132486539680713, 3.361433066165957051, 1.250136525132557574 ) ) ;
#4223 = DIRECTION ( 'NONE',  ( -1.520093157366847861E-16, 0.5877852522924624790, 0.8090169943749551118 ) ) ;
#4225 = CARTESIAN_POINT ( 'NONE',  ( -56.25952994616206126, -4.643455692769913008E-15, 3.599999999999798916 ) ) ;
#4224 = VECTOR ( 'NONE', #16333, 1000.000000000000000 ) ;
#4226 = CARTESIAN_POINT ( 'NONE',  ( 51.84429591523409897, 0.2531794267987216851, 4.351658421183466352 ) ) ;
#4227 = CARTESIAN_POINT ( 'NONE',  ( 50.59602332238209499, 0.1408342061609074158, -1.212874140286673841 ) ) ;
#4228 = CARTESIAN_POINT ( 'NONE',  ( 50.38476904405314372, 1.115727354199254950, -3.895947837398489266 ) ) ;
#4229 = CARTESIAN_POINT ( 'NONE',  ( -57.36042740578360366, 3.725040285533373741, -1.239922660687670763 ) ) ;
#4230 = DIRECTION ( 'NONE',  ( -1.040834085586084257E-14, 0.000000000000000000, -1.000000000000000000 ) ) ;
#4231 = EDGE_LOOP ( 'NONE', ( #5289, #23761, #22530, #22067 ) ) ;
#4232 = LINE ( 'NONE', #13149, #7429 ) ;
#4233 = ADVANCED_FACE ( 'NONE', ( #19023 ), #4447, .F. ) ;
#4234 = CARTESIAN_POINT ( 'NONE',  ( 34.56702326949724835, 8.213851659285209550, -2.050000000000119726 ) ) ;
#4235 = CARTESIAN_POINT ( 'NONE',  ( -36.68133364217572989, 0.7247683022688486965, 5.358970532132285136 ) ) ;
#4236 = DIRECTION ( 'NONE',  ( 0.000000000000000000, 0.000000000000000000, 1.000000000000000000 ) ) ;
#4237 = EDGE_CURVE ( 'NONE', #10792, #4826, #31036, .T. ) ;
#4238 = ORIENTED_EDGE ( 'NONE', *, *, #17518, .T. ) ;
#4239 = LINE ( 'NONE', #23575, #6737 ) ;
#4240 = ORIENTED_EDGE ( 'NONE', *, *, #31187, .F. ) ;
#4241 = CARTESIAN_POINT ( 'NONE',  ( 51.87416143049284756, 8.598705507415683513, 1.949999999999818767 ) ) ;
#4242 = AXIS2_PLACEMENT_3D ( 'NONE', #7911, #5853, #25324 ) ;
#4243 = CARTESIAN_POINT ( 'NONE',  ( 58.65844932252372246, 0.9660788770032745498, -1.607045716458365581 ) ) ;
#4244 = ORIENTED_EDGE ( 'NONE', *, *, #27945, .T. ) ;
#4245 = ORIENTED_EDGE ( 'NONE', *, *, #28550, .T. ) ;
#4246 = DIRECTION ( 'NONE',  ( 0.000000000000000000, 0.000000000000000000, 1.000000000000000000 ) ) ;
#4247 = DIRECTION ( 'NONE',  ( 2.475188721679744024E-12, -0.7438053426811914726, -0.6683962987621305807 ) ) ;
#4249 = CARTESIAN_POINT ( 'NONE',  ( 61.05455829109366306, 0.5997039666881081033, -1.862468256791881327 ) ) ;
#4248 = DIRECTION ( 'NONE',  ( 0.000000000000000000, 0.000000000000000000, 1.000000000000000000 ) ) ;
#4250 = ORIENTED_EDGE ( 'NONE', *, *, #944, .F. ) ;
#4251 = CARTESIAN_POINT ( 'NONE',  ( -60.17292740578359656, 1.073804522883521351, 3.225979517392337126 ) ) ;
#4252 = CIRCLE ( 'NONE', #14870, 0.1500000000000001887 ) ;
#4253 = DIRECTION ( 'NONE',  ( -0.9993908270190957621, 0.03489949670250094838, 3.492791461889839594E-15 ) ) ;
#4254 = SHAPE_DEFINITION_REPRESENTATION ( #29783, #16755 ) ;
#4255 = CARTESIAN_POINT ( 'NONE',  ( -61.34999999999997300, -2.583824419212624957, -0.5885162450438690129 ) ) ;
#4256 = CARTESIAN_POINT ( 'NONE',  ( -62.34999999999997300, 2.749147127886321318, 0.06848408015298348972 ) ) ;
#4257 = DIRECTION ( 'NONE',  ( -1.000000000000000000, -0.000000000000000000, 3.491481338843133750E-15 ) ) ;
#4258 = ORIENTED_EDGE ( 'NONE', *, *, #12404, .T. ) ;
#4259 = AXIS2_PLACEMENT_3D ( 'NONE', #600, #29562, #12939 ) ;
#4260 = CARTESIAN_POINT ( 'NONE',  ( 15.03925126672132961, -2.686240680702165928, 4.475885388010711452 ) ) ;
#4261 = APPLICATION_CONTEXT ( 'automotive_design' ) ;
#4262 = CARTESIAN_POINT ( 'NONE',  ( -36.11122220296831387, 2.734418404389770796, -4.440882220947520054 ) ) ;
#4263 = DIRECTION ( 'NONE',  ( 1.000000000000000000, 0.000000000000000000, -1.047444401652940007E-14 ) ) ;
#4264 = AXIS2_PLACEMENT_3D ( 'NONE', #13850, #30821, #1527 ) ;
#4265 = DIRECTION ( 'NONE',  ( 0.000000000000000000, -1.000000000000000000, 0.000000000000000000 ) ) ;
#4266 = CARTESIAN_POINT ( 'NONE',  ( 15.90468948301722918, 0.6818242347930796310, -5.365311767243446717 ) ) ;
#4268 = CARTESIAN_POINT ( 'NONE',  ( 58.73371041428929118, -1.788808215311387118, -0.5624054559931295216 ) ) ;
#4267 = DIRECTION ( 'NONE',  ( 0.000000000000000000, -1.000000000000000000, 0.000000000000000000 ) ) ;
#4269 = CARTESIAN_POINT ( 'NONE',  ( 51.80000048712015115, 3.919471099442191520, -2.045252491637605807 ) ) ;
#4271 = CARTESIAN_POINT ( 'NONE',  ( -59.61691039550309767, 2.025699712120192064, 1.710375399846320255 ) ) ;
#4270 = CARTESIAN_POINT ( 'NONE',  ( -62.04999999999998295, -2.636465585633694264, 0.1493792525119592429 ) ) ;
#4272 = EDGE_CURVE ( 'NONE', #5179, #26160, #23549, .T. ) ;
#4273 = VERTEX_POINT ( 'NONE', #4599 ) ;
#4274 = CARTESIAN_POINT ( 'NONE',  ( -61.34999999999997300, -2.617575446388284099, 0.6620413751912884726 ) ) ;
#4275 = EDGE_CURVE ( 'NONE', #8161, #19631, #25664, .T. ) ;
#4276 = CYLINDRICAL_SURFACE ( 'NONE', #29248, 2.525000000000001243 ) ;
#4278 = CARTESIAN_POINT ( 'NONE',  ( -36.89017861347081606, 5.235729994560179179, 1.359191621353925905 ) ) ;
#4277 = DIRECTION ( 'NONE',  ( -1.000000000000000000, -0.000000000000000000, -0.000000000000000000 ) ) ;
#4279 = DIRECTION ( 'NONE',  ( 1.000000000000000000, 3.054025858079668409E-16, -2.042474015755241579E-16 ) ) ;
#4280 = AXIS2_PLACEMENT_3D ( 'NONE', #9088, #28402, #28073 ) ;
#4281 = ORIENTED_EDGE ( 'NONE', *, *, #1624, .T. ) ;
#4282 = AXIS2_PLACEMENT_3D ( 'NONE', #10523, #8596, #8444 ) ;
#4283 = CARTESIAN_POINT ( 'NONE',  ( -36.42771574642760868, -4.977801270594346406, 2.126472881633285628 ) ) ;
#4284 = FACE_OUTER_BOUND ( 'NONE', #8959, .T. ) ;
#4285 = ORIENTED_EDGE ( 'NONE', *, *, #12706, .F. ) ;
#4286 = AXIS2_PLACEMENT_3D ( 'NONE', #29880, #30023, #745 ) ;
#4287 = CARTESIAN_POINT ( 'NONE',  ( -56.24999999999997158, -1.184343223768582032, -3.558065644182724974 ) ) ;
#4288 = ORIENTED_EDGE ( 'NONE', *, *, #3028, .F. ) ;
#4289 = CARTESIAN_POINT ( 'NONE',  ( 60.75000000000001421, 1.000000000000636380, -1.996089927833914146 ) ) ;
#4290 = VERTEX_POINT ( 'NONE', #14256 ) ;
#4291 = FILL_AREA_STYLE_COLOUR ( '', #31325 ) ;
#4292 = EDGE_CURVE ( 'NONE', #3728, #7731, #21180, .T. ) ;
#4293 = CARTESIAN_POINT ( 'NONE',  ( -57.39405989232411542, -2.944486372867076263, -1.700000000000214451 ) ) ;
#4294 = ORIENTED_EDGE ( 'NONE', *, *, #6688, .F. ) ;
#4295 = AXIS2_PLACEMENT_3D ( 'NONE', #16013, #10791, #11105 ) ;
#4296 = VERTEX_POINT ( 'NONE', #2218 ) ;
#4297 = EDGE_LOOP ( 'NONE', ( #27696, #15667, #12138, #14102 ) ) ;
#4298 = CARTESIAN_POINT ( 'NONE',  ( -56.00952994616203995, -3.117691453623963938, -1.800000000000210099 ) ) ;
#4299 = CARTESIAN_POINT ( 'NONE',  ( -67.99999999999995737, 0.5554785485864213168, -2.708628542650378890 ) ) ;
#4300 = CARTESIAN_POINT ( 'NONE',  ( -54.39999999999996305, -1.499999999999978906, -3.959797974644881258 ) ) ;
#4301 = DIRECTION ( 'NONE',  ( 1.000000000000000000, 1.047444401652940007E-14, 0.000000000000000000 ) ) ;
#4302 = CIRCLE ( 'NONE', #9383, 0.4576450603546999840 ) ;
#4303 = CARTESIAN_POINT ( 'NONE',  ( -60.85363833753338270, -2.450811742487699174, -0.9690170259278018117 ) ) ;
#4304 = AXIS2_PLACEMENT_3D ( 'NONE', #12089, #10484, #10314 ) ;
#4306 = FACE_OUTER_BOUND ( 'NONE', #17084, .T. ) ;
#4305 = CARTESIAN_POINT ( 'NONE',  ( -36.00197790576392265, 5.377732432866631385, -0.5657657256215206099 ) ) ;
#4307 = CARTESIAN_POINT ( 'NONE',  ( 57.05000000000001847, -0.8156862745098041323, -2.468735688885368873 ) ) ;
#4308 = DIRECTION ( 'NONE',  ( 1.000000000000000000, 2.586136946169074517E-16, -0.000000000000000000 ) ) ;
#4309 = AXIS2_PLACEMENT_3D ( 'NONE', #25885, #4039, #21640 ) ;
#4310 = CARTESIAN_POINT ( 'NONE',  ( -36.00201293083839715, -4.018128179617960427, -3.618665901676318075 ) ) ;
#4311 = ADVANCED_FACE ( 'NONE', ( #21563 ), #30733, .F. ) ;
#4312 = CARTESIAN_POINT ( 'NONE',  ( 58.72427158855725793, -1.646019958200114486, -0.8981388483283767599 ) ) ;
#4313 = DIRECTION ( 'NONE',  ( 1.000000000000000000, 0.000000000000000000, 0.000000000000000000 ) ) ;
#4314 = CIRCLE ( 'NONE', #15443, 4.000000000000000000 ) ;
#4315 = CARTESIAN_POINT ( 'NONE',  ( 50.97819963584588976, 8.730054137149846127, -1.950000000000177147 ) ) ;
#4316 = ORIENTED_EDGE ( 'NONE', *, *, #29166, .T. ) ;
#4318 = FACE_OUTER_BOUND ( 'NONE', #18719, .T. ) ;
#4317 = CARTESIAN_POINT ( 'NONE',  ( 54.04571512766927555, 5.333082506721908977, 2.049999999999811529 ) ) ;
#4319 = DIRECTION ( 'NONE',  ( 1.000000000000000000, -0.000000000000000000, -0.000000000000000000 ) ) ;
#4320 = ORIENTED_EDGE ( 'NONE', *, *, #19627, .T. ) ;
#4321 = CARTESIAN_POINT ( 'NONE',  ( -71.49999999999998579, -0.9743475445367636434, 4.751120590182405401 ) ) ;
#4322 = CARTESIAN_POINT ( 'NONE',  ( 61.02708519082499095, 0.5631634571416959112, -1.705199831323242821 ) ) ;
#4323 = CARTESIAN_POINT ( 'NONE',  ( -61.12499999999995737, 2.944486372867106905, -1.700000000000204459 ) ) ;
#4324 = ORIENTED_EDGE ( 'NONE', *, *, #23356, .T. ) ;
#4325 = ORIENTED_EDGE ( 'NONE', *, *, #20002, .F. ) ;
#4326 = VECTOR ( 'NONE', #22014, 1000.000000000000000 ) ;
#4327 = CARTESIAN_POINT ( 'NONE',  ( 15.49676243306308088, 4.927920137446221815, 1.660974799722156892 ) ) ;
#4328 = ORIENTED_EDGE ( 'NONE', *, *, #21675, .T. ) ;
#4329 = AXIS2_PLACEMENT_3D ( 'NONE', #28499, #21246, #18542 ) ;
#4330 = CARTESIAN_POINT ( 'NONE',  ( 51.31802667458094902, 1.005866567097610575, -1.281163073955430720 ) ) ;
#4331 = EDGE_CURVE ( 'NONE', #6201, #31046, #3467, .T. ) ;
#4332 = FACE_OUTER_BOUND ( 'NONE', #1938, .T. ) ;
#4333 = ORIENTED_EDGE ( 'NONE', *, *, #19570, .F. ) ;
#4334 = DIRECTION ( 'NONE',  ( 0.000000000000000000, -1.517883041479702421E-14, -1.000000000000000000 ) ) ;
#4335 = DIRECTION ( 'NONE',  ( -1.000000000000000000, 0.000000000000000000, 1.047444401652940007E-14 ) ) ;
#4336 = AXIS2_PLACEMENT_3D ( 'NONE', #1053, #10704, #15296 ) ;
#4337 = DIRECTION ( 'NONE',  ( 1.000000000000000000, -1.219044193948983948E-29, 3.491481338843133355E-15 ) ) ;
#4338 = VERTEX_POINT ( 'NONE', #20924 ) ;
#4339 = ORIENTED_EDGE ( 'NONE', *, *, #3223, .T. ) ;
#4340 = AXIS2_PLACEMENT_3D ( 'NONE', #3682, #23011, #6223 ) ;
#4341 =( BOUNDED_CURVE ( )  B_SPLINE_CURVE ( 3, ( #10055, #17189, #231, #9605 ),
 .UNSPECIFIED., .F., .T. ) 
 B_SPLINE_CURVE_WITH_KNOTS ( ( 4, 4 ),
 ( 4.339533644879389307, 4.356609821944394056 ),
 .UNSPECIFIED. ) 
 CURVE ( )  GEOMETRIC_REPRESENTATION_ITEM ( )  RATIONAL_B_SPLINE_CURVE ( ( 1.000000000000000000, 0.9999757004956882911, 0.9999757004956882911, 1.000000000000000000 ) ) 
 REPRESENTATION_ITEM ( '' )  );
#4342 = CYLINDRICAL_SURFACE ( 'NONE', #30426, 3.750000000000000444 ) ;
#4343 = CARTESIAN_POINT ( 'NONE',  ( 64.25000000000001421, 1.836970198722195229E-16, 1.374999999999777067 ) ) ;
#4344 = CARTESIAN_POINT ( 'NONE',  ( 57.01033040358699111, -0.8080171122822069618, -2.471263581425196421 ) ) ;
#4345 = VERTEX_POINT ( 'NONE', #8863 ) ;
#4346 = LINE ( 'NONE', #28577, #272 ) ;
#4347 = CARTESIAN_POINT ( 'NONE',  ( 58.65000000000002700, -0.6121634413827002907, 1.877732920581024700 ) ) ;
#4348 = DIRECTION ( 'NONE',  ( -1.000000000000000000, -1.047444401652940007E-14, -0.000000000000000000 ) ) ;
#4349 = CIRCLE ( 'NONE', #20559, 0.1000000000000002554 ) ;
#4350 = CARTESIAN_POINT ( 'NONE',  ( 58.75000000000002132, -0.5933363752205416120, 1.867039175319914923 ) ) ;
#4351 = CARTESIAN_POINT ( 'NONE',  ( 58.65000000000002700, -0.8495817349410276220, 1.671477153793481163 ) ) ;
#4352 = CIRCLE ( 'NONE', #4878, 4.800000000000000711 ) ;
#4353 = CARTESIAN_POINT ( 'NONE',  ( 51.80000000000002558, 3.850000000000016520, 1.949999999999818767 ) ) ;
#4354 = LINE ( 'NONE', #18632, #29702 ) ;
#4355 = EDGE_CURVE ( 'NONE', #29040, #1141, #13568, .T. ) ;
#4357 = CYLINDRICAL_SURFACE ( 'NONE', #21889, 159.6997717543496833 ) ;
#4356 = AXIS2_PLACEMENT_3D ( 'NONE', #24271, #26938, #2425 ) ;
#4358 = VERTEX_POINT ( 'NONE', #21097 ) ;
#4359 = EDGE_CURVE ( 'NONE', #22738, #8786, #4638, .T. ) ;
#4360 = AXIS2_PLACEMENT_3D ( 'NONE', #7812, #17487, #20023 ) ;
#4361 = CIRCLE ( 'NONE', #25107, 0.1500000000000002720 ) ;
#4362 = AXIS2_PLACEMENT_3D ( 'NONE', #4779, #9073, #14440 ) ;
#4363 = LINE ( 'NONE', #16576, #5237 ) ;
#4364 = ORIENTED_EDGE ( 'NONE', *, *, #26969, .T. ) ;
#4365 = AXIS2_PLACEMENT_3D ( 'NONE', #15295, #30004, #18307 ) ;
#4366 = CARTESIAN_POINT ( 'NONE',  ( 51.46757676178952323, 4.376162276235349147, 2.049999999999819966 ) ) ;
#4367 = CARTESIAN_POINT ( 'NONE',  ( -57.15835481156724285, 4.108500314926515351, -1.367561758111408121 ) ) ;
#4369 = CARTESIAN_POINT ( 'NONE',  ( -36.38012252111052902, 3.953287617511453078, 3.694739123711269890 ) ) ;
#4368 = DIRECTION ( 'NONE',  ( -1.000000000000000000, -0.000000000000000000, 3.491481338843133355E-15 ) ) ;
#4370 = ORIENTED_EDGE ( 'NONE', *, *, #29219, .F. ) ;
#4371 = EDGE_LOOP ( 'NONE', ( #29066, #28515, #5665 ) ) ;
#4372 = CARTESIAN_POINT ( 'NONE',  ( 22.68585293163317473, 6.704127117150638249, -2.050000000000078870 ) ) ;
#4373 = ORIENTED_EDGE ( 'NONE', *, *, #30925, .T. ) ;
#4374 = CARTESIAN_POINT ( 'NONE',  ( 56.95000000000001705, 0.000000000000000000, 0.000000000000000000 ) ) ;
#4375 = EDGE_CURVE ( 'NONE', #5258, #36, #1805, .T. ) ;
#4376 = EDGE_LOOP ( 'NONE', ( #3161, #15196, #21884, #16621, #7858 ) ) ;
#4378 = DIRECTION ( 'NONE',  ( 0.000000000000000000, 0.000000000000000000, 1.000000000000000000 ) ) ;
#4377 = CARTESIAN_POINT ( 'NONE',  ( 50.33814819168215138, 1.426738236278596972, 3.843750512866276559 ) ) ;
#4379 = AXIS2_PLACEMENT_3D ( 'NONE', #3542, #8130, #17802 ) ;
#4380 = ORIENTED_EDGE ( 'NONE', *, *, #8875, .F. ) ;
#4381 = CYLINDRICAL_SURFACE ( 'NONE', #2546, 0.05000000000000143219 ) ;
#4382 = VECTOR ( 'NONE', #10935, 1000.000000000000000 ) ;
#4383 = DIRECTION ( 'NONE',  ( 0.000000000000000000, 0.000000000000000000, 1.000000000000000000 ) ) ;
#4384 = AXIS2_PLACEMENT_3D ( 'NONE', #7289, #14098, #21 ) ;
#4385 = CARTESIAN_POINT ( 'NONE',  ( -54.45495050826418293, -1.500000000000000000, -3.300094695611020867 ) ) ;
#4386 = AXIS2_PLACEMENT_3D ( 'NONE', #20623, #10633, #30085 ) ;
#4387 = DIRECTION ( 'NONE',  ( 1.000000000000000000, 1.047444401652940007E-14, 0.000000000000000000 ) ) ;
#4388 = CARTESIAN_POINT ( 'NONE',  ( -59.07202994616203995, -4.156921938165296204, -2.246292432604653256E-13 ) ) ;
#4390 = EDGE_CURVE ( 'NONE', #11041, #29912, #14450, .T. ) ;
#4389 = CIRCLE ( 'NONE', #22596, 1.875000000000001776 ) ;
#4391 = CARTESIAN_POINT ( 'NONE',  ( 51.87254251396529980, 0.05753116748212284276, 4.370911451931760894 ) ) ;
#4392 = AXIS2_PLACEMENT_3D ( 'NONE', #15695, #10473, #25342 ) ;
#4393 = TOROIDAL_SURFACE ( 'NONE', #29169, 1.975000000000001865, 0.1000000000000000056 ) ;
#4394 = CYLINDRICAL_SURFACE ( 'NONE', #18549, 3.750000000000000444 ) ;
#4395 = DIRECTION ( 'NONE',  ( 1.000000000000000000, 0.000000000000000000, 0.000000000000000000 ) ) ;
#4396 = CARTESIAN_POINT ( 'NONE',  ( -57.54792740578359656, -1.073804522883506696, -3.225979517392338902 ) ) ;
#4397 = EDGE_CURVE ( 'NONE', #7031, #22738, #16121, .T. ) ;
#4398 = DIRECTION ( 'NONE',  ( 0.000000000000000000, -0.4295302013423027421, 0.9030524935654852259 ) ) ;
#4399 = EDGE_CURVE ( 'NONE', #30643, #15709, #9682, .T. ) ;
#4400 = ORIENTED_EDGE ( 'NONE', *, *, #8203, .F. ) ;
#4401 = AXIS2_PLACEMENT_3D ( 'NONE', #29, #2398, #28076 ) ;
#4402 = EDGE_CURVE ( 'NONE', #27109, #8262, #166, .T. ) ;
#4403 = DIRECTION ( 'NONE',  ( 3.491481338843133355E-15, 3.491481338843133355E-15, -1.000000000000000000 ) ) ;
#4404 = CIRCLE ( 'NONE', #2892, 0.1500000000000001887 ) ;
#4405 = CARTESIAN_POINT ( 'NONE',  ( -35.85663232820596136, -0.7747498368337714103, 5.363501452440941897 ) ) ;
#4406 = DIRECTION ( 'NONE',  ( 1.000000000000000000, 1.047444401652940007E-14, 0.000000000000000000 ) ) ;
#4407 = ORIENTED_EDGE ( 'NONE', *, *, #13871, .T. ) ;
#4408 = CARTESIAN_POINT ( 'NONE',  ( -36.40793637698146057, -5.360541651686778764, 0.7128348320083932599 ) ) ;
#4409 = VERTEX_POINT ( 'NONE', #14725 ) ;
#4410 =( LENGTH_UNIT ( ) NAMED_UNIT ( * ) SI_UNIT ( .MILLI., .METRE. ) );
#4412 = LINE ( 'NONE', #16620, #28304 ) ;
#4411 = CARTESIAN_POINT ( 'NONE',  ( 58.65838214097848891, 0.9083679987363961761, -1.640356269756322094 ) ) ;
#4413 = ORIENTED_EDGE ( 'NONE', *, *, #19873, .F. ) ;
#4414 = ORIENTED_EDGE ( 'NONE', *, *, #14813, .F. ) ;
#4415 = CARTESIAN_POINT ( 'NONE',  ( -59.69457535546588645, -2.411387898320983769, -1.235406689480271103 ) ) ;
#4416 = AXIS2_PLACEMENT_3D ( 'NONE', #25261, #12305, #19460 ) ;
#4417 = DIRECTION ( 'NONE',  ( 1.000000000000000000, 0.000000000000000000, -3.491481338843133355E-15 ) ) ;
#4418 = AXIS2_PLACEMENT_3D ( 'NONE', #3182, #27550, #13147 ) ;
#4420 = CARTESIAN_POINT ( 'NONE',  ( 53.81457038983117513, 5.799118250651475570, -1.689328355159275041 ) ) ;
#4419 = SPHERICAL_SURFACE ( 'NONE', #25150, 0.2500000000000000000 ) ;
#4421 = AXIS2_PLACEMENT_3D ( 'NONE', #21859, #26273, #146 ) ;
#4422 = ORIENTED_EDGE ( 'NONE', *, *, #1967, .F. ) ;
#4423 = CARTESIAN_POINT ( 'NONE',  ( -56.93749999999997158, 0.8699069336946686493, -4.241846523238428368 ) ) ;
#4424 = DIRECTION ( 'NONE',  ( -0.7313537016191670181, -0.6819983600625022513, 2.468850131082252327E-15 ) ) ;
#4425 = CARTESIAN_POINT ( 'NONE',  ( -55.39405989232414385, -4.753426312438548412E-15, 3.399999999999801847 ) ) ;
#4426 = CARTESIAN_POINT ( 'NONE',  ( -57.74999999999997158, -2.944486372867094914, 1.699999999999774358 ) ) ;
#4427 = CARTESIAN_POINT ( 'NONE',  ( -54.49131719536980967, 1.521332553059528081, -4.044684194243342468 ) ) ;
#4428 = CIRCLE ( 'NONE', #9999, 1.625000000000001332 ) ;
#4429 = EDGE_CURVE ( 'NONE', #14364, #23034, #5489, .T. ) ;
#4430 = ORIENTED_EDGE ( 'NONE', *, *, #4640, .T. ) ;
#4431 = VECTOR ( 'NONE', #6963, 1000.000000000000000 ) ;
#4432 = DIRECTION ( 'NONE',  ( 1.000000000000000000, 3.053848253006669023E-16, -2.042510438544995415E-16 ) ) ;
#4433 = AXIS2_PLACEMENT_3D ( 'NONE', #7560, #29530, #9929 ) ;
#4434 = ADVANCED_FACE ( 'NONE', ( #24527 ), #14404, .F. ) ;
#4435 = CARTESIAN_POINT ( 'NONE',  ( -36.11780688638067716, 4.018128186974130323, -3.618665893507954756 ) ) ;
#4436 = CARTESIAN_POINT ( 'NONE',  ( -54.54999999999998295, -0.9743475445367587584, 4.751120590182401848 ) ) ;
#4437 = CARTESIAN_POINT ( 'NONE',  ( -77.28999999999996362, -3.470778894058966809E-15, 5.300300110251643219E-15 ) ) ;
#4438 = DIRECTION ( 'NONE',  ( -2.614375865348240525E-16, 0.2008964009354147762, -0.9796124928211140670 ) ) ;
#4439 = AXIS2_PLACEMENT_3D ( 'NONE', #23863, #30345, #8652 ) ;
#4441 = DIRECTION ( 'NONE',  ( 0.000000000000000000, -1.000000000000000000, -4.336808689942015369E-15 ) ) ;
#4440 = DIRECTION ( 'NONE',  ( -1.000000000000000000, -0.000000000000000000, -0.000000000000000000 ) ) ;
#4442 = LINE ( 'NONE', #31199, #2336 ) ;
#4444 = LINE ( 'NONE', #26133, #26123 ) ;
#4443 = CARTESIAN_POINT ( 'NONE',  ( 50.30000000000001847, -1.391941090707485396, 3.850000000000022737 ) ) ;
#4445 = ORIENTED_EDGE ( 'NONE', *, *, #5485, .F. ) ;
#4446 = CARTESIAN_POINT ( 'NONE',  ( -62.05783247874898478, -2.669955732903997792, -0.3664444735944112908 ) ) ;
#4447 = CYLINDRICAL_SURFACE ( 'NONE', #27230, 3.075000000000000622 ) ;
#4449 = CARTESIAN_POINT ( 'NONE',  ( -36.92443669619682112, 5.094475812726813935, 1.819860688632667367 ) ) ;
#4448 = DIRECTION ( 'NONE',  ( 1.000000000000000000, -1.219044193948983948E-29, 3.491481338843133355E-15 ) ) ;
#4450 = CARTESIAN_POINT ( 'NONE',  ( 15.86395258069124203, -5.320649567603481955, 0.9667173501064290075 ) ) ;
#4451 = EDGE_LOOP ( 'NONE', ( #20168, #369, #23422, #5115 ) ) ;
#4452 = VERTEX_POINT ( 'NONE', #24386 ) ;
#4453 = DIRECTION ( 'NONE',  ( -3.023770467182126270E-15, 0.4999707644721522182, -0.8660422822663637055 ) ) ;
#4454 = DIRECTION ( 'NONE',  ( 0.9993908270190956511, -0.03489949670250202390, -3.491481338843132961E-15 ) ) ;
#4455 = VECTOR ( 'NONE', #27653, 1000.000000000000000 ) ;
#4456 = ORIENTED_EDGE ( 'NONE', *, *, #11758, .T. ) ;
#4457 = CARTESIAN_POINT ( 'NONE',  ( 58.72219294808260770, 0.5000000000006150636, 1.828782891498946350 ) ) ;
#4458 = ORIENTED_EDGE ( 'NONE', *, *, #20222, .F. ) ;
#4459 = DIRECTION ( 'NONE',  ( 0.000000000000000000, 0.2008964009354147762, -0.9796124928211140670 ) ) ;
#4460 = ORIENTED_EDGE ( 'NONE', *, *, #28019, .T. ) ;
#4461 =( NAMED_UNIT ( * ) PLANE_ANGLE_UNIT ( ) SI_UNIT ( $, .RADIAN. ) );
#4462 = DIRECTION ( 'NONE',  ( -1.000000000000000000, 1.219044193948983948E-29, -3.491481338843133355E-15 ) ) ;
#4463 = ORIENTED_EDGE ( 'NONE', *, *, #28999, .T. ) ;
#4464 = PRESENTATION_STYLE_ASSIGNMENT (( #6529 ) ) ;
#4465 = B_SPLINE_CURVE_WITH_KNOTS ( 'NONE', 3,
 ( #18842, #4249, #13893, #11554 ),
 .UNSPECIFIED., .F., .F.,
 ( 4, 4 ),
 ( 0.000000000000000000, 0.0001886355468578361809 ),
 .UNSPECIFIED. ) ;
#4466 = ADVANCED_FACE ( 'NONE', ( #24076 ), #28977, .T. ) ;
#4467 = ORIENTED_EDGE ( 'NONE', *, *, #11497, .T. ) ;
#4468 = ADVANCED_FACE ( 'NONE', ( #20 ), #26603, .F. ) ;
#4469 = CARTESIAN_POINT ( 'NONE',  ( -60.87499999999997158, -3.920666489018282036E-15, 3.399999999999783196 ) ) ;
#4470 = EDGE_CURVE ( 'NONE', #17229, #13576, #28758, .T. ) ;
#4471 = CARTESIAN_POINT ( 'NONE',  ( 65.00000000000002842, 1.401298464324817071E-42, -6.808388610744111684E-13 ) ) ;
#4472 = CARTESIAN_POINT ( 'NONE',  ( 69.25000000000001421, 4.557543281186736018E-17, -7.253552481446610839E-13 ) ) ;
#4473 = FACE_OUTER_BOUND ( 'NONE', #10149, .T. ) ;
#4474 = CARTESIAN_POINT ( 'NONE',  ( 51.80000000000001847, 6.982261990806648555E-14, -1.796574372350448449E-13 ) ) ;
#4475 = COLOUR_RGB ( '', 0.72549020, 0.75294118, 0.79215686) ;
#4477 = CARTESIAN_POINT ( 'NONE',  ( 51.79118295937481520, 4.088185644532909002, -1.991056910035179817 ) ) ;
#4476 = CARTESIAN_POINT ( 'NONE',  ( -36.14504829323105639, 4.698774973472866101, -2.676767126782043427 ) ) ;
#4478 = LINE ( 'NONE', #14129, #19077 ) ;
#4479 = DIRECTION ( 'NONE',  ( 1.000000000000000000, 0.000000000000000000, 0.000000000000000000 ) ) ;
#4480 = CARTESIAN_POINT ( 'NONE',  ( -36.52679053911623441, -2.412550141807427106, -4.840569432287353813 ) ) ;
#4481 = B_SPLINE_CURVE_WITH_KNOTS ( 'NONE', 3,
 ( #25389, #1314, #20200, #27300, #24767, #6086, #8453, #18133, #29979, #18279, #22557, #3231 ),
 .UNSPECIFIED., .F., .F.,
 ( 4, 2, 2, 2, 2, 4 ),
 ( 0.000000000000000000, 5.522938194211729973E-05, 0.0001104587638842345995, 0.0002209175277684801765, 0.0004418350555369711949, 0.0008836701110739511719 ),
 .UNSPECIFIED. ) ;
#4482 = EDGE_CURVE ( 'NONE', #9046, #2667, #19172, .T. ) ;
#4483 = VERTEX_POINT ( 'NONE', #15034 ) ;
#4484 = DIRECTION ( 'NONE',  ( -1.000000000000000000, -0.000000000000000000, -0.000000000000000000 ) ) ;
#4485 = DIRECTION ( 'NONE',  ( 1.000000000000000000, -1.219044193948983948E-29, 3.491481338843133355E-15 ) ) ;
#4486 = ORIENTED_EDGE ( 'NONE', *, *, #23258, .F. ) ;
#4488 = CARTESIAN_POINT ( 'NONE',  ( 58.75000000000002132, 6.153735859711025284E-13, 3.111507638930570854E-58 ) ) ;
#4487 = DIRECTION ( 'NONE',  ( 1.000000000000000000, 1.047444401652940007E-14, 0.000000000000000000 ) ) ;
#4489 = CARTESIAN_POINT ( 'NONE',  ( 54.30613356357999777, 6.708647743757887305, -2.050000000000188560 ) ) ;
#4490 = DIRECTION ( 'NONE',  ( -9.958586508671106819E-15, 0.9507508458640636650, -0.3099561728515299319 ) ) ;
#4491 = ORIENTED_EDGE ( 'NONE', *, *, #1688, .T. ) ;
#4492 = CARTESIAN_POINT ( 'NONE',  ( 31.20024169370289613, 7.859880413227774199, 1.424999999999891687 ) ) ;
#4493 = CARTESIAN_POINT ( 'NONE',  ( -59.37499999999997868, -3.920666489018300969E-15, 3.399999999999788525 ) ) ;
#4494 = EDGE_LOOP ( 'NONE', ( #21455, #27286, #23573, #6104, #4186 ) ) ;
#4495 = ORIENTED_EDGE ( 'NONE', *, *, #18598, .F. ) ;
#4496 = CARTESIAN_POINT ( 'NONE',  ( 15.98305126557427869, 4.951626736499044057, 2.174059107776793454 ) ) ;
#4497 = STYLED_ITEM ( 'NONE', ( #27430 ), #1717 ) ;
#4498 = VERTEX_POINT ( 'NONE', #2553 ) ;
#4499 = DIRECTION ( 'NONE',  ( -9.994490842163784987E-15, 0.7438053426821212843, -0.6683962987610958528 ) ) ;
#4500 = CIRCLE ( 'NONE', #16123, 0.2499999999999986955 ) ;
#4501 = CARTESIAN_POINT ( 'NONE',  ( -56.69702994616203284, -2.078460969082631227, -3.600000000000207923 ) ) ;
#4502 = ORIENTED_EDGE ( 'NONE', *, *, #15891, .T. ) ;
#4503 = CARTESIAN_POINT ( 'NONE',  ( 48.30000000000001847, 2.478823385132571406E-14, 4.100000000000022737 ) ) ;
#4504 =( BOUNDED_SURFACE ( )  B_SPLINE_SURFACE ( 3, 2, ( 
 ( #16350, #19053, #4623 ),
 ( #26473, #30760, #11757 ),
 ( #7019, #14283, #4303 ),
 ( #28860, #4943, #2243 ) ),
 .UNSPECIFIED., .F., .F., .F. ) 
 B_SPLINE_SURFACE_WITH_KNOTS ( ( 4, 4 ),
 ( 3, 3 ),
 ( 5.003379805550770776, 5.119240129666620120 ),
 ( 0.000000000000000000, 1.000000000000000000 ),
 .UNSPECIFIED. ) 
 GEOMETRIC_REPRESENTATION_ITEM ( )  RATIONAL_B_SPLINE_SURFACE ( (
 ( 1.000000000000000000, 0.6043181045777066274, 1.000000000000000000),
 ( 1.000000000000000000, 0.5899361674293883695, 1.000000000000000000),
 ( 1.000000000000000000, 0.5752896509278045967, 1.000000000000000000),
 ( 1.000000000000000000, 0.5604218610591197303, 1.000000000000000000) ) ) 
 REPRESENTATION_ITEM ( '' )  SURFACE ( )  );
#4505 = CARTESIAN_POINT ( 'NONE',  ( 31.33102771648083618, 7.478136438692525090, 2.049999999999890132 ) ) ;
#4506 = ORIENTED_EDGE ( 'NONE', *, *, #29746, .F. ) ;
#4507 = ORIENTED_EDGE ( 'NONE', *, *, #19286, .T. ) ;
#4508 = ADVANCED_FACE ( 'NONE', ( #314 ), #24693, .F. ) ;
#4509 = CARTESIAN_POINT ( 'NONE',  ( 50.25000000000000711, 1.106298139390723190, -1.666164585742097914 ) ) ;
#4510 = ADVANCED_FACE ( 'NONE', ( #7607 ), #30250, .T. ) ;
#4511 = DIRECTION ( 'NONE',  ( -0.03489949670185131525, -0.9993908270191184107, 0.000000000000000000 ) ) ;
#4512 = CARTESIAN_POINT ( 'NONE',  ( -54.72085481156724285, 1.184343223768591580, 3.558065644182726750 ) ) ;
#4513 = ORIENTED_EDGE ( 'NONE', *, *, #7852, .T. ) ;
#4514 = AXIS2_PLACEMENT_3D ( 'NONE', #30626, #23694, #30800 ) ;
#4515 = CARTESIAN_POINT ( 'NONE',  ( 50.50000000000002132, 2.428612866367529932E-14, 0.000000000000000000 ) ) ;
#4516 = DIRECTION ( 'NONE',  ( 0.000000000000000000, 0.000000000000000000, 1.000000000000000000 ) ) ;
#4517 = FACE_OUTER_BOUND ( 'NONE', #27998, .T. ) ;
#4518 = FACE_OUTER_BOUND ( 'NONE', #29031, .T. ) ;
#4520 = CARTESIAN_POINT ( 'NONE',  ( 58.65000000000005542, -1.827356000909702294, -0.4213753797513699051 ) ) ;
#4519 = SURFACE_STYLE_USAGE ( .BOTH. , #20996 ) ;
#4521 = CARTESIAN_POINT ( 'NONE',  ( 58.75000000000002132, -0.4999999999991334154, 1.863080903344709549 ) ) ;
#4522 = FACE_OUTER_BOUND ( 'NONE', #25805, .T. ) ;
#4523 = CIRCLE ( 'NONE', #22238, 2.649999999999999911 ) ;
#4524 = EDGE_CURVE ( 'NONE', #21420, #12623, #3529, .T. ) ;
#4525 = CARTESIAN_POINT ( 'NONE',  ( 61.25000000000002132, 6.415596960124259844E-13, 3.111507638930570854E-58 ) ) ;
#4526 = ORIENTED_EDGE ( 'NONE', *, *, #27619, .T. ) ;
#4527 = ORIENTED_EDGE ( 'NONE', *, *, #24721, .T. ) ;
#4528 = ORIENTED_EDGE ( 'NONE', *, *, #3455, .F. ) ;
#4529 = DIRECTION ( 'NONE',  ( 1.000000000000000000, 0.000000000000000000, 0.000000000000000000 ) ) ;
#4530 = CARTESIAN_POINT ( 'NONE',  ( -55.42292740578360366, -3.330682475591783209, -0.6830477631804113825 ) ) ;
#4532 = CARTESIAN_POINT ( 'NONE',  ( -36.80043232705877898, 3.597789892641451104, 4.037455662930098832 ) ) ;
#4531 = CARTESIAN_POINT ( 'NONE',  ( 50.83686442967772479, 8.734989671305513070, -2.050000000000176570 ) ) ;
#4533 = ORIENTED_EDGE ( 'NONE', *, *, #5340, .T. ) ;
#4534 = VERTEX_POINT ( 'NONE', #27225 ) ;
#4535 = EDGE_CURVE ( 'NONE', #4273, #4826, #11537, .T. ) ;
#4536 = DIRECTION ( 'NONE',  ( 1.000000000000000000, 3.053848253006669023E-16, -2.042510438544995415E-16 ) ) ;
#4537 = VERTEX_POINT ( 'NONE', #13408 ) ;
#4538 = CARTESIAN_POINT ( 'NONE',  ( 41.48619405471883681, -151.3359592902621955, -1.950000000000163380 ) ) ;
#4539 =( BOUNDED_CURVE ( )  B_SPLINE_CURVE ( 2, ( #3996, #23322, #6534, #1762, #16195, #25843, #13785, #11434, #29451 ),
 .UNSPECIFIED., .F., .T. ) 
 B_SPLINE_CURVE_WITH_KNOTS ( ( 3, 2, 2, 2, 3 ),
 ( 0.08333333333333334259, 0.09259259259259258745, 0.1111111111111111049, 0.1296296296296296224, 0.1388888888888888951 ),
 .UNSPECIFIED. ) 
 CURVE ( )  GEOMETRIC_REPRESENTATION_ITEM ( )  RATIONAL_B_SPLINE_CURVE ( ( 0.9330127018922192983, 0.9330127018922194093, 1.000000000000000000, 0.8660254037844387076, 1.000000000000000000, 0.8660254037844387076, 1.000000000000000000, 0.9330127018922191873, 0.9330127018922192983 ) ) 
 REPRESENTATION_ITEM ( '' )  );
#4540 = EDGE_LOOP ( 'NONE', ( #15894, #24992, #23976, #20010 ) ) ;
#4542 = DIRECTION ( 'NONE',  ( 0.000000000000000000, 1.000000000000000000, 3.491481338843252079E-15 ) ) ;
#4541 = CARTESIAN_POINT ( 'NONE',  ( 61.25000000000004263, -1.470078920827193825, -1.320078920827526758 ) ) ;
#4543 = VERTEX_POINT ( 'NONE', #23114 ) ;
#4544 = CARTESIAN_POINT ( 'NONE',  ( 65.00000000000001421, -1.025519176787267142E-28, -6.808388610744108654E-13 ) ) ;
#4545 = FACE_BOUND ( 'NONE', #19947, .T. ) ;
#4546 = AXIS2_PLACEMENT_3D ( 'NONE', #31003, #9324, #18989 ) ;
#4547 = ADVANCED_FACE ( 'NONE', ( #15814 ), #3312, .T. ) ;
#4548 = CARTESIAN_POINT ( 'NONE',  ( 15.03925126672133139, -5.377732432866647372, 0.5657657256215454789 ) ) ;
#4549 = CIRCLE ( 'NONE', #10, 0.1000000000000001443 ) ;
#4550 = CARTESIAN_POINT ( 'NONE',  ( 15.03925126672123369, -4.683225679163331101, -2.703237727951255387 ) ) ;
#4551 = PRODUCT_DEFINITION_SHAPE ( 'NONE', 'NONE',  #31334 ) ;
#4552 = CARTESIAN_POINT ( 'NONE',  ( -56.75952994616203995, -3.117691453623963938, -1.800000000000212763 ) ) ;
#4553 = VECTOR ( 'NONE', #17171, 1000.000000000000000 ) ;
#4554 = DIRECTION ( 'NONE',  ( 1.000000000000000000, -0.000000000000000000, -1.047444401652940007E-14 ) ) ;
#4555 = CARTESIAN_POINT ( 'NONE',  ( 50.50000000000002132, 2.428612866367529932E-14, 0.000000000000000000 ) ) ;
#4556 = CARTESIAN_POINT ( 'NONE',  ( -58.48542740578359656, -3.725040285533367523, 1.239922660687669209 ) ) ;
#4557 = ADVANCED_FACE ( 'NONE', ( #10747 ), #3964, .T. ) ;
#4558 = AXIS2_PLACEMENT_3D ( 'NONE', #3252, #29850, #17676 ) ;
#4559 = PLANE ( 'NONE',  #7391 ) ;
#4560 = ORIENTED_EDGE ( 'NONE', *, *, #31125, .F. ) ;
#4561 = DIRECTION ( 'NONE',  ( 3.489354422748178582E-15, -1.218509414717996338E-16, 1.000000000000000000 ) ) ;
#4562 = CARTESIAN_POINT ( 'NONE',  ( 53.17422497822705196, 4.853022681123431603, 1.601063398553745021 ) ) ;
#4563 = CARTESIAN_POINT ( 'NONE',  ( 53.82818506963806016, 5.794550291359760408, 1.819877325055229145 ) ) ;
#4564 = ORIENTED_EDGE ( 'NONE', *, *, #10947, .T. ) ;
#4565 = CARTESIAN_POINT ( 'NONE',  ( 63.50000000000002842, 1.401298464324817071E-42, -6.651271950496169736E-13 ) ) ;
#4566 = VERTEX_POINT ( 'NONE', #7905 ) ;
#4567 = FILL_AREA_STYLE_COLOUR ( '', #21336 ) ;
#4569 = CARTESIAN_POINT ( 'NONE',  ( 58.65000000000003411, -1.394635017527501297, 1.253243060178016899 ) ) ;
#4568 = CARTESIAN_POINT ( 'NONE',  ( 51.59043415373528063, -4.226158602834444444, -1.819860353018915911 ) ) ;
#4570 = EDGE_CURVE ( 'NONE', #26101, #24402, #488, .T. ) ;
#4571 = EDGE_LOOP ( 'NONE', ( #27306, #2557, #12420 ) ) ;
#4572 = AXIS2_PLACEMENT_3D ( 'NONE', #20687, #5956, #20524 ) ;
#4573 = CARTESIAN_POINT ( 'NONE',  ( -44.59999999999996589, -1.399999999999979039, -3.959797974644846619 ) ) ;
#4575 = CARTESIAN_POINT ( 'NONE',  ( 58.72427158855730767, 0.9764256747737051212, 1.600821037878903619 ) ) ;
#4574 = CARTESIAN_POINT ( 'NONE',  ( 58.65000000000002700, -0.5811678240974692544, 1.782657835994643447 ) ) ;
#4576 = ORIENTED_EDGE ( 'NONE', *, *, #541, .T. ) ;
#4577 = CARTESIAN_POINT ( 'NONE',  ( -60.36042740578359656, 3.725040285533370632, -1.239922660687674982 ) ) ;
#4578 = FACE_OUTER_BOUND ( 'NONE', #5736, .T. ) ;
#4579 = CYLINDRICAL_SURFACE ( 'NONE', #25145, 4.000000000000000000 ) ;
#4580 = CARTESIAN_POINT ( 'NONE',  ( -36.00201293083839005, 4.018128179617898255, 3.618665901676350938 ) ) ;
#4581 = EDGE_CURVE ( 'NONE', #7044, #8649, #8072, .T. ) ;
#4582 = CARTESIAN_POINT ( 'NONE',  ( -61.35799158996540825, -2.608967300040148984, -0.6002010391711750659 ) ) ;
#4583 = EDGE_CURVE ( 'NONE', #16075, #17943, #1430, .T. ) ;
#4584 = CARTESIAN_POINT ( 'NONE',  ( 61.25000000000003553, -1.323060376180724029, -1.499837071477706729 ) ) ;
#4585 = ADVANCED_FACE ( 'NONE', ( #3157 ), #12078, .F. ) ;
#4586 = VERTEX_POINT ( 'NONE', #951 ) ;
#4587 = FACE_OUTER_BOUND ( 'NONE', #3730, .T. ) ;
#4588 = CARTESIAN_POINT ( 'NONE',  ( -36.04581030752699888, 3.779372845002908932, -3.883777290284648576 ) ) ;
#4589 = CARTESIAN_POINT ( 'NONE',  ( 48.37784963381696457, 1.308847734660516071, -3.885629509820973659 ) ) ;
#4590 = CARTESIAN_POINT ( 'NONE',  ( 61.25000000000002132, 6.415596960124259844E-13, 3.111507638930570854E-58 ) ) ;
#4591 = CONICAL_SURFACE ( 'NONE', #13658, 2.765000000000001013, 0.03997868712329009228 ) ;
#4592 = CARTESIAN_POINT ( 'NONE',  ( 51.23644008536122385, 1.080112125196981854, 1.214076932077872817 ) ) ;
#4593 = CYLINDRICAL_SURFACE ( 'NONE', #6962, 1.000000000000000000 ) ;
#4594 = CARTESIAN_POINT ( 'NONE',  ( -62.09999999999998010, -2.625757682666624682, -0.2804666419185123383 ) ) ;
#4596 = CARTESIAN_POINT ( 'NONE',  ( 60.81561938753820584, -0.6499999999993623101, 1.489337100860648633 ) ) ;
#4595 = DIRECTION ( 'NONE',  ( 0.000000000000000000, 0.000000000000000000, -1.000000000000000000 ) ) ;
#4597 = EDGE_LOOP ( 'NONE', ( #26376, #29185, #8642, #10821 ) ) ;
#4598 = DIRECTION ( 'NONE',  ( -1.000000000000000000, -0.000000000000000000, -0.000000000000000000 ) ) ;
#4599 = CARTESIAN_POINT ( 'NONE',  ( 52.06628335902946247, -0.5434431642975682264, 1.794517909405659806 ) ) ;
#4601 = CARTESIAN_POINT ( 'NONE',  ( -36.68866260399369850, 4.872353571451107257, 2.347449169364858701 ) ) ;
#4600 = CARTESIAN_POINT ( 'NONE',  ( 16.10624235918717773, -3.046685255238767986, -4.470266847515925512 ) ) ;
#4602 = CARTESIAN_POINT ( 'NONE',  ( 15.03925126672133317, -4.861582140531632845, 2.394243978978315646 ) ) ;
#4603 = ADVANCED_FACE ( 'NONE', ( #27697 ), #12797, .T. ) ;
#4604 = VERTEX_POINT ( 'NONE', #20280 ) ;
#4605 = ORIENTED_EDGE ( 'NONE', *, *, #13802, .T. ) ;
#4606 = CARTESIAN_POINT ( 'NONE',  ( -57.28335481156723574, 0.7533615035078095046, -3.673546848079178861 ) ) ;
#4607 = ORIENTED_EDGE ( 'NONE', *, *, #11156, .T. ) ;
#4608 = EDGE_CURVE ( 'NONE', #15357, #3421, #16631, .T. ) ;
#4609 = FACE_OUTER_BOUND ( 'NONE', #29544, .T. ) ;
#4610 = CARTESIAN_POINT ( 'NONE',  ( 58.74840439586692753, 0.5000000000006153966, 1.859896009349663037 ) ) ;
#4611 = ORIENTED_EDGE ( 'NONE', *, *, #28999, .F. ) ;
#4612 = CARTESIAN_POINT ( 'NONE',  ( -56.67499999999996874, 3.131991715727200307E-15, -1.107867533772800737E-16 ) ) ;
#4613 = ORIENTED_EDGE ( 'NONE', *, *, #14032, .F. ) ;
#4614 = CARTESIAN_POINT ( 'NONE',  ( 58.75000000000002132, -0.5380862305903428844, -2.008165151418244143 ) ) ;
#4615 = FILL_AREA_STYLE_COLOUR ( '', #17130 ) ;
#4616 = EDGE_CURVE ( 'NONE', #737, #5233, #2469, .T. ) ;
#4617 = EDGE_CURVE ( 'NONE', #28052, #22181, #26217, .T. ) ;
#4618 = ORIENTED_EDGE ( 'NONE', *, *, #29522, .T. ) ;
#4619 = CARTESIAN_POINT ( 'NONE',  ( -59.49999999999997158, 2.944486372867092250, 1.699999999999800115 ) ) ;
#4620 = DIRECTION ( 'NONE',  ( 0.000000000000000000, 0.2008964009354147484, -0.9796124928211139560 ) ) ;
#4621 = DIRECTION ( 'NONE',  ( 1.000000000000000000, 0.000000000000000000, 0.000000000000000000 ) ) ;
#4622 = CARTESIAN_POINT ( 'NONE',  ( -54.49999999999999289, -1.400000000000004574, 3.363870538531238186 ) ) ;
#4623 = CARTESIAN_POINT ( 'NONE',  ( -61.38768957378469793, -2.520043259258192503, -0.7763025981709992251 ) ) ;
#4624 = AXIS2_PLACEMENT_3D ( 'NONE', #14198, #4695, #26721 ) ;
#4626 = CARTESIAN_POINT ( 'NONE',  ( -41.12388279035661753, -1.755788972190012401E-14, 0.000000000000000000 ) ) ;
#4625 =( NAMED_UNIT ( * ) SI_UNIT ( $, .STERADIAN. ) SOLID_ANGLE_UNIT ( ) );
#4627 = B_SPLINE_CURVE_WITH_KNOTS ( 'NONE', 3,
 ( #7882, #27211, #5522, #30317, #8625, #6886, #26032, #21321, #23838, #16385, #7055, #28264, #9595, #7204, #2129, #9269, #11791, #18932, #30623 ),
 .UNSPECIFIED., .F., .F.,
 ( 4, 3, 3, 3, 3, 3, 4 ),
 ( 0.000000000000000000, 6.909591911046148761E-06, 4.342671684267912936E-05, 7.786482953143393916E-05, 0.0001105775006590781824, 0.0001427429525918440115, 0.0001749426303720831523 ),
 .UNSPECIFIED. ) ;
#4628 = DIRECTION ( 'NONE',  ( 2.117927888850091331E-16, -0.02490330187381135929, 0.9996898646859343485 ) ) ;
#4629 = DIRECTION ( 'NONE',  ( 3.304235192336781034E-15, 0.000000000000000000, 1.000000000000000000 ) ) ;
#4630 = CYLINDRICAL_SURFACE ( 'NONE', #23584, 3.625000000000028866 ) ;
#4631 = VERTEX_POINT ( 'NONE', #26096 ) ;
#4632 = CARTESIAN_POINT ( 'NONE',  ( 58.66133336607604321, -1.348863877412392664, -1.302803168107730114 ) ) ;
#4633 = CARTESIAN_POINT ( 'NONE',  ( 60.81472790383496374, -0.4999999999993504640, 1.863080903340958328 ) ) ;
#4635 = CARTESIAN_POINT ( 'NONE',  ( 50.38693217303928407, -1.296871156637275702, 3.889656364559860080 ) ) ;
#4634 = CARTESIAN_POINT ( 'NONE',  ( 61.25000000000004263, -1.800471618824186493, -1.039502773796582069 ) ) ;
#4636 = CARTESIAN_POINT ( 'NONE',  ( 54.27131183106372703, 6.003201256477255221, -2.050000000000188116 ) ) ;
#4637 = EDGE_CURVE ( 'NONE', #7143, #23119, #23419, .T. ) ;
#4638 = B_SPLINE_CURVE_WITH_KNOTS ( 'NONE', 3,
 ( #17409, #26770, #4745, #17123, #29432, #21879 ),
 .UNSPECIFIED., .F., .F.,
 ( 4, 2, 4 ),
 ( 0.000000000000000000, 0.0001939776071359005987, 0.0003879552142718011975 ),
 .UNSPECIFIED. ) ;
#4639 = DIRECTION ( 'NONE',  ( 1.000000000000000000, 1.047444401652940007E-14, 0.000000000000000000 ) ) ;
#4640 = EDGE_CURVE ( 'NONE', #20201, #3601, #15751, .T. ) ;
#4641 = AXIS2_PLACEMENT_3D ( 'NONE', #6535, #25844, #25994 ) ;
#4642 = ORIENTED_EDGE ( 'NONE', *, *, #5312, .F. ) ;
#4643 = ADVANCED_FACE ( 'NONE', ( #18674 ), #26260, .T. ) ;
#4644 = CARTESIAN_POINT ( 'NONE',  ( 52.10126625705170511, 0.5195911883743922210, 1.546252172343136388 ) ) ;
#4645 = CARTESIAN_POINT ( 'NONE',  ( 34.55000000000001847, 0.000000000000000000, 0.000000000000000000 ) ) ;
#4646 = CARTESIAN_POINT ( 'NONE',  ( -59.18749999999996447, -3.925981830489445379, -2.242119407191119848E-13 ) ) ;
#4647 = ORIENTED_EDGE ( 'NONE', *, *, #1847, .T. ) ;
#4648 = VERTEX_POINT ( 'NONE', #28156 ) ;
#4649 = CARTESIAN_POINT ( 'NONE',  ( 15.41080140630216988, 4.895960019030393795, 2.323379425334584081 ) ) ;
#4650 = ORIENTED_EDGE ( 'NONE', *, *, #12450, .T. ) ;
#4651 = VECTOR ( 'NONE', #3785, 1000.000000000000000 ) ;
#4652 = LINE ( 'NONE', #26497, #5545 ) ;
#4653 = VECTOR ( 'NONE', #28419, 1000.000000000000000 ) ;
#4654 = CARTESIAN_POINT ( 'NONE',  ( -58.25952994616203284, -3.117691453623963938, -1.800000000000218092 ) ) ;
#4655 = ORIENTED_EDGE ( 'NONE', *, *, #28790, .T. ) ;
#4656 = DIRECTION ( 'NONE',  ( -0.1208805777273481014, 0.9926670569371698338, 0.000000000000000000 ) ) ;
#4657 = CYLINDRICAL_SURFACE ( 'NONE', #19757, 0.1499999999999999667 ) ;
#4658 = CARTESIAN_POINT ( 'NONE',  ( 33.39233489564711732, 8.222108905996257988, 2.049999999999883027 ) ) ;
#4659 = ORIENTED_EDGE ( 'NONE', *, *, #9443, .F. ) ;
#4660 = DIRECTION ( 'NONE',  ( -3.491481338843133355E-15, -3.491481338843133355E-15, 1.000000000000000000 ) ) ;
#4661 = MANIFOLD_SOLID_BREP ( 'Stock-MAS-683-1', #8946 ) ;
#4662 = LINE ( 'NONE', #9427, #25032 ) ;
#4663 = CARTESIAN_POINT ( 'NONE',  ( 58.65000045311413146, -0.8645309767535818146, -1.663878723407328897 ) ) ;
#4664 = ORIENTED_EDGE ( 'NONE', *, *, #27378, .F. ) ;
#4665 = CARTESIAN_POINT ( 'NONE',  ( -61.39999999999998437, -2.604492677689918878, 0.7117709546332967596 ) ) ;
#4666 = DIRECTION ( 'NONE',  ( 1.000000000000000000, 0.000000000000000000, 0.000000000000000000 ) ) ;
#4667 = CARTESIAN_POINT ( 'NONE',  ( 47.00000000000002132, -3.976179070414207928, -1.000000000000000000 ) ) ;
#4668 = CARTESIAN_POINT ( 'NONE',  ( -60.49999999999997868, 1.656632322739229403E-15, 1.870925083934595927E-15 ) ) ;
#4669 = CARTESIAN_POINT ( 'NONE',  ( -73.90999999999998238, -1.259609229504280004, -0.03137816036099756040 ) ) ;
#4670 = B_SPLINE_CURVE_WITH_KNOTS ( 'NONE', 3,
 ( #25797, #4107, #1714, #13134, #20444, #23904, #150, #16635, #13900, #21540, #2197, #31016, #4582, #19174, #28338, #16785, #11860, #7267, #4255 ),
 .UNSPECIFIED., .F., .F.,
 ( 4, 3, 3, 3, 3, 3, 4 ),
 ( -1.475060283556113230E-06, 0.000000000000000000, 2.253555103675729373E-05, 4.073269212999672338E-05, 5.627305529011999768E-05, 7.083906737679824997E-05, 8.547717314343541571E-05 ),
 .UNSPECIFIED. ) ;
#4671 = DIRECTION ( 'NONE',  ( 0.000000000000000000, 0.000000000000000000, 1.000000000000000000 ) ) ;
#4672 = ORIENTED_EDGE ( 'NONE', *, *, #10728, .F. ) ;
#4673 = EDGE_CURVE ( 'NONE', #2624, #4056, #16618, .T. ) ;
#4674 = CARTESIAN_POINT ( 'NONE',  ( -59.15690588169601227, -2.360521237243748072, 1.241563447891223859 ) ) ;
#4675 = ORIENTED_EDGE ( 'NONE', *, *, #7674, .T. ) ;
#4676 =( BOUNDED_CURVE ( )  B_SPLINE_CURVE ( 3, ( #3688, #20662, #25529, #10671 ),
 .UNSPECIFIED., .F., .T. ) 
 B_SPLINE_CURVE_WITH_KNOTS ( ( 4, 4 ),
 ( 1.817784745758538767, 2.232964403949253107 ),
 .UNSPECIFIED. ) 
 CURVE ( )  GEOMETRIC_REPRESENTATION_ITEM ( )  RATIONAL_B_SPLINE_CURVE ( ( 1.000000000000000000, 0.9856869983806465507, 0.9856869983806465507, 1.000000000000000000 ) ) 
 REPRESENTATION_ITEM ( '' )  );
#4677 = CARTESIAN_POINT ( 'NONE',  ( 53.13232117966331458, 4.211086031869615276, 2.049999999999814637 ) ) ;
#4678 = CIRCLE ( 'NONE', #24396, 0.1000000000000000472 ) ;
#4679 = CARTESIAN_POINT ( 'NONE',  ( -55.86042740578360366, 3.725040285533370632, -1.239922660687676315 ) ) ;
#4681 = DIRECTION ( 'NONE',  ( 1.000000000000000000, -0.000000000000000000, -1.047444401652940007E-14 ) ) ;
#4680 = DIRECTION ( 'NONE',  ( 0.000000000000000000, 0.000000000000000000, -1.000000000000000000 ) ) ;
#4682 = VERTEX_POINT ( 'NONE', #23268 ) ;
#4683 = ORIENTED_EDGE ( 'NONE', *, *, #31020, .F. ) ;
#4684 = CARTESIAN_POINT ( 'NONE',  ( -67.89999999999997726, -6.032153844857049047E-16, 3.382382808457892732E-15 ) ) ;
#4685 = ORIENTED_EDGE ( 'NONE', *, *, #25214, .F. ) ;
#4686 = CARTESIAN_POINT ( 'NONE',  ( 69.25000000000001421, 1.401298464324817071E-42, -7.253552481446610839E-13 ) ) ;
#4687 = VERTEX_POINT ( 'NONE', #15959 ) ;
#4688 = CARTESIAN_POINT ( 'NONE',  ( -36.72207054450174724, 5.313409993919671948, 1.009519134730257228 ) ) ;
#4689 = ORIENTED_EDGE ( 'NONE', *, *, #2821, .T. ) ;
#4690 = B_SPLINE_CURVE_WITH_KNOTS ( 'NONE', 3,
 ( #27638, #3260, #27172, #12598, #7842, #21713 ),
 .UNSPECIFIED., .F., .F.,
 ( 4, 2, 4 ),
 ( 0.000000000000000000, 0.0001000270069607746585, 0.0002000540139215493170 ),
 .UNSPECIFIED. ) ;
#4691 = DIRECTION ( 'NONE',  ( -1.000000000000000000, -3.054025858079668409E-16, 2.042474015755241579E-16 ) ) ;
#4692 = CARTESIAN_POINT ( 'NONE',  ( 57.00074754615238248, 0.7099475343046129927, 1.812279303590036639 ) ) ;
#4693 = EDGE_CURVE ( 'NONE', #18665, #12339, #19804, .T. ) ;
#4694 = CARTESIAN_POINT ( 'NONE',  ( -54.48833221701376317, -1.517896399908648108, -3.311598511234999709 ) ) ;
#4695 = DIRECTION ( 'NONE',  ( 0.3420201433256656043, -0.02340144900402423012, 0.9394011889198369269 ) ) ;
#4696 = CARTESIAN_POINT ( 'NONE',  ( -60.07202994616204705, 2.078460969082646770, 3.599999999999794031 ) ) ;
#4697 = CARTESIAN_POINT ( 'NONE',  ( 59.35000000000002984, 1.401298464324817071E-42, -6.216582523810200043E-13 ) ) ;
#4698 = LINE ( 'NONE', #26247, #18101 ) ;
#4699 = AXIS2_PLACEMENT_3D ( 'NONE', #7963, #367, #27273 ) ;
#4700 = FILL_AREA_STYLE ('',( #265 ) ) ;
#4701 = CYLINDRICAL_SURFACE ( 'NONE', #6898, 3.399999999999999911 ) ;
#4702 = VERTEX_POINT ( 'NONE', #27994 ) ;
#4703 = CARTESIAN_POINT ( 'NONE',  ( 47.07708546080149858, 8.766223091587681537, -1.550000000000163469 ) ) ;
#4704 = CARTESIAN_POINT ( 'NONE',  ( -59.09999999999997300, 8.366749974758448157E-15, -2.099585467500611340E-13 ) ) ;
#4705 = DIRECTION ( 'NONE',  ( 0.000000000000000000, 0.000000000000000000, 1.000000000000000000 ) ) ;
#4706 = ORIENTED_EDGE ( 'NONE', *, *, #13438, .F. ) ;
#4707 = EDGE_CURVE ( 'NONE', #12071, #26982, #10685, .T. ) ;
#4708 = CARTESIAN_POINT ( 'NONE',  ( -54.49999516060625382, 1.549196738101655590, 4.063926895246979143 ) ) ;
#4709 =( BOUNDED_SURFACE ( )  B_SPLINE_SURFACE ( 3, 2, ( 
 ( #28864, #28713, #11608 ),
 ( #6849, #2423, #16838 ),
 ( #7176, #12084, #21291 ),
 ( #26477, #191, #28540 ),
 ( #21760, #26796, #19524 ),
 ( #16991, #11761, #21436 ) ),
 .UNSPECIFIED., .F., .F., .F. ) 
 B_SPLINE_SURFACE_WITH_KNOTS ( ( 4, 2, 4 ),
 ( 3, 3 ),
 ( 0.0001319104779587709254, 0.0002905946498119449514, 0.0004492788216651190315 ),
 ( 0.000000000000000000, 1.000000000000000000 ),
 .UNSPECIFIED. ) 
 GEOMETRIC_REPRESENTATION_ITEM ( )  RATIONAL_B_SPLINE_SURFACE ( (
 ( 1.000000000000000000, 0.7779866052154992273, 1.000000000000000000),
 ( 1.000000000000000000, 0.7780052684394881402, 1.000000000000000000),
 ( 1.000000000000000000, 0.7724636952541197310, 1.000000000000000000),
 ( 1.000000000000000000, 0.7490013934199948320, 1.000000000000000000),
 ( 1.000000000000000000, 0.7305684325697214820, 1.000000000000000000),
 ( 1.000000000000000000, 0.7071067811865471286, 1.000000000000000000) ) ) 
 REPRESENTATION_ITEM ( '' )  SURFACE ( )  );
#4710 = VERTEX_POINT ( 'NONE', #8675 ) ;
#4712 = DIRECTION ( 'NONE',  ( 3.489354422748178582E-15, -1.218509414717996338E-16, 1.000000000000000000 ) ) ;
#4711 = CARTESIAN_POINT ( 'NONE',  ( -57.62499999999996447, -2.944486372867072710, -1.700000000000221334 ) ) ;
#4713 = ORIENTED_EDGE ( 'NONE', *, *, #62, .F. ) ;
#4714 = CARTESIAN_POINT ( 'NONE',  ( 51.01608411450973080, -0.7569233679470204201, 1.030722644926826748 ) ) ;
#4715 = DIRECTION ( 'NONE',  ( 0.000000000000000000, 1.000000000000000000, 0.000000000000000000 ) ) ;
#4717 = CARTESIAN_POINT ( 'NONE',  ( 58.65844932252329613, 0.9087029769946789459, 1.640171707773312004 ) ) ;
#4716 = CARTESIAN_POINT ( 'NONE',  ( 58.64999999999991331, -0.8948927608045756932, 1.760622601995819325 ) ) ;
#4718 = EDGE_LOOP ( 'NONE', ( #174, #16253, #6562, #13548 ) ) ;
#4719 = CARTESIAN_POINT ( 'NONE',  ( -54.56249999999997868, 4.108500314926513575, -1.367561758111407899 ) ) ;
#4720 = CARTESIAN_POINT ( 'NONE',  ( -57.22499999999997300, -0.9241234443029052725, 4.506217466977124886 ) ) ;
#4721 = DIRECTION ( 'NONE',  ( -1.000000000000000000, -3.054025858079668409E-16, 2.042474015755241579E-16 ) ) ;
#4722 = AXIS2_PLACEMENT_3D ( 'NONE', #17774, #30404, #22841 ) ;
#4723 = DIRECTION ( 'NONE',  ( 0.000000000000000000, 0.9953301976458442946, -0.09652874004297590238 ) ) ;
#4724 = DIRECTION ( 'NONE',  ( -3.491481338843133355E-15, 0.000000000000000000, -1.000000000000000000 ) ) ;
#4725 = LINE ( 'NONE', #6973, #10828 ) ;
#4726 = ORIENTED_EDGE ( 'NONE', *, *, #1365, .T. ) ;
#4727 = CARTESIAN_POINT ( 'NONE',  ( -56.99999999999997158, -1.184343223768575371, -3.558065644182727638 ) ) ;
#4728 = APPLICATION_CONTEXT ( 'automotive_design' ) ;
#4729 = CARTESIAN_POINT ( 'NONE',  ( 15.39414421509790287, -3.291455042465448511, 4.036171416105464260 ) ) ;
#4730 = DIRECTION ( 'NONE',  ( -1.000000000000000000, -3.054025858079668409E-16, 2.042474015755241579E-16 ) ) ;
#4731 = CARTESIAN_POINT ( 'NONE',  ( 51.80000000000002558, -3.933368109459642437, 2.186004417992994497 ) ) ;
#4732 = ADVANCED_FACE ( 'NONE', ( #25936 ), #18357, .T. ) ;
#4733 = CARTESIAN_POINT ( 'NONE',  ( -62.06576242361286688, -2.663271400516645127, 0.2033751180053996188 ) ) ;
#4735 = DIRECTION ( 'NONE',  ( 0.5633368246414943714, 0.8262273428075581627, 0.000000000000000000 ) ) ;
#4734 = FACE_OUTER_BOUND ( 'NONE', #744, .T. ) ;
#4736 = AXIS2_PLACEMENT_3D ( 'NONE', #28115, #25898, #13840 ) ;
#4737 = FACE_OUTER_BOUND ( 'NONE', #30449, .T. ) ;
#4739 = DIRECTION ( 'NONE',  ( 1.027984282060330001E-14, 0.000000000000000000, 1.000000000000000000 ) ) ;
#4738 = DIRECTION ( 'NONE',  ( 1.000000000000000000, 5.172273892338137201E-16, 0.000000000000000000 ) ) ;
#4740 = ORIENTED_EDGE ( 'NONE', *, *, #8840, .T. ) ;
#4741 = EDGE_CURVE ( 'NONE', #8527, #27612, #24662, .T. ) ;
#4742 = FACE_OUTER_BOUND ( 'NONE', #29851, .T. ) ;
#4743 = UNCERTAINTY_MEASURE_WITH_UNIT (LENGTH_MEASURE( 1.000000000000000082E-05 ), #18140, 'distance_accuracy_value', 'NONE');
#4744 = EDGE_CURVE ( 'NONE', #333, #20706, #77, .T. ) ;
#4745 = CARTESIAN_POINT ( 'NONE',  ( 60.97363240180332156, 0.7541976959284683035, 1.440084173506624321 ) ) ;
#4747 = DIRECTION ( 'NONE',  ( -1.000000000000000000, -0.000000000000000000, 3.491481338843133355E-15 ) ) ;
#4746 = DIRECTION ( 'NONE',  ( 3.491481338843133355E-15, 3.491481338843133355E-15, -1.000000000000000000 ) ) ;
#4749 = ADVANCED_FACE ( 'NONE', ( #26413 ), #17230, .T. ) ;
#4748 = CARTESIAN_POINT ( 'NONE',  ( -35.85663232820583346, 3.817150320979498357, 2.203324261493436520 ) ) ;
#4750 = ORIENTED_EDGE ( 'NONE', *, *, #27378, .T. ) ;
#4751 = AXIS2_PLACEMENT_3D ( 'NONE', #29252, #9485, #26407 ) ;
#4752 = ORIENTED_EDGE ( 'NONE', *, *, #29152, .F. ) ;
#4753 = CARTESIAN_POINT ( 'NONE',  ( 61.25000000000001421, 1.000000000000641709, -1.655766640117574795 ) ) ;
#4754 = ORIENTED_EDGE ( 'NONE', *, *, #20002, .T. ) ;
#4755 = CARTESIAN_POINT ( 'NONE',  ( 57.01810253486932112, 0.8103601741748552856, -2.470489098966295316 ) ) ;
#4756 = MANIFOLD_SOLID_BREP ( 'Stock-MAS-683-1', #4905 ) ;
#4757 = DIRECTION ( 'NONE',  ( -1.000000000000000000, -3.053848253006669023E-16, 2.042510438544995415E-16 ) ) ;
#4758 = ORIENTED_EDGE ( 'NONE', *, *, #27975, .F. ) ;
#4759 = CARTESIAN_POINT ( 'NONE',  ( -36.68866260399371271, -4.872353571451353282, -2.347449169364439925 ) ) ;
#4760 = ORIENTED_EDGE ( 'NONE', *, *, #5241, .T. ) ;
#4761 =( LENGTH_UNIT ( ) NAMED_UNIT ( * ) SI_UNIT ( .MILLI., .METRE. ) );
#4762 = CIRCLE ( 'NONE', #19449, 2.624999999999998668 ) ;
#4763 = EDGE_CURVE ( 'NONE', #6711, #18916, #31319, .T. ) ;
#4764 = CARTESIAN_POINT ( 'NONE',  ( -54.39999999999996305, 1.600000000000021627, -3.363870538531679610 ) ) ;
#4765 = VERTEX_POINT ( 'NONE', #19307 ) ;
#4766 = AXIS2_PLACEMENT_3D ( 'NONE', #20893, #30523, #13736 ) ;
#4767 = ORIENTED_EDGE ( 'NONE', *, *, #26690, .F. ) ;
#4768 = CARTESIAN_POINT ( 'NONE',  ( -55.38452994616205416, -3.117691453623976816, 1.799999999999791100 ) ) ;
#4769 = CARTESIAN_POINT ( 'NONE',  ( 50.49731030164353029, 0.9327905306641951499, 3.995066436131523346 ) ) ;
#4770 = CARTESIAN_POINT ( 'NONE',  ( 58.75000000000000711, 1.760622601997809955, -0.8948927608024527247 ) ) ;
#4771 = AXIS2_PLACEMENT_3D ( 'NONE', #15325, #1221, #5674 ) ;
#4772 = CARTESIAN_POINT ( 'NONE',  ( -54.45996984137642727, -1.500763111530254434, 3.300586169551323223 ) ) ;
#4773 = ADVANCED_FACE ( 'NONE', ( #134 ), #8729, .T. ) ;
#4774 = FACE_OUTER_BOUND ( 'NONE', #20120, .T. ) ;
#4776 = CARTESIAN_POINT ( 'NONE',  ( -36.92362342067168868, -0.1627367787821575318, -5.407318510437578496 ) ) ;
#4775 = DIRECTION ( 'NONE',  ( 1.000000000000000000, 3.054025858079668409E-16, -2.042474015755241579E-16 ) ) ;
#4777 = CIRCLE ( 'NONE', #27534, 4.099999999999992539 ) ;
#4778 = AXIS2_PLACEMENT_3D ( 'NONE', #7989, #19867, #24604 ) ;
#4779 = CARTESIAN_POINT ( 'NONE',  ( 58.75000000000002132, 6.153735859711025284E-13, 3.111507638930570854E-58 ) ) ;
#4781 = DIRECTION ( 'NONE',  ( -1.000000000000000000, -3.054025858079668409E-16, 2.042474015755241579E-16 ) ) ;
#4780 = CARTESIAN_POINT ( 'NONE',  ( 58.75000000000002842, -1.039502773796102897, -1.800471618824325493 ) ) ;
#4782 = ORIENTED_EDGE ( 'NONE', *, *, #10819, .T. ) ;
#4783 = ADVANCED_FACE ( 'NONE', ( #10569 ), #10713, .T. ) ;
#4784 = CARTESIAN_POINT ( 'NONE',  ( 60.75000000000001421, 0.5000000000006363798, -1.863080903343375061 ) ) ;
#4785 = EDGE_CURVE ( 'NONE', #28051, #107, #1596, .T. ) ;
#4786 = AXIS2_PLACEMENT_3D ( 'NONE', #921, #10407, #20401 ) ;
#4787 = LINE ( 'NONE', #8906, #1711 ) ;
#4789 = CARTESIAN_POINT ( 'NONE',  ( 50.40671278470074412, -1.343285922954033040, 3.873819829599201015 ) ) ;
#4788 = CARTESIAN_POINT ( 'NONE',  ( 48.43389689255278796, -1.399562922973020429, 3.853849143137397792 ) ) ;
#4791 = EDGE_CURVE ( 'NONE', #585, #8786, #7151, .T. ) ;
#4790 = DIRECTION ( 'NONE',  ( 0.000000000000000000, -0.7438053426816512159, -0.6683962987616188789 ) ) ;
#4792 = ORIENTED_EDGE ( 'NONE', *, *, #20393, .T. ) ;
#4793 = CYLINDRICAL_SURFACE ( 'NONE', #30152, 4.375000000000000000 ) ;
#4794 = EDGE_LOOP ( 'NONE', ( #11511, #7083, #6770 ) ) ;
#4795 = CIRCLE ( 'NONE', #23514, 2.750000000000000000 ) ;
#4796 = CARTESIAN_POINT ( 'NONE',  ( 28.63101374161908552, 6.274379892050021112, 1.424999999999900346 ) ) ;
#4797 = CARTESIAN_POINT ( 'NONE',  ( -56.69702994616203284, -2.078460969082631227, -3.600000000000207923 ) ) ;
#4798 = ORIENTED_EDGE ( 'NONE', *, *, #3216, .F. ) ;
#4799 = VERTEX_POINT ( 'NONE', #7862 ) ;
#4800 = CARTESIAN_POINT ( 'NONE',  ( 15.61033468494287391, 4.977801270594249594, 2.126472881633401091 ) ) ;
#4801 = VERTEX_POINT ( 'NONE', #15636 ) ;
#4802 = CARTESIAN_POINT ( 'NONE',  ( 52.05052023551990459, 4.366200217884951940, 1.447862837342193565 ) ) ;
#4803 = CARTESIAN_POINT ( 'NONE',  ( -56.94702994616206126, -2.078460969082657872, 3.599999999999789591 ) ) ;
#4804 = ORIENTED_EDGE ( 'NONE', *, *, #10429, .F. ) ;
#4805 = FACE_OUTER_BOUND ( 'NONE', #12100, .T. ) ;
#4806 = CARTESIAN_POINT ( 'NONE',  ( -35.85663232820584057, -4.945493884734809775, 1.606888370749721684 ) ) ;
#4807 = AXIS2_PLACEMENT_3D ( 'NONE', #9235, #23954, #20953 ) ;
#4808 = CARTESIAN_POINT ( 'NONE',  ( 31.46392738815476164, 7.544460793879348870, 2.049999999999889688 ) ) ;
#4809 = VERTEX_POINT ( 'NONE', #3276 ) ;
#4810 = B_SPLINE_CURVE_WITH_KNOTS ( 'NONE', 3,
 ( #14608, #17156, #24274, #4632, #14902, #2586 ),
 .UNSPECIFIED., .F., .F.,
 ( 4, 2, 4 ),
 ( 0.000000000000000000, 0.0001000270069604664605, 0.0002000540139209329210 ),
 .UNSPECIFIED. ) ;
#4811 = CARTESIAN_POINT ( 'NONE',  ( -59.29999999999997584, 2.330309927981285032E-15, 4.253626757584724400E-16 ) ) ;
#4812 = CARTESIAN_POINT ( 'NONE',  ( 53.76063741390512973, 7.747904304409473752, -2.050000000000187228 ) ) ;
#4814 = CARTESIAN_POINT ( 'NONE',  ( 50.59602332238209499, 0.1408342061609076379, -0.8215393206232032286 ) ) ;
#4813 = AXIS2_PLACEMENT_3D ( 'NONE', #1178, #20518, #25248 ) ;
#4815 = ORIENTED_EDGE ( 'NONE', *, *, #4331, .F. ) ;
#4816 = DIRECTION ( 'NONE',  ( 0.000000000000000000, 1.000000000000000000, 0.000000000000000000 ) ) ;
#4817 = EDGE_CURVE ( 'NONE', #11068, #29981, #8929, .T. ) ;
#4818 = CARTESIAN_POINT ( 'NONE',  ( 57.00000000000001421, 0.000000000000000000, 0.000000000000000000 ) ) ;
#4819 = EDGE_CURVE ( 'NONE', #17369, #4543, #28891, .T. ) ;
#4820 = VECTOR ( 'NONE', #21388, 1000.000000000000000 ) ;
#4821 = EDGE_CURVE ( 'NONE', #27463, #2662, #15221, .T. ) ;
#4823 = FACE_OUTER_BOUND ( 'NONE', #2485, .T. ) ;
#4822 = DIRECTION ( 'NONE',  ( 1.000000000000000000, 3.054025858079668409E-16, -2.042474015755241579E-16 ) ) ;
#4824 = DIRECTION ( 'NONE',  ( -1.000000000000000000, 0.000000000000000000, 1.047444401652940007E-14 ) ) ;
#4825 = CARTESIAN_POINT ( 'NONE',  ( 69.23535533905938166, 4.557543281186736018E-17, 2.764644660939941101 ) ) ;
#4826 = VERTEX_POINT ( 'NONE', #17540 ) ;
#4827 = CIRCLE ( 'NONE', #9897, 3.675000000000000711 ) ;
#4828 = VECTOR ( 'NONE', #28314, 1000.000000000000000 ) ;
#4829 = AXIS2_PLACEMENT_3D ( 'NONE', #28719, #26482, #21604 ) ;
#4830 = ORIENTED_EDGE ( 'NONE', *, *, #14813, .T. ) ;
#4831 = FACE_OUTER_BOUND ( 'NONE', #29175, .T. ) ;
#4832 = ORIENTED_EDGE ( 'NONE', *, *, #20783, .F. ) ;
#4833 = DIRECTION ( 'NONE',  ( 0.000000000000000000, 0.000000000000000000, -1.000000000000000000 ) ) ;
#4834 = CARTESIAN_POINT ( 'NONE',  ( -60.28335481156722864, 0.8699069336946685382, -4.241846523238430144 ) ) ;
#4836 = DIRECTION ( 'NONE',  ( 1.000000000000000000, 1.047444401652940007E-14, 0.000000000000000000 ) ) ;
#4835 = CARTESIAN_POINT ( 'NONE',  ( -54.49999999999997868, 8.366749974758391359E-15, -1.938977325913827332E-13 ) ) ;
#4837 = ORIENTED_EDGE ( 'NONE', *, *, #9226, .F. ) ;
#4838 = CIRCLE ( 'NONE', #16483, 0.2500000000000000000 ) ;
#4839 = ORIENTED_EDGE ( 'NONE', *, *, #8216, .T. ) ;
#4840 = DIRECTION ( 'NONE',  ( 1.000000000000000000, -0.000000000000000000, -1.047444401652940007E-14 ) ) ;
#4841 = VERTEX_POINT ( 'NONE', #1063 ) ;
#4842 = CIRCLE ( 'NONE', #5836, 0.2500000000000000000 ) ;
#4843 = CARTESIAN_POINT ( 'NONE',  ( 68.00000000000000000, 0.7500000000000000000, -1.988246715074068582 ) ) ;
#4844 = VERTEX_POINT ( 'NONE', #3121 ) ;
#4845 = CARTESIAN_POINT ( 'NONE',  ( -36.81959771849334828, 4.939398376933260337, 2.210903708596522410 ) ) ;
#4846 = STYLED_ITEM ( 'NONE', ( #932 ), #25183 ) ;
#4847 = VERTEX_POINT ( 'NONE', #916 ) ;
#4848 = CARTESIAN_POINT ( 'NONE',  ( -62.04999999999998295, 1.183285843523195887E-15, 2.187514201909070562E-15 ) ) ;
#4849 = CARTESIAN_POINT ( 'NONE',  ( 52.08333333333335702, 4.368973594129894167, 1.439468559502539824 ) ) ;
#4850 = CARTESIAN_POINT ( 'NONE',  ( 33.47623932017462778, -2.199885893005940840, 4.939696249117685234 ) ) ;
#4851 = CARTESIAN_POINT ( 'NONE',  ( -55.39405989232414385, -3.920666489018348300E-15, 3.399999999999801847 ) ) ;
#4852 = CARTESIAN_POINT ( 'NONE',  ( 58.75000000000003553, -1.791164585742486937, -0.8897917884440847969 ) ) ;
#4853 = ADVANCED_FACE ( 'NONE', ( #20396 ), #23325, .F. ) ;
#4854 = CIRCLE ( 'NONE', #10903, 0.1500000000000001887 ) ;
#4855 = ADVANCED_FACE ( 'NONE', ( #3594 ), #27334, .T. ) ;
#4856 = AXIS2_PLACEMENT_3D ( 'NONE', #28859, #26634, #7171 ) ;
#4857 = CARTESIAN_POINT ( 'NONE',  ( 65.05000000000005400, -1.025519176787267142E-28, 4.049999999999318590 ) ) ;
#4858 = AXIS2_PLACEMENT_3D ( 'NONE', #11044, #1212, #30495 ) ;
#4859 = CIRCLE ( 'NONE', #24560, 0.7500000000000001110 ) ;
#4860 = DIRECTION ( 'NONE',  ( -1.000000000000000000, -3.053848253006669023E-16, 2.042510438544995415E-16 ) ) ;
#4861 = AXIS2_PLACEMENT_3D ( 'NONE', #18898, #23956, #16205 ) ;
#4862 = VERTEX_POINT ( 'NONE', #11971 ) ;
#4863 = AXIS2_PLACEMENT_3D ( 'NONE', #29333, #21923, #202 ) ;
#4864 = CARTESIAN_POINT ( 'NONE',  ( -36.40793637698146057, -0.9785522574022036402, 5.318456145981289573 ) ) ;
#4865 = ORIENTED_EDGE ( 'NONE', *, *, #26519, .F. ) ;
#4866 = DIRECTION ( 'NONE',  ( 0.000000000000000000, 0.000000000000000000, 1.000000000000000000 ) ) ;
#4867 = CARTESIAN_POINT ( 'NONE',  ( 58.66107449606997193, 1.349793924523127187, -1.301839550767805331 ) ) ;
#4868 = CARTESIAN_POINT ( 'NONE',  ( 53.90826136769680943, 6.078611636103663507, 1.730551604087905204 ) ) ;
#4869 = ORIENTED_EDGE ( 'NONE', *, *, #23870, .T. ) ;
#4870 = ADVANCED_FACE ( 'NONE', ( #16884 ), #17051, .T. ) ;
#4871 = CARTESIAN_POINT ( 'NONE',  ( -54.49983703358571319, 1.542636180423125225, 4.059406436927349482 ) ) ;
#4872 = ORIENTED_EDGE ( 'NONE', *, *, #25274, .F. ) ;
#4873 = CIRCLE ( 'NONE', #8419, 0.04999999999999987094 ) ;
#4874 = CARTESIAN_POINT ( 'NONE',  ( 15.68751737981905947, 0.3564988296781282928, -5.398869307934854866 ) ) ;
#4876 = LINE ( 'NONE', #14541, #9630 ) ;
#4875 = CARTESIAN_POINT ( 'NONE',  ( 51.35976194839694386, -4.327157167232345003, -1.563052875988793611 ) ) ;
#4877 = ORIENTED_EDGE ( 'NONE', *, *, #22395, .F. ) ;
#4878 = AXIS2_PLACEMENT_3D ( 'NONE', #28110, #4781, #9125 ) ;
#4879 = FACE_OUTER_BOUND ( 'NONE', #5294, .T. ) ;
#4880 = CARTESIAN_POINT ( 'NONE',  ( 68.00000000000001421, 5.529431079676072613E-15, -7.122621931239992550E-13 ) ) ;
#4881 = AXIS2_PLACEMENT_3D ( 'NONE', #15224, #22837, #8559 ) ;
#4883 = CARTESIAN_POINT ( 'NONE',  ( -54.49608498031047787, -1.530604779201329535, -4.051096982736679841 ) ) ;
#4882 = CARTESIAN_POINT ( 'NONE',  ( 58.75000000000002132, 6.153735859711025284E-13, 3.111507638930570854E-58 ) ) ;
#4884 = ORIENTED_EDGE ( 'NONE', *, *, #25906, .T. ) ;
#4885 = CARTESIAN_POINT ( 'NONE',  ( -58.68749999999997158, -4.108500314926507357, 1.367561758111406789 ) ) ;
#4886 = CARTESIAN_POINT ( 'NONE',  ( -63.82928932188132620, 6.399178848011186396E-16, 2.550935903222500290E-15 ) ) ;
#4887 = FACE_OUTER_BOUND ( 'NONE', #21748, .T. ) ;
#4888 = AXIS2_PLACEMENT_3D ( 'NONE', #9852, #26644, #14752 ) ;
#4889 = CARTESIAN_POINT ( 'NONE',  ( 51.80000000000003268, 6.982261990806648555E-14, 4.599999999999857536 ) ) ;
#4890 = DIRECTION ( 'NONE',  ( -1.000000000000000000, -0.000000000000000000, -0.000000000000000000 ) ) ;
#4891 = TOROIDAL_SURFACE ( 'NONE', #12974, 4.199999999999993072, 0.1000000000000000056 ) ;
#4892 = TOROIDAL_SURFACE ( 'NONE', #14524, 1.975000000000001865, 0.1000000000000000056 ) ;
#4893 = FACE_OUTER_BOUND ( 'NONE', #12551, .T. ) ;
#4894 = ORIENTED_EDGE ( 'NONE', *, *, #13577, .F. ) ;
#4895 = ADVANCED_FACE ( 'NONE', ( #14180 ), #4105, .T. ) ;
#4896 = DIRECTION ( 'NONE',  ( 1.000000000000000000, 1.047444401652940007E-14, 0.000000000000000000 ) ) ;
#4897 = DIRECTION ( 'NONE',  ( 0.7071067811865534569, 0.1420552074174021573, -0.6926906366088618761 ) ) ;
#4898 = AXIS2_PLACEMENT_3D ( 'NONE', #6398, #21575, #11143 ) ;
#4899 = CARTESIAN_POINT ( 'NONE',  ( 23.02167883289836681, 6.240626183124143189, -1.950000000000080558 ) ) ;
#4900 = CIRCLE ( 'NONE', #27665, 1.975000000000001865 ) ;
#4901 = CARTESIAN_POINT ( 'NONE',  ( -62.05303033788776190, -2.687940397879565513, 0.2501026294260040861 ) ) ;
#4902 = AXIS2_PLACEMENT_3D ( 'NONE', #6658, #30397, #16320 ) ;
#4904 = CARTESIAN_POINT ( 'NONE',  ( 53.35463186488154008, 7.923732722238535864, -1.887452792520897704 ) ) ;
#4903 = CARTESIAN_POINT ( 'NONE',  ( -62.06974646775923787, -2.693531034594032203, 0.1939937330634021184 ) ) ;
#4905 = CLOSED_SHELL ( 'NONE', ( #16569, #14887, #7630, #18173, #29915, #14900, #25480, #971, #3104, #4749, #6069, #18994, #27414, #14476, #17598, #6299, #29577, #9466, #16673, #23950, #30272, #24587, #24972, #24022, #14387, #8811, #1780, #30895, #23989, #18516, #15614, #24209, #15044, #8851, #22821, #4434, #27075, #4466, #29355, #7194, #13533, #14774, #4468, #19070, #22025, #11347, #7135, #26636, #27703, #17566, #22039, #904, #12240, #12061, #1344, #17033, #15188, #8331, #24932, #27519, #25159, #20464, #26612, #9484, #7711, #8771, #17359, #28125, #7481, #16274, #17305, #15132, #12604, #7704, #5784, #23294, #17435, #13081, #24680, #25048, #4174, #8879, #2970, #27983, #17950, #25120, #13264, #20665, #12324, #25310, #8848, #26626, #15233, #31214, #12937, #21898, #10590 ) ) ;
#4906 = DIRECTION ( 'NONE',  ( -1.000000000000000000, -3.054025858079668409E-16, 2.042474015755241579E-16 ) ) ;
#4907 = CIRCLE ( 'NONE', #3812, 0.7500000000000002220 ) ;
#4909 = CARTESIAN_POINT ( 'NONE',  ( 22.20257169554298216, 7.242789023567402396, 1.424999999999922995 ) ) ;
#4908 = CARTESIAN_POINT ( 'NONE',  ( 51.35185081662972095, -3.852602532216165887, 1.405026670785422871 ) ) ;
#4910 = ORIENTED_EDGE ( 'NONE', *, *, #4673, .T. ) ;
#4911 = ADVANCED_FACE ( 'NONE', ( #238 ), #19273, .F. ) ;
#4912 = CARTESIAN_POINT ( 'NONE',  ( 58.72200624034184102, -1.816790722507359179, 0.4641018782093048189 ) ) ;
#4913 = CIRCLE ( 'NONE', #22636, 0.05000000000000012768 ) ;
#4914 = DIRECTION ( 'NONE',  ( -1.000000000000000000, -3.054025858079668409E-16, 2.042474015755241579E-16 ) ) ;
#4916 = CARTESIAN_POINT ( 'NONE',  ( 58.68279620299891519, -0.4999999999993856026, -1.809045707182514118 ) ) ;
#4915 = DIRECTION ( 'NONE',  ( -3.491481338843133355E-15, -3.491481338843133355E-15, 1.000000000000000000 ) ) ;
#4917 = DIRECTION ( 'NONE',  ( 1.000000000000000000, 0.000000000000000000, 0.000000000000000000 ) ) ;
#4918 = ORIENTED_EDGE ( 'NONE', *, *, #28677, .F. ) ;
#4919 = ORIENTED_EDGE ( 'NONE', *, *, #6181, .T. ) ;
#4920 = DIRECTION ( 'NONE',  ( 0.000000000000000000, 0.000000000000000000, -1.000000000000000000 ) ) ;
#4921 = ORIENTED_EDGE ( 'NONE', *, *, #909, .F. ) ;
#4922 = DIRECTION ( 'NONE',  ( 0.000000000000000000, 0.000000000000000000, 1.000000000000000000 ) ) ;
#4923 = CARTESIAN_POINT ( 'NONE',  ( -71.44999999999998863, -1.380331489585512972E-15, 2.906968604901091669E-15 ) ) ;
#4924 = AXIS2_PLACEMENT_3D ( 'NONE', #28451, #31133, #4542 ) ;
#4925 = VERTEX_POINT ( 'NONE', #2476 ) ;
#4926 = DIRECTION ( 'NONE',  ( 0.000000000000000000, 0.000000000000000000, 1.000000000000000000 ) ) ;
#4927 = ORIENTED_EDGE ( 'NONE', *, *, #4985, .T. ) ;
#4928 =( NAMED_UNIT ( * ) SI_UNIT ( $, .STERADIAN. ) SOLID_ANGLE_UNIT ( ) );
#4929 = CIRCLE ( 'NONE', #3928, 3.625000000000024869 ) ;
#4930 = DIRECTION ( 'NONE',  ( 0.000000000000000000, 0.000000000000000000, 1.000000000000000000 ) ) ;
#4931 = VERTEX_POINT ( 'NONE', #31286 ) ;
#4932 = CIRCLE ( 'NONE', #25130, 2.874999999999999112 ) ;
#4933 = SURFACE_SIDE_STYLE ('',( #5392 ) ) ;
#4934 = ORIENTED_EDGE ( 'NONE', *, *, #8258, .F. ) ;
#4935 = AXIS2_PLACEMENT_3D ( 'NONE', #10870, #15473, #13382 ) ;
#4936 = ADVANCED_FACE ( 'NONE', ( #26377 ), #97, .T. ) ;
#4937 = CARTESIAN_POINT ( 'NONE',  ( -59.32202994616204705, 2.078460969082646770, 3.599999999999797140 ) ) ;
#4938 = AXIS2_PLACEMENT_3D ( 'NONE', #16567, #16875, #31277 ) ;
#4939 = CARTESIAN_POINT ( 'NONE',  ( 52.98705886115021002, 8.418976914897422503, -2.050000000000184563 ) ) ;
#4940 = DIRECTION ( 'NONE',  ( 0.000000000000000000, 0.000000000000000000, 1.000000000000000000 ) ) ;
#4942 = ADVANCED_FACE ( 'NONE', ( #12268 ), #9903, .F. ) ;
#4941 = CARTESIAN_POINT ( 'NONE',  ( -54.44999999999997442, -1.500000000000000000, 3.300094695611020867 ) ) ;
#4943 = CARTESIAN_POINT ( 'NONE',  ( -60.58528264635176441, -2.480971988140598050, -1.067472133821737446 ) ) ;
#4945 = CARTESIAN_POINT ( 'NONE',  ( -36.89017861347081606, -0.3252614978953602964, -5.399488438498864618 ) ) ;
#4944 = CARTESIAN_POINT ( 'NONE',  ( 61.23770293222972327, 0.8897917884438596436, 1.791164585743606041 ) ) ;
#4946 = CIRCLE ( 'NONE', #908, 3.625000000000024869 ) ;
#4947 = CIRCLE ( 'NONE', #3441, 3.648039984012787507 ) ;
#4948 =( NAMED_UNIT ( * ) SI_UNIT ( $, .STERADIAN. ) SOLID_ANGLE_UNIT ( ) );
#4949 = CARTESIAN_POINT ( 'NONE',  ( 15.70940947763171280, -2.412550141807447091, 4.840569432287336049 ) ) ;
#4951 = DIRECTION ( 'NONE',  ( 1.000000000000000000, 1.047444401652940007E-14, 0.000000000000000000 ) ) ;
#4950 = DIRECTION ( 'NONE',  ( 0.000000000000000000, -0.2008964009354148039, 0.9796124928211140670 ) ) ;
#4952 = ORIENTED_EDGE ( 'NONE', *, *, #2601, .T. ) ;
#4953 = ADVANCED_FACE ( 'NONE', ( #4996 ), #10063, .F. ) ;
#4955 = CARTESIAN_POINT ( 'NONE',  ( 15.03925126672133139, -4.817150320980666756, 2.203324261490539282 ) ) ;
#4954 = CIRCLE ( 'NONE', #7987, 1.000000000000000000 ) ;
#4956 = CARTESIAN_POINT ( 'NONE',  ( -36.14490256869204643, -4.698781674909506378, -2.676750094560167881 ) ) ;
#4958 = DIRECTION ( 'NONE',  ( -1.000000000000000000, -3.054025858079668409E-16, 2.042474015755241579E-16 ) ) ;
#4957 = FACE_OUTER_BOUND ( 'NONE', #7909, .T. ) ;
#4959 = FACE_OUTER_BOUND ( 'NONE', #16370, .T. ) ;
#4960 = ORIENTED_EDGE ( 'NONE', *, *, #1864, .T. ) ;
#4961 = FACE_OUTER_BOUND ( 'NONE', #22319, .T. ) ;
#4962 = VERTEX_POINT ( 'NONE', #11811 ) ;
#4963 = CARTESIAN_POINT ( 'NONE',  ( 65.00000000000005684, 5.021051876503122852E-16, 4.099999999999319300 ) ) ;
#4964 = CARTESIAN_POINT ( 'NONE',  ( -57.07202994616206126, 2.078460969082646770, 3.599999999999804690 ) ) ;
#4965 = VERTEX_POINT ( 'NONE', #7072 ) ;
#4966 = ADVANCED_FACE ( 'NONE', ( #5147 ), #29538, .T. ) ;
#4967 = ORIENTED_EDGE ( 'NONE', *, *, #6983, .T. ) ;
#4968 = CARTESIAN_POINT ( 'NONE',  ( -54.49999999999997868, 3.673546848079182858, 0.7533615035078058408 ) ) ;
#4969 = ORIENTED_EDGE ( 'NONE', *, *, #26248, .F. ) ;
#4970 = LINE ( 'NONE', #29342, #19734 ) ;
#4971 = CARTESIAN_POINT ( 'NONE',  ( -55.88452994616203995, 2.093608279459368564E-14, -3.600000000000198597 ) ) ;
#4972 = ORIENTED_EDGE ( 'NONE', *, *, #5136, .F. ) ;
#4973 = DIRECTION ( 'NONE',  ( 1.000000000000000000, 3.125586771759065906E-16, 0.000000000000000000 ) ) ;
#4974 = CARTESIAN_POINT ( 'NONE',  ( 65.00000000000007105, 4.867971026610729436E-16, 3.949999999999319389 ) ) ;
#4975 = B_SPLINE_CURVE_WITH_KNOTS ( 'NONE', 3,
 ( #21127, #2090, #30759, #30914 ),
 .UNSPECIFIED., .F., .F.,
 ( 4, 4 ),
 ( 0.000000000000000000, 0.0003819718307412712306 ),
 .UNSPECIFIED. ) ;
#4976 = CARTESIAN_POINT ( 'NONE',  ( 31.37624803156852948, 7.388935656075745761, 2.049999999999763567 ) ) ;
#4977 = VERTEX_POINT ( 'NONE', #24457 ) ;
#4978 = AXIS2_PLACEMENT_3D ( 'NONE', #73, #2275, #11940 ) ;
#4979 = EDGE_CURVE ( 'NONE', #19242, #9490, #7807, .T. ) ;
#4980 = CARTESIAN_POINT ( 'NONE',  ( -77.29999999999998295, -0.2599193648183464878, -0.006474858487185622576 ) ) ;
#4981 = EDGE_CURVE ( 'NONE', #25975, #1935, #19962, .T. ) ;
#4982 = DIRECTION ( 'NONE',  ( 0.000000000000000000, 0.000000000000000000, -1.000000000000000000 ) ) ;
#4983 = CARTESIAN_POINT ( 'NONE',  ( 50.56925576102500486, -0.1015751161694646437, -0.8011113709441625153 ) ) ;
#4985 = EDGE_CURVE ( 'NONE', #14659, #6036, #9850, .T. ) ;
#4984 = CARTESIAN_POINT ( 'NONE',  ( -59.62499999999996447, 2.944486372867118895, -1.700000000000178924 ) ) ;
#4986 = CARTESIAN_POINT ( 'NONE',  ( 57.04458252721509126, -0.7500000000000000000, 2.421260002560649660 ) ) ;
#4988 = LINE ( 'NONE', #14643, #5804 ) ;
#4987 = DIRECTION ( 'NONE',  ( 0.000000000000000000, 0.000000000000000000, 1.000000000000000000 ) ) ;
#4989 = CARTESIAN_POINT ( 'NONE',  ( 51.80576158887517835, -4.272136569073781587, 0.9439330974870294710 ) ) ;
#4990 = FACE_OUTER_BOUND ( 'NONE', #23126, .T. ) ;
#4991 = CARTESIAN_POINT ( 'NONE',  ( 53.49139514279634966, 5.155866831720416599, 2.049999999999812861 ) ) ;
#4992 = ORIENTED_EDGE ( 'NONE', *, *, #29132, .F. ) ;
#4993 = ORIENTED_EDGE ( 'NONE', *, *, #1270, .F. ) ;
#4994 = AXIS2_PLACEMENT_3D ( 'NONE', #9720, #28398, #16362 ) ;
#4995 = ORIENTED_EDGE ( 'NONE', *, *, #29706, .T. ) ;
#4996 = FACE_OUTER_BOUND ( 'NONE', #3448, .T. ) ;
#4997 = CARTESIAN_POINT ( 'NONE',  ( -55.92292740578360366, 2.256877952708269408, -2.542931754211925632 ) ) ;
#4999 = CARTESIAN_POINT ( 'NONE',  ( 58.75000000000002842, -0.8897917884436052915, -1.791164585742600179 ) ) ;
#4998 = CARTESIAN_POINT ( 'NONE',  ( -54.62499999999997158, -2.944486372867076707, -1.700000000000204903 ) ) ;
#5000 = EDGE_LOOP ( 'NONE', ( #28846, #23493, #15348, #28122 ) ) ;
#5001 = EDGE_CURVE ( 'NONE', #20368, #25749, #26565, .T. ) ;
#5002 = VERTEX_POINT ( 'NONE', #25242 ) ;
#5003 = DIRECTION ( 'NONE',  ( 1.000000000000000000, -0.000000000000000000, -0.000000000000000000 ) ) ;
#5004 = ORIENTED_EDGE ( 'NONE', *, *, #12849, .F. ) ;
#5005 = CARTESIAN_POINT ( 'NONE',  ( 33.05069135236684019, 8.148093138862860130, -1.950000000000114531 ) ) ;
#5006 = ORIENTED_EDGE ( 'NONE', *, *, #9302, .F. ) ;
#5007 = CARTESIAN_POINT ( 'NONE',  ( 32.57869118518439677, 7.908463454149920580, -2.050000000000176570 ) ) ;
#5008 = EDGE_CURVE ( 'NONE', #1696, #14148, #14947, .T. ) ;
#5009 = EDGE_LOOP ( 'NONE', ( #28883, #14456, #9053, #30097 ) ) ;
#5010 = LINE ( 'NONE', #14668, #5066 ) ;
#5011 = CARTESIAN_POINT ( 'NONE',  ( 57.03577985506672832, 0.7479400494557524315, 1.780189605359982608 ) ) ;
#5012 = B_SPLINE_CURVE_WITH_KNOTS ( 'NONE', 3,
 ( #19136, #28457, #28776, #2323, #23400, #13861, #2013, #6760, #16420, #21356 ),
 .UNSPECIFIED., .F., .F.,
 ( 4, 2, 2, 2, 4 ),
 ( 0.000000000000000000, 0.0003601004132760236712, 0.0007202008265520473424, 0.001080301239828071122, 0.001440401653104094685 ),
 .UNSPECIFIED. ) ;
#5013 = CARTESIAN_POINT ( 'NONE',  ( -55.01905989232411542, 2.023778652682504950E-14, -3.400000000000195310 ) ) ;
#5015 = EDGE_CURVE ( 'NONE', #1037, #27051, #3563, .T. ) ;
#5014 = CARTESIAN_POINT ( 'NONE',  ( 52.82099478266073334, 4.588601447596447613, -1.578939844535521386 ) ) ;
#5016 =( GEOMETRIC_REPRESENTATION_CONTEXT ( 3 ) GLOBAL_UNCERTAINTY_ASSIGNED_CONTEXT ( ( #7287 ) ) GLOBAL_UNIT_ASSIGNED_CONTEXT ( ( #16339, #1753, #16184 ) ) REPRESENTATION_CONTEXT ( 'NONE', 'WORKASPACE' ) );
#5017 = AXIS2_PLACEMENT_3D ( 'NONE', #25625, #953, #20746 ) ;
#5018 = FACE_OUTER_BOUND ( 'NONE', #19394, .T. ) ;
#5019 = DIRECTION ( 'NONE',  ( 3.384826294588897856E-15, -8.881784197001252323E-16, 1.000000000000000000 ) ) ;
#5020 = CARTESIAN_POINT ( 'NONE',  ( 15.97944027357902819, -4.944296796129584948, -2.193698057025752490 ) ) ;
#5021 = DIRECTION ( 'NONE',  ( -1.000000000000000000, -3.053848253006669023E-16, 2.042510438544995415E-16 ) ) ;
#5022 = B_SPLINE_CURVE_WITH_KNOTS ( 'NONE', 3,
 ( #24847, #9404, #19957, #22193, #3013, #7914, #14873, #19073, #12504, #12655 ),
 .UNSPECIFIED., .F., .F.,
 ( 4, 2, 2, 2, 4 ),
 ( 0.000000000000000000, 0.0003926182454497119476, 0.0007852364908994238953, 0.001177854736349135843, 0.001570472981798847791 ),
 .UNSPECIFIED. ) ;
#5023 = AXIS2_PLACEMENT_3D ( 'NONE', #15767, #10700, #22901 ) ;
#5024 = ORIENTED_EDGE ( 'NONE', *, *, #24099, .T. ) ;
#5026 = DIRECTION ( 'NONE',  ( 1.000000000000000000, 0.000000000000000000, 0.000000000000000000 ) ) ;
#5025 = CARTESIAN_POINT ( 'NONE',  ( -36.92362342067078629, -3.309998894527926172, -4.278958290368498396 ) ) ;
#5027 = FACE_OUTER_BOUND ( 'NONE', #2966, .T. ) ;
#5028 = EDGE_LOOP ( 'NONE', ( #31262, #16063, #18258, #23587 ) ) ;
#5029 = CARTESIAN_POINT ( 'NONE',  ( -61.39999999999998437, 1.381785979968628826E-15, 2.054751023403646402E-15 ) ) ;
#5030 = AXIS2_PLACEMENT_3D ( 'NONE', #11374, #4247, #11552 ) ;
#5031 = ORIENTED_EDGE ( 'NONE', *, *, #19144, .F. ) ;
#5032 = CARTESIAN_POINT ( 'NONE',  ( 15.61033468494287924, 0.4841707035674313042, -5.391286593723154219 ) ) ;
#5033 = CARTESIAN_POINT ( 'NONE',  ( -36.58361892166016816, -5.109611055794880841, 1.772889539330528619 ) ) ;
#5035 = FACE_OUTER_BOUND ( 'NONE', #12205, .T. ) ;
#5034 = CARTESIAN_POINT ( 'NONE',  ( 58.75000000000000711, 1.470078920827434965, 1.470078920828533420 ) ) ;
#5036 = ORIENTED_EDGE ( 'NONE', *, *, #350, .T. ) ;
#5037 = ADVANCED_FACE ( 'NONE', ( #29680 ), #15116, .F. ) ;
#5038 = CARTESIAN_POINT ( 'NONE',  ( 58.50000000000001421, -0.8000000000000000444, -2.421260002560649660 ) ) ;
#5039 = LINE ( 'NONE', #4889, #4820 ) ;
#5040 = EDGE_CURVE ( 'NONE', #21318, #17938, #2249, .T. ) ;
#5041 = AXIS2_PLACEMENT_3D ( 'NONE', #440, #12015, #19771 ) ;
#5042 = CARTESIAN_POINT ( 'NONE',  ( -54.39999999999996305, -1.399999999999981037, -3.363870538531691157 ) ) ;
#5043 = AXIS2_PLACEMENT_3D ( 'NONE', #9381, #21753, #31233 ) ;
#5045 = CARTESIAN_POINT ( 'NONE',  ( -54.49999999999997868, -1.549598385535858380, -4.064203588144675194 ) ) ;
#5044 = DIRECTION ( 'NONE',  ( 2.477824476393711885E-12, -0.8914544820231923294, -0.4531102586355355011 ) ) ;
#5046 = EDGE_CURVE ( 'NONE', #4604, #3896, #4777, .T. ) ;
#5047 = EDGE_LOOP ( 'NONE', ( #2585, #2401, #15070, #27283, #20892, #13162, #26022, #2447, #9939, #12246, #25982, #22277, #30857, #28564, #21150, #18575, #25722, #1671, #16223, #177, #14264, #25322 ) ) ;
#5048 = CARTESIAN_POINT ( 'NONE',  ( -60.74999999999996447, -1.184343223768586251, -3.558065644182722753 ) ) ;
#5049 = CARTESIAN_POINT ( 'NONE',  ( 61.23770293223015670, -0.8897917884444476178, 1.791164585743103999 ) ) ;
#5050 = CARTESIAN_POINT ( 'NONE',  ( 52.20711756518983293, 0.5000000000005468959, -1.807104036850122109 ) ) ;
#5051 = CARTESIAN_POINT ( 'NONE',  ( 69.20000000000003126, 5.529431079676072613E-15, -7.248315259438346108E-13 ) ) ;
#5052 = AXIS2_PLACEMENT_3D ( 'NONE', #23868, #7386, #19431 ) ;
#5053 = CARTESIAN_POINT ( 'NONE',  ( -54.49999999999994316, -0.7277771693817812748, -3.394129477159102404 ) ) ;
#5054 = CARTESIAN_POINT ( 'NONE',  ( -58.02900635094607651, 3.400000000000002576, 0.9110272542656318029 ) ) ;
#5055 = DIRECTION ( 'NONE',  ( -1.000000000000000000, -3.054027077731387480E-16, 2.042479963029832083E-16 ) ) ;
#5056 = ORIENTED_EDGE ( 'NONE', *, *, #5838, .T. ) ;
#5057 = ADVANCED_FACE ( 'NONE', ( #22407 ), #22733, .T. ) ;
#5058 = CARTESIAN_POINT ( 'NONE',  ( 15.57907767661756360, -3.590618801409561911, 4.051716037497246070 ) ) ;
#5059 =( BOUNDED_SURFACE ( )  B_SPLINE_SURFACE ( 3, 2, ( 
 ( #12158, #21840, #31153 ),
 ( #14682, #24343, #5176 ),
 ( #21977, #7102, #269 ),
 ( #2174, #2794, #21516 ) ),
 .UNSPECIFIED., .F., .F., .F. ) 
 B_SPLINE_SURFACE_WITH_KNOTS ( ( 4, 4 ),
 ( 3, 3 ),
 ( 7.146054570217184225E-05, 0.0002313930902385299038 ),
 ( 0.000000000000000000, 1.000000000000000000 ),
 .UNSPECIFIED. ) 
 GEOMETRIC_REPRESENTATION_ITEM ( )  RATIONAL_B_SPLINE_SURFACE ( (
 ( 1.000000000000000000, 0.7071067811864972796, 1.000000000000000000),
 ( 1.000000000000000000, 0.6583912147046423469, 1.000000000000000000),
 ( 1.000000000000000000, 0.5850387677749523396, 1.000000000000000000),
 ( 1.000000000000000000, 0.5857791861290068125, 1.000000000000000000) ) ) 
 REPRESENTATION_ITEM ( '' )  SURFACE ( )  );
#5060 = CARTESIAN_POINT ( 'NONE',  ( 32.22975847903030910, 7.786540417375088730, -1.950000000000110756 ) ) ;
#5061 = DIRECTION ( 'NONE',  ( 0.000000000000000000, 0.000000000000000000, -1.000000000000000000 ) ) ;
#5062 = AXIS2_PLACEMENT_3D ( 'NONE', #29065, #2769, #24320 ) ;
#5063 = CARTESIAN_POINT ( 'NONE',  ( -59.42113335569190014, 3.317668011003051642, -1.077534877302829264 ) ) ;
#5064 = VECTOR ( 'NONE', #21462, 1000.000000000000000 ) ;
#5066 = VECTOR ( 'NONE', #712, 1000.000000000000000 ) ;
#5065 = CARTESIAN_POINT ( 'NONE',  ( -67.36397038208805554, -2.135367159695522155, -0.05319419038625883972 ) ) ;
#5068 = CARTESIAN_POINT ( 'NONE',  ( 50.38701762163459819, -1.088467210617550807, -3.899823238510139678 ) ) ;
#5067 = CYLINDRICAL_SURFACE ( 'NONE', #25621, 1.875000000000001776 ) ;
#5069 = ORIENTED_EDGE ( 'NONE', *, *, #8145, .F. ) ;
#5070 = B_SPLINE_CURVE_WITH_KNOTS ( 'NONE', 3,
 ( #5552, #8084, #10457, #5701, #5386, #27238, #22196, #15203, #24998, #2705, #7920, #480, #7617, #29443 ),
 .UNSPECIFIED., .F., .F.,
 ( 4, 2, 2, 2, 2, 2, 4 ),
 ( 0.000000000000000000, 2.506106230924540920E-05, 5.012212461849081840E-05, 0.0001002442492369731529, 0.0002004884984739371985, 0.0004009769969478685966, 0.0008019539938957305795 ),
 .UNSPECIFIED. ) ;
#5071 = PLANE ( 'NONE',  #5217 ) ;
#5072 = VERTEX_POINT ( 'NONE', #7999 ) ;
#5073 = CARTESIAN_POINT ( 'NONE',  ( 51.80000000000001137, 4.349412134559255350, -1.696806954411249402 ) ) ;
#5075 = CYLINDRICAL_SURFACE ( 'NONE', #11601, 1.000000000000000000 ) ;
#5074 = CARTESIAN_POINT ( 'NONE',  ( 15.44259799936805777, -2.880023619481785424, -4.335093843541868885 ) ) ;
#5076 = LINE ( 'NONE', #9685, #9520 ) ;
#5077 = ORIENTED_EDGE ( 'NONE', *, *, #2293, .F. ) ;
#5078 = ORIENTED_EDGE ( 'NONE', *, *, #16650, .F. ) ;
#5079 = DIRECTION ( 'NONE',  ( -7.401486830834377462E-15, 0.000000000000000000, -1.000000000000000000 ) ) ;
#5080 = EDGE_CURVE ( 'NONE', #6162, #7502, #5803, .T. ) ;
#5081 = VERTEX_POINT ( 'NONE', #10359 ) ;
#5082 = CARTESIAN_POINT ( 'NONE',  ( 58.75000000000002842, -1.039502773796971091, 1.800471618824829756 ) ) ;
#5083 = EDGE_CURVE ( 'NONE', #8829, #6950, #6154, .T. ) ;
#5084 = CARTESIAN_POINT ( 'NONE',  ( -54.86042740578361077, -0.7887156198831597465, 3.845940847736172952 ) ) ;
#5085 = VERTEX_POINT ( 'NONE', #22567 ) ;
#5086 = CARTESIAN_POINT ( 'NONE',  ( -36.22955757456080050, -5.027944117024021331, -1.353132643598599305 ) ) ;
#5087 = ORIENTED_EDGE ( 'NONE', *, *, #11156, .F. ) ;
#5088 = CARTESIAN_POINT ( 'NONE',  ( 58.65000000000003411, -1.253243060177393620, -1.394635017528123688 ) ) ;
#5089 = FILL_AREA_STYLE ('',( #19670 ) ) ;
#5090 = ORIENTED_EDGE ( 'NONE', *, *, #20294, .T. ) ;
#5091 = VECTOR ( 'NONE', #20263, 1000.000000000000114 ) ;
#5092 = EDGE_CURVE ( 'NONE', #21532, #11640, #5771, .T. ) ;
#5093 = CARTESIAN_POINT ( 'NONE',  ( -59.50952994616202574, 3.117691453623994580, -1.800000000000197664 ) ) ;
#5094 = CARTESIAN_POINT ( 'NONE',  ( 54.16568811108923143, 5.603438171869654205, -2.050000000000187672 ) ) ;
#5095 = DIRECTION ( 'NONE',  ( 8.860386339788722010E-15, -0.8459051693633015123, 0.5333333333333332149 ) ) ;
#5096 = CARTESIAN_POINT ( 'NONE',  ( -54.49983832461118283, -1.542920080254279958, 3.327619142904489014 ) ) ;
#5097 = DIRECTION ( 'NONE',  ( -2.614375865348241018E-16, 0.2008964009354147762, -0.9796124928211140670 ) ) ;
#5098 = DIRECTION ( 'NONE',  ( 1.000000000000000000, 1.047444401652940007E-14, 0.000000000000000000 ) ) ;
#5100 = CARTESIAN_POINT ( 'NONE',  ( -36.25997906085255096, -0.2181161761758297624, -5.200000001420975515 ) ) ;
#5099 = CARTESIAN_POINT ( 'NONE',  ( 58.50000000000001421, -0.8000000000000000444, 2.421260002560649660 ) ) ;
#5101 = DIRECTION ( 'NONE',  ( 0.000000000000000000, -0.9996898646859344595, -0.02490330187381124480 ) ) ;
#5102 = CARTESIAN_POINT ( 'NONE',  ( 50.25000000000000000, 1.960427193528456069, 0.3958853607757182314 ) ) ;
#5104 = DIRECTION ( 'NONE',  ( 0.9991330730923518866, 0.04161763361012259937, 0.001036738022138443578 ) ) ;
#5103 = CARTESIAN_POINT ( 'NONE',  ( 15.48609859788815690, 4.980680447166627722, -1.498595263773850661 ) ) ;
#5105 = ORIENTED_EDGE ( 'NONE', *, *, #5434, .T. ) ;
#5106 = CARTESIAN_POINT ( 'NONE',  ( 58.75000000000003553, -1.960427193528576639, 0.3958853607747486181 ) ) ;
#5107 = FACE_OUTER_BOUND ( 'NONE', #7591, .T. ) ;
#5108 = CIRCLE ( 'NONE', #12186, 1.260000000000000231 ) ;
#5110 = DIRECTION ( 'NONE',  ( -3.489354422748178188E-15, 1.218509414717996091E-16, -1.000000000000000000 ) ) ;
#5109 = CARTESIAN_POINT ( 'NONE',  ( 48.46185180831791683, -1.426738236278548566, 3.843750512866276559 ) ) ;
#5111 = CARTESIAN_POINT ( 'NONE',  ( 58.45000000000001705, -0.8000000000000000444, -1.778341924377873751 ) ) ;
#5112 = ORIENTED_EDGE ( 'NONE', *, *, #11080, .F. ) ;
#5113 = CARTESIAN_POINT ( 'NONE',  ( 61.25000000000003553, -0.9999999999993586242, 1.586072192556190252 ) ) ;
#5114 = ADVANCED_FACE ( 'NONE', ( #8297 ), #30559, .T. ) ;
#5115 = ORIENTED_EDGE ( 'NONE', *, *, #5759, .F. ) ;
#5116 = CARTESIAN_POINT ( 'NONE',  ( -59.37009172985672478, 3.234433134214944161, -1.048065980887175952 ) ) ;
#5117 = VERTEX_POINT ( 'NONE', #6395 ) ;
#5118 = ORIENTED_EDGE ( 'NONE', *, *, #26851, .T. ) ;
#5119 = CARTESIAN_POINT ( 'NONE',  ( -67.92156587216960872, -1.648633347906702129, -0.04106915093617326262 ) ) ;
#5120 = ORIENTED_EDGE ( 'NONE', *, *, #8315, .F. ) ;
#5121 = CARTESIAN_POINT ( 'NONE',  ( 52.06777441456687683, 4.366880381858252669, 1.445821729970449221 ) ) ;
#5122 = CARTESIAN_POINT ( 'NONE',  ( -55.38452994616205416, -3.117691453623976816, 1.799999999999791100 ) ) ;
#5123 = ORIENTED_EDGE ( 'NONE', *, *, #6295, .F. ) ;
#5124 = CARTESIAN_POINT ( 'NONE',  ( -56.31249999999998579, -1.962990915244736678, 3.399999999999788969 ) ) ;
#5125 = CARTESIAN_POINT ( 'NONE',  ( 33.47623932017462778, -4.018128179617534101, -3.618665901676658692 ) ) ;
#5126 = CARTESIAN_POINT ( 'NONE',  ( 30.98482657477578428, 7.184130536712136639, 2.050000000000149925 ) ) ;
#5127 = ORIENTED_EDGE ( 'NONE', *, *, #24333, .F. ) ;
#5128 = PRESENTATION_LAYER_ASSIGNMENT (  '', '', ( #1084 ) ) ;
#5129 = EDGE_CURVE ( 'NONE', #21850, #23309, #6556, .T. ) ;
#5130 = CARTESIAN_POINT ( 'NONE',  ( 51.45655683570189609, 0.9591657938401632055, -1.468576096419530463 ) ) ;
#5131 = FACE_OUTER_BOUND ( 'NONE', #8472, .T. ) ;
#5132 = DIRECTION ( 'NONE',  ( 1.000000000000000000, 1.047444401652940007E-14, 0.000000000000000000 ) ) ;
#5133 = CARTESIAN_POINT ( 'NONE',  ( 57.00555950015162665, -0.7236022373656367801, 2.438089627148707805 ) ) ;
#5135 = CARTESIAN_POINT ( 'NONE',  ( -44.49999999999999289, -1.400000000000007017, 3.959797974644484242 ) ) ;
#5134 = CARTESIAN_POINT ( 'NONE',  ( -36.56390771145571250, -3.345968172200375790, 4.250076229745575418 ) ) ;
#5136 = EDGE_CURVE ( 'NONE', #28516, #16439, #10691, .T. ) ;
#5137 = CARTESIAN_POINT ( 'NONE',  ( 51.11922224408084503, 0.9310536428531250852, 1.338077479438640971 ) ) ;
#5138 = CARTESIAN_POINT ( 'NONE',  ( 69.20000000000000284, -0.8558823529411765385, -2.268940368966790189 ) ) ;
#5139 = VECTOR ( 'NONE', #1153, 1000.000000000000000 ) ;
#5140 = CARTESIAN_POINT ( 'NONE',  ( 53.91678946233205494, 6.821600947619984368, 1.787725782035106459 ) ) ;
#5141 = ORIENTED_EDGE ( 'NONE', *, *, #24882, .F. ) ;
#5142 = B_SPLINE_CURVE_WITH_KNOTS ( 'NONE', 3,
 ( #26375, #6741, #14331, #16401 ),
 .UNSPECIFIED., .F., .F.,
 ( 4, 4 ),
 ( 0.000000000000000000, 2.862003379465107863E-05 ),
 .UNSPECIFIED. ) ;
#5143 = VERTEX_POINT ( 'NONE', #1782 ) ;
#5144 = CIRCLE ( 'NONE', #26374, 0.4576450603546982632 ) ;
#5145 = ADVANCED_FACE ( 'NONE', ( #6238 ), #30601, .T. ) ;
#5146 = ORIENTED_EDGE ( 'NONE', *, *, #28217, .F. ) ;
#5147 = FACE_OUTER_BOUND ( 'NONE', #19706, .T. ) ;
#5148 = CARTESIAN_POINT ( 'NONE',  ( -60.59585481156722864, -2.489203624310587504, 2.804704140674919355 ) ) ;
#5150 = CARTESIAN_POINT ( 'NONE',  ( -36.22909104983142470, 2.595074437874489437, 4.757608386864812466 ) ) ;
#5149 = CARTESIAN_POINT ( 'NONE',  ( 15.03925126672132784, 4.683225679163323996, 2.703237727951258051 ) ) ;
#5151 = ADVANCED_FACE ( 'NONE', ( #13511 ), #24007, .T. ) ;
#5152 = ORIENTED_EDGE ( 'NONE', *, *, #610, .T. ) ;
#5153 = CARTESIAN_POINT ( 'NONE',  ( -56.12486116251334778, -1.737685414808513018, 3.471684241605566879 ) ) ;
#5154 = VERTEX_POINT ( 'NONE', #8609 ) ;
#5155 = CARTESIAN_POINT ( 'NONE',  ( 21.97322666366011035, 8.076925076899403422, 1.949999999999922906 ) ) ;
#5156 = ORIENTED_EDGE ( 'NONE', *, *, #27593, .T. ) ;
#5157 = CARTESIAN_POINT ( 'NONE',  ( 33.40812713800432476, 8.122903761241905940, -1.949999999999987965 ) ) ;
#5158 = ORIENTED_EDGE ( 'NONE', *, *, #13644, .F. ) ;
#5159 = CARTESIAN_POINT ( 'NONE',  ( 50.93312545610842790, 0.6352506689595297518, -1.438808137080895611 ) ) ;
#5160 = DIRECTION ( 'NONE',  ( 1.000000000000000000, -1.219044193948983948E-29, 3.491481338843133355E-15 ) ) ;
#5161 = EDGE_CURVE ( 'NONE', #14419, #21148, #10855, .T. ) ;
#5162 = DIRECTION ( 'NONE',  ( 3.491481338843133750E-15, 0.000000000000000000, 1.000000000000000000 ) ) ;
#5164 = AXIS2_PLACEMENT_3D ( 'NONE', #11989, #2639, #19432 ) ;
#5163 = CARTESIAN_POINT ( 'NONE',  ( -55.14405989232412253, -2.944486372867076263, -1.700000000000206235 ) ) ;
#5165 = CARTESIAN_POINT ( 'NONE',  ( 51.68129744679067272, 4.333300462216210569, -2.050000000000496758 ) ) ;
#5166 = CARTESIAN_POINT ( 'NONE',  ( -58.81249999999996447, 3.400000000000008349, -1.915049148454697437E-13 ) ) ;
#5167 = CARTESIAN_POINT ( 'NONE',  ( 50.30000000000001847, 1.391941090707540685, -3.850000000000022293 ) ) ;
#5168 = EDGE_CURVE ( 'NONE', #26348, #1696, #3697, .T. ) ;
#5169 = FACE_OUTER_BOUND ( 'NONE', #23417, .T. ) ;
#5170 =( BOUNDED_SURFACE ( )  B_SPLINE_SURFACE ( 3, 2, ( 
 ( #27659, #27493, #15924 ),
 ( #13552, #18010, #17856 ),
 ( #27823, #1667, #25585 ),
 ( #30185, #23074, #5987 ),
 ( #23384, #1370, #23235 ),
 ( #1523, #11326, #20398 ) ),
 .UNSPECIFIED., .F., .F., .T. ) 
 B_SPLINE_SURFACE_WITH_KNOTS ( ( 4, 2, 4 ),
 ( 3, 3 ),
 ( 9.486769009248163798E-19, 0.0002090583013612445288, 0.0004181166027224881361 ),
 ( 0.000000000000000000, 1.000000000000000000 ),
 .UNSPECIFIED. ) 
 GEOMETRIC_REPRESENTATION_ITEM ( )  RATIONAL_B_SPLINE_SURFACE ( (
 ( 1.000000000000000000, 0.7071067811865492381, 1.000000000000000000),
 ( 1.000000000000000000, 0.7521684882082728674, 1.000000000000000000),
 ( 1.000000000000000000, 0.7851308282770136371, 1.000000000000000000),
 ( 1.000000000000000000, 0.8276934144745947686, 1.000000000000000000),
 ( 1.000000000000000000, 0.8364441017664203670, 1.000000000000000000),
 ( 1.000000000000000000, 0.8366600265340731202, 1.000000000000000000) ) ) 
 REPRESENTATION_ITEM ( '' )  SURFACE ( )  );
#5172 = ADVANCED_FACE ( 'NONE', ( #27925 ), #11140, .T. ) ;
#5171 = FACE_OUTER_BOUND ( 'NONE', #10876, .T. ) ;
#5173 = MANIFOLD_SOLID_BREP ( 'Stock-MAS-683-1', #14520 ) ;
#5174 = VECTOR ( 'NONE', #10057, 1000.000000000000000 ) ;
#5175 = ORIENTED_EDGE ( 'NONE', *, *, #18929, .F. ) ;
#5176 = CARTESIAN_POINT ( 'NONE',  ( 56.95000081403880188, -0.7675332364161941978, -2.484758330364432943 ) ) ;
#5177 = CARTESIAN_POINT ( 'NONE',  ( -35.85663232820601820, -2.199885893005943061, -4.939696249117692339 ) ) ;
#5178 = CARTESIAN_POINT ( 'NONE',  ( 53.91582462592150193, 6.672259099522118042, -0.8960560664367791528 ) ) ;
#5179 = VERTEX_POINT ( 'NONE', #13804 ) ;
#5180 = DIRECTION ( 'NONE',  ( 1.000000000000000000, 0.000000000000000000, -1.047444401652940007E-14 ) ) ;
#5181 = ORIENTED_EDGE ( 'NONE', *, *, #15824, .F. ) ;
#5182 = EDGE_CURVE ( 'NONE', #22859, #29340, #23489, .T. ) ;
#5183 = CARTESIAN_POINT ( 'NONE',  ( 48.30000000000003268, 0.7901969350670130510, 4.025772098418840983 ) ) ;
#5185 = DIRECTION ( 'NONE',  ( 1.000000000000000000, 0.000000000000000000, -0.000000000000000000 ) ) ;
#5184 = DIRECTION ( 'NONE',  ( 1.000000000000000000, 1.047444401652940007E-14, 0.000000000000000000 ) ) ;
#5186 = EDGE_CURVE ( 'NONE', #2667, #7825, #13973, .T. ) ;
#5187 = ORIENTED_EDGE ( 'NONE', *, *, #8547, .F. ) ;
#5188 = DIRECTION ( 'NONE',  ( 0.000000000000000000, 0.4531102586345838179, -0.8914544820236760536 ) ) ;
#5189 = DIRECTION ( 'NONE',  ( -1.000000000000000000, -1.293068473084537258E-16, -0.000000000000000000 ) ) ;
#5191 = CARTESIAN_POINT ( 'NONE',  ( -59.69999999999997442, 2.444843547360534775, -1.238538609462265905 ) ) ;
#5190 = CARTESIAN_POINT ( 'NONE',  ( -67.99999999999995737, -3.266925685480207642E-16, 2.202315069465528948E-15 ) ) ;
#5192 = CARTESIAN_POINT ( 'NONE',  ( 52.06628335902946247, -0.5434431642975682264, -1.794517909405659806 ) ) ;
#5193 = CARTESIAN_POINT ( 'NONE',  ( -59.68749999999997158, 3.238593381231845036, 2.874284765127022023 ) ) ;
#5194 = CARTESIAN_POINT ( 'NONE',  ( 36.50000000000002132, -0.8000000000000000444, 1.778341924377873751 ) ) ;
#5195 = DIRECTION ( 'NONE',  ( 0.7071067811865435759, 0.7068874824028903436, 0.01760929362890753525 ) ) ;
#5196 = CARTESIAN_POINT ( 'NONE',  ( 34.56269065792917417, 8.313757757582560970, 2.049999999999879474 ) ) ;
#5197 = CARTESIAN_POINT ( 'NONE',  ( -54.49999999999997158, -0.9764555328423589753, -3.345672051885957732 ) ) ;
#5198 = CARTESIAN_POINT ( 'NONE',  ( 52.20711756518984714, -0.7499999999994533262, -1.996089927833914146 ) ) ;
#5200 = CARTESIAN_POINT ( 'NONE',  ( 48.50000000000002132, 1.391941090707534023, 3.850000000000022737 ) ) ;
#5199 = CIRCLE ( 'NONE', #3681, 0.1500000000000001887 ) ;
#5201 = ORIENTED_EDGE ( 'NONE', *, *, #1082, .F. ) ;
#5202 = B_SPLINE_CURVE_WITH_KNOTS ( 'NONE', 3,
 ( #23616, #28197, #11402, #9036, #1913, #11575, #21404, #31032, #12197, #16952, #5068, #19650, #7738, #24070 ),
 .UNSPECIFIED., .F., .F.,
 ( 4, 2, 2, 2, 2, 2, 4 ),
 ( 0.000000000000000000, 2.506106230924558877E-05, 5.012212461849117754E-05, 0.0001002442492369727192, 0.0002004884984739364396, 0.0004009769969478670787, 0.0008019539938957288448 ),
 .UNSPECIFIED. ) ;
#5203 = CARTESIAN_POINT ( 'NONE',  ( 51.76665129121498410, 4.175715153428418702, 1.929612129901060902 ) ) ;
#5204 = FACE_OUTER_BOUND ( 'NONE', #27411, .T. ) ;
#5205 = EDGE_CURVE ( 'NONE', #25278, #10205, #22491, .T. ) ;
#5206 = EDGE_CURVE ( 'NONE', #9375, #20708, #13336, .T. ) ;
#5207 = FACE_OUTER_BOUND ( 'NONE', #11250, .T. ) ;
#5209 = EDGE_CURVE ( 'NONE', #2740, #27829, #2608, .T. ) ;
#5208 = FACE_OUTER_BOUND ( 'NONE', #18727, .T. ) ;
#5210 = CARTESIAN_POINT ( 'NONE',  ( -60.54800159808252147, 1.949167012834402697E-15, 6.802637593289325421E-16 ) ) ;
#5212 = FACE_OUTER_BOUND ( 'NONE', #19208, .T. ) ;
#5211 = CARTESIAN_POINT ( 'NONE',  ( 58.75000006180458456, 0.5511536957114213653, 1.849318015439010532 ) ) ;
#5213 = ORIENTED_EDGE ( 'NONE', *, *, #771, .F. ) ;
#5214 = CARTESIAN_POINT ( 'NONE',  ( 58.65266784251144827, -1.827264058874260133, 0.4207260278637539597 ) ) ;
#5215 = ORIENTED_EDGE ( 'NONE', *, *, #2584, .T. ) ;
#5216 = DIRECTION ( 'NONE',  ( -1.000000000000000000, 0.000000000000000000, 0.000000000000000000 ) ) ;
#5217 = AXIS2_PLACEMENT_3D ( 'NONE', #22019, #19652, #23776 ) ;
#5219 = DIRECTION ( 'NONE',  ( -2.167639087557276846E-15, 0.2069455031824688485, -0.9783524716136586807 ) ) ;
#5218 = CARTESIAN_POINT ( 'NONE',  ( 69.20000000000004547, 0.7500000000000000000, 1.988246715072631732 ) ) ;
#5220 = FACE_OUTER_BOUND ( 'NONE', #30306, .T. ) ;
#5221 = AXIS2_PLACEMENT_3D ( 'NONE', #13155, #8254, #1273 ) ;
#5222 = ORIENTED_EDGE ( 'NONE', *, *, #29707, .F. ) ;
#5223 = ORIENTED_EDGE ( 'NONE', *, *, #20813, .F. ) ;
#5224 = FACE_OUTER_BOUND ( 'NONE', #25462, .T. ) ;
#5225 = DIRECTION ( 'NONE',  ( 1.093889549751081128E-14, -0.9507508458637282667, -0.3099561728525587756 ) ) ;
#5226 = ORIENTED_EDGE ( 'NONE', *, *, #18865, .F. ) ;
#5227 = CARTESIAN_POINT ( 'NONE',  ( 51.77696287275522735, -4.162962223351915902, 1.036150832289953971 ) ) ;
#5228 = CARTESIAN_POINT ( 'NONE',  ( -55.23542740578361077, 0.7887156198831668519, -3.845940847736174728 ) ) ;
#5229 = CARTESIAN_POINT ( 'NONE',  ( -36.11122220296834229, -5.068511731019583522, -1.228278365481880297 ) ) ;
#5230 = VERTEX_POINT ( 'NONE', #2853 ) ;
#5231 = CARTESIAN_POINT ( 'NONE',  ( 0.000000000000000000, 0.000000000000000000, 0.000000000000000000 ) ) ;
#5232 = CARTESIAN_POINT ( 'NONE',  ( -59.29999999999999716, -3.501719128350677224, -1.006773934787358771 ) ) ;
#5233 = VERTEX_POINT ( 'NONE', #7038 ) ;
#5234 = CARTESIAN_POINT ( 'NONE',  ( -59.63452994616203284, 2.093608279459373297E-14, -3.600000000000211475 ) ) ;
#5235 = CARTESIAN_POINT ( 'NONE',  ( 51.80000000000001137, 8.701414213562481237, -2.050000000000180123 ) ) ;
#5236 = CARTESIAN_POINT ( 'NONE',  ( 48.30000000000002558, -0.6462379109120511833, -4.048750000000022276 ) ) ;
#5237 = VECTOR ( 'NONE', #12127, 1000.000000000000000 ) ;
#5238 = DIRECTION ( 'NONE',  ( 1.000000000000000000, -0.000000000000000000, -0.000000000000000000 ) ) ;
#5239 = CIRCLE ( 'NONE', #8209, 1.487500000000000933 ) ;
#5240 = CARTESIAN_POINT ( 'NONE',  ( 50.80000000000002558, -4.031600731908413948, 1.173113608511496375 ) ) ;
#5241 = EDGE_CURVE ( 'NONE', #133, #9283, #5022, .T. ) ;
#5242 = CARTESIAN_POINT ( 'NONE',  ( -58.58155989232410832, 3.400000000000007905, -1.908076882137507950E-13 ) ) ;
#5245 = ADVANCED_FACE ( 'NONE', ( #23821 ), #28728, .F. ) ;
#5244 = CARTESIAN_POINT ( 'NONE',  ( -36.11692583559979397, -1.123735554575807427, -5.289358692618237434 ) ) ;
#5243 = DIRECTION ( 'NONE',  ( 0.000000000000000000, -0.9333474217026306308, 0.3589743589743588648 ) ) ;
#5246 = DIRECTION ( 'NONE',  ( 0.000000000000000000, 0.000000000000000000, 1.000000000000000000 ) ) ;
#5248 = DIRECTION ( 'NONE',  ( 0.000000000000000000, 0.000000000000000000, 1.000000000000000000 ) ) ;
#5247 = DIRECTION ( 'NONE',  ( 0.000000000000000000, 0.000000000000000000, 1.000000000000000000 ) ) ;
#5249 = ORIENTED_EDGE ( 'NONE', *, *, #10781, .F. ) ;
#5250 = DIRECTION ( 'NONE',  ( 2.581436205204234499E-16, -0.9796124928211140670, -0.2008964009354146651 ) ) ;
#5251 = CARTESIAN_POINT ( 'NONE',  ( -36.52679053911622731, -4.797009389500161092, -2.498041539401842925 ) ) ;
#5253 = DIRECTION ( 'NONE',  ( 1.520093157366863885E-16, -0.5877852522924685852, -0.8090169943749507819 ) ) ;
#5252 = CARTESIAN_POINT ( 'NONE',  ( 15.74652664997094931, 3.008101665203244846, -4.495550615867462518 ) ) ;
#5254 = DIRECTION ( 'NONE',  ( 0.8023336663629093701, 0.5470456816110859100, -0.2387503090077881251 ) ) ;
#5255 = ORIENTED_EDGE ( 'NONE', *, *, #9238, .T. ) ;
#5256 = CARTESIAN_POINT ( 'NONE',  ( 68.94999999999998863, 4.837354856632045057E-16, -3.950000000000722711 ) ) ;
#5257 = EDGE_CURVE ( 'NONE', #25072, #30388, #20223, .T. ) ;
#5258 = VERTEX_POINT ( 'NONE', #22339 ) ;
#5259 = CIRCLE ( 'NONE', #22970, 0.1000000000000000611 ) ;
#5260 = CARTESIAN_POINT ( 'NONE',  ( 51.31572262954149011, 1.002608958138273554, -1.395204572094392637 ) ) ;
#5261 = ORIENTED_EDGE ( 'NONE', *, *, #9015, .T. ) ;
#5262 = ORIENTED_EDGE ( 'NONE', *, *, #14118, .T. ) ;
#5263 = CARTESIAN_POINT ( 'NONE',  ( 58.65000000000002700, -0.5539202450379242526, -1.791540873397694966 ) ) ;
#5264 = B_SPLINE_CURVE_WITH_KNOTS ( 'NONE', 3,
 ( #26635, #1765, #9069, #18743, #6689, #28535 ),
 .UNSPECIFIED., .F., .F.,
 ( 4, 2, 4 ),
 ( 0.000000000000000000, 0.0003982002662752217367, 0.0007964005325504434733 ),
 .UNSPECIFIED. ) ;
#5265 = ORIENTED_EDGE ( 'NONE', *, *, #5279, .F. ) ;
#5266 = DIRECTION ( 'NONE',  ( 0.000000000000000000, 1.000000000000000000, 0.000000000000000000 ) ) ;
#5267 = CARTESIAN_POINT ( 'NONE',  ( -55.14405989232412253, -2.944486372867076263, -1.700000000000206235 ) ) ;
#5268 = ORIENTED_EDGE ( 'NONE', *, *, #3523, .T. ) ;
#5269 = CIRCLE ( 'NONE', #11856, 0.4576450603546999840 ) ;
#5270 = FACE_OUTER_BOUND ( 'NONE', #10710, .T. ) ;
#5271 = AXIS2_PLACEMENT_3D ( 'NONE', #7854, #15146, #20076 ) ;
#5272 = CARTESIAN_POINT ( 'NONE',  ( 25.99900894223004855, 5.212247165294382256, 1.949999999999974198 ) ) ;
#5273 = VERTEX_POINT ( 'NONE', #29300 ) ;
#5274 = LINE ( 'NONE', #17643, #21361 ) ;
#5275 = DIRECTION ( 'NONE',  ( 0.000000000000000000, 0.000000000000000000, -1.000000000000000000 ) ) ;
#5276 = CARTESIAN_POINT ( 'NONE',  ( 58.75000000000002842, -1.077297519403688009, -1.655311165516759608 ) ) ;
#5277 = DIRECTION ( 'NONE',  ( 1.000000000000000000, 0.000000000000000000, 0.000000000000000000 ) ) ;
#5278 = CARTESIAN_POINT ( 'NONE',  ( 57.00500393873097238, 0.7225500701544015358, 2.438740121660158078 ) ) ;
#5279 = EDGE_CURVE ( 'NONE', #3014, #14583, #29798, .T. ) ;
#5281 = DIRECTION ( 'NONE',  ( 0.000000000000000000, 0.000000000000000000, 1.000000000000000000 ) ) ;
#5280 = CARTESIAN_POINT ( 'NONE',  ( -35.85663232820592583, -3.426725943139568020, 3.937891353488737423 ) ) ;
#5282 = AXIS2_PLACEMENT_3D ( 'NONE', #11513, #11330, #23388 ) ;
#5283 = CARTESIAN_POINT ( 'NONE',  ( 51.80000000000001847, -3.726179070414207928, 1.100000000000000533 ) ) ;
#5284 = CARTESIAN_POINT ( 'NONE',  ( 53.87827693845219557, 5.944250707180090743, 1.708828125785182728 ) ) ;
#5285 = AXIS2_PLACEMENT_3D ( 'NONE', #20934, #6355, #18564 ) ;
#5286 = ORIENTED_EDGE ( 'NONE', *, *, #22542, .F. ) ;
#5287 = ORIENTED_EDGE ( 'NONE', *, *, #11983, .T. ) ;
#5288 = ADVANCED_FACE ( 'NONE', ( #26914 ), #627, .T. ) ;
#5289 = ORIENTED_EDGE ( 'NONE', *, *, #29184, .T. ) ;
#5290 = CARTESIAN_POINT ( 'NONE',  ( -59.15580762875987375, 2.348892103289441202, 1.260680929859216537 ) ) ;
#5291 = CARTESIAN_POINT ( 'NONE',  ( -59.42292740578359656, 1.073804522883521351, 3.225979517392337126 ) ) ;
#5293 = DIRECTION ( 'NONE',  ( 0.000000000000000000, 0.000000000000000000, 1.000000000000000000 ) ) ;
#5292 = CARTESIAN_POINT ( 'NONE',  ( 60.75000000000003553, -0.9999999999993638422, -1.996089927833914146 ) ) ;
#5294 = EDGE_LOOP ( 'NONE', ( #8058, #30938, #15112, #14632, #18512 ) ) ;
#5295 = ORIENTED_EDGE ( 'NONE', *, *, #14044, .T. ) ;
#5296 = AXIS2_PLACEMENT_3D ( 'NONE', #7134, #158, #14713 ) ;
#5297 = CARTESIAN_POINT ( 'NONE',  ( 53.90826135247864670, 6.078611590743634885, -1.730551853729838774 ) ) ;
#5298 = ORIENTED_EDGE ( 'NONE', *, *, #3819, .T. ) ;
#5299 = DIRECTION ( 'NONE',  ( -1.000000000000000000, -3.054025858079668409E-16, 2.042474015755241579E-16 ) ) ;
#5300 = ORIENTED_EDGE ( 'NONE', *, *, #2711, .T. ) ;
#5301 = CARTESIAN_POINT ( 'NONE',  ( 29.19109589769589164, 6.114704649263054570, -2.050000000000100631 ) ) ;
#5302 = AXIS2_PLACEMENT_3D ( 'NONE', #21387, #23752, #19001 ) ;
#5303 = CARTESIAN_POINT ( 'NONE',  ( -57.39405989232411542, -2.944486372867072710, -1.700000000000220446 ) ) ;
#5304 = CARTESIAN_POINT ( 'NONE',  ( -59.29999999999997584, 2.330309927981285032E-15, 4.253626757584724400E-16 ) ) ;
#5305 = CARTESIAN_POINT ( 'NONE',  ( 15.29954477411456892, -4.683225668089734839, -2.703237747135711189 ) ) ;
#5306 = CIRCLE ( 'NONE', #8845, 0.2999999999999999334 ) ;
#5307 = CARTESIAN_POINT ( 'NONE',  ( -60.25952994616203284, 3.117691453623994580, -1.800000000000200329 ) ) ;
#5308 = CARTESIAN_POINT ( 'NONE',  ( 51.97945110550969616, 4.337541896208930048, -1.549654688285467596 ) ) ;
#5309 = ADVANCED_FACE ( 'NONE', ( #22030 ), #2475, .T. ) ;
#5310 = DIRECTION ( 'NONE',  ( 0.000000000000000000, 0.000000000000000000, 1.000000000000000000 ) ) ;
#5311 = FACE_OUTER_BOUND ( 'NONE', #23467, .T. ) ;
#5312 = EDGE_CURVE ( 'NONE', #1336, #2824, #993, .T. ) ;
#5313 = CIRCLE ( 'NONE', #21536, 0.05000000000000002359 ) ;
#5314 = CARTESIAN_POINT ( 'NONE',  ( -59.19126343180466421, -2.406052454186071277, 1.245092465133171844 ) ) ;
#5315 = CIRCLE ( 'NONE', #20520, 4.800000000000000711 ) ;
#5316 = CARTESIAN_POINT ( 'NONE',  ( 51.34893360928146677, -1.002183861492330630, 1.396106892655424980 ) ) ;
#5317 = VERTEX_POINT ( 'NONE', #27233 ) ;
#5318 = CARTESIAN_POINT ( 'NONE',  ( -59.29999999999998295, 2.406774162954685714, 2.810364340920085358 ) ) ;
#5319 = CARTESIAN_POINT ( 'NONE',  ( 61.09423418604154676, -0.6373668173473425735, 1.895722432253304168 ) ) ;
#5320 = CARTESIAN_POINT ( 'NONE',  ( 54.24287105605030490, 6.361183780992974768, 2.049999999999811529 ) ) ;
#5321 = TOROIDAL_SURFACE ( 'NONE', #9391, 1.875000000000000222, 0.2500000000000000000 ) ;
#5322 = EDGE_LOOP ( 'NONE', ( #5823, #17092 ) ) ;
#5323 = EDGE_CURVE ( 'NONE', #9517, #9001, #15042, .T. ) ;
#5324 = CARTESIAN_POINT ( 'NONE',  ( 58.64999999999992752, -1.877732920580853948, 0.6121634413819996290 ) ) ;
#5325 = ORIENTED_EDGE ( 'NONE', *, *, #27536, .T. ) ;
#5326 = AXIS2_PLACEMENT_3D ( 'NONE', #28085, #6565, #13097 ) ;
#5327 = CARTESIAN_POINT ( 'NONE',  ( 15.94709373951305054, 0.6031025731807972967, -5.374022845360688194 ) ) ;
#5328 = CARTESIAN_POINT ( 'NONE',  ( -35.85663232820601820, -5.377732432866662471, 0.5657657256215425923 ) ) ;
#5330 = CARTESIAN_POINT ( 'NONE',  ( -61.34138888940498902, -2.634947490092511835, -0.5919143299442317652 ) ) ;
#5329 = CARTESIAN_POINT ( 'NONE',  ( 51.52519442949588324, -4.265347051556910962, 1.724604836179060019 ) ) ;
#5331 = ORIENTED_EDGE ( 'NONE', *, *, #22449, .F. ) ;
#5332 = CARTESIAN_POINT ( 'NONE',  ( -57.83155989232412253, 3.400000000000007905, -1.837192174579415376E-13 ) ) ;
#5333 = DIRECTION ( 'NONE',  ( 3.304235192336781034E-15, 0.000000000000000000, 1.000000000000000000 ) ) ;
#5334 = ORIENTED_EDGE ( 'NONE', *, *, #27663, .T. ) ;
#5336 = CARTESIAN_POINT ( 'NONE',  ( -59.69142724121850563, 2.412383461849218591, -1.233589124872089826 ) ) ;
#5335 = CARTESIAN_POINT ( 'NONE',  ( -58.17306624327022746, -3.399999999999988365, -0.9110272542660463602 ) ) ;
#5337 = ORIENTED_EDGE ( 'NONE', *, *, #3505, .T. ) ;
#5338 = CARTESIAN_POINT ( 'NONE',  ( -58.93749999999996447, 3.238593381231845036, 2.874284765127021579 ) ) ;
#5339 = CARTESIAN_POINT ( 'NONE',  ( 57.05000000000001847, -0.7794871794871796045, 1.732743413496389939 ) ) ;
#5340 = EDGE_CURVE ( 'NONE', #7978, #6201, #24701, .T. ) ;
#5341 = AXIS2_PLACEMENT_3D ( 'NONE', #303, #24376, #7139 ) ;
#5342 = CARTESIAN_POINT ( 'NONE',  ( -55.40400635094609072, 1.737685414808522788, -3.471684241605564658 ) ) ;
#5343 = TOROIDAL_SURFACE ( 'NONE', #6368, 4.275000000000000355, 0.1000000000000000056 ) ;
#5344 = CARTESIAN_POINT ( 'NONE',  ( -54.49999999999996447, -3.201122295486859226, -1.751003668462366880 ) ) ;
#5345 = CARTESIAN_POINT ( 'NONE',  ( -59.69999999999997442, 0.8751759519302413359, -3.334367871151324714 ) ) ;
#5346 = DIRECTION ( 'NONE',  ( -2.614375865348241018E-16, 0.2008964009354147762, -0.9796124928211140670 ) ) ;
#5347 = DIRECTION ( 'NONE',  ( 0.000000000000000000, -0.2008964009354148039, 0.9796124928211139560 ) ) ;
#5348 = CIRCLE ( 'NONE', #13423, 1.679509022399086948 ) ;
#5349 = ORIENTED_EDGE ( 'NONE', *, *, #16851, .T. ) ;
#5350 = CIRCLE ( 'NONE', #15460, 0.2500000000000000000 ) ;
#5351 = CIRCLE ( 'NONE', #6965, 0.5000000000000013323 ) ;
#5352 = ADVANCED_FACE ( 'NONE', ( #9250 ), #13886, .F. ) ;
#5353 =( BOUNDED_CURVE ( )  B_SPLINE_CURVE ( 3, ( #23769, #8699, #28502, #16467 ),
 .UNSPECIFIED., .F., .T. ) 
 B_SPLINE_CURVE_WITH_KNOTS ( ( 4, 4 ),
 ( 1.982313172862383732, 2.241731514487931065 ),
 .UNSPECIFIED. ) 
 CURVE ( )  GEOMETRIC_REPRESENTATION_ITEM ( )  RATIONAL_B_SPLINE_CURVE ( ( 1.000000000000000000, 0.9943997021150919879, 0.9943997021150919879, 1.000000000000000000 ) ) 
 REPRESENTATION_ITEM ( '' )  );
#5354 = TOROIDAL_SURFACE ( 'NONE', #14444, 4.050000000000000711, 0.05000000000000000278 ) ;
#5355 = CARTESIAN_POINT ( 'NONE',  ( 15.66436536804550883, 2.847679722116457146, 4.601476325142709101 ) ) ;
#5356 = EDGE_CURVE ( 'NONE', #16069, #17883, #25759, .T. ) ;
#5357 = ADVANCED_FACE ( 'NONE', ( #6027, #30061 ), #1246, .F. ) ;
#5358 = B_SPLINE_CURVE_WITH_KNOTS ( 'NONE', 3,
 ( #2050, #23759, #16457, #11714, #9021, #18851, #18692, #11229, #9188, #16150, #4427, #16788, #21392, #7128, #28494, #25801, #9340, #30534, #21239 ),
 .UNSPECIFIED., .F., .F.,
 ( 4, 3, 3, 3, 3, 3, 4 ),
 ( 0.000000000000000000, 1.462084321540209121E-05, 2.917085440492037316E-05, 4.467649728434973632E-05, 6.285390091960512901E-05, 8.531547445983615763E-05, 8.677858956768834506E-05 ),
 .UNSPECIFIED. ) ;
#5359 = CARTESIAN_POINT ( 'NONE',  ( 58.65000000000003411, -1.320082690053553387, -1.469015551796290397 ) ) ;
#5360 = AXIS2_PLACEMENT_3D ( 'NONE', #28470, #3763, #6772 ) ;
#5361 = DIRECTION ( 'NONE',  ( 1.000000000000000000, 1.047444401652940007E-14, 0.000000000000000000 ) ) ;
#5362 = CIRCLE ( 'NONE', #24578, 0.05000000000000012768 ) ;
#5363 = CARTESIAN_POINT ( 'NONE',  ( -59.39369649845482257, 3.270110022916793646, 1.536003293967694860 ) ) ;
#5364 = CARTESIAN_POINT ( 'NONE',  ( -56.56249999999997158, -0.7533615035078050637, 3.673546848079176197 ) ) ;
#5366 = CARTESIAN_POINT ( 'NONE',  ( 29.45665666413592376, 6.177494273110388789, 1.424999999999897904 ) ) ;
#5365 = FACE_OUTER_BOUND ( 'NONE', #24098, .T. ) ;
#5367 = ORIENTED_EDGE ( 'NONE', *, *, #30465, .F. ) ;
#5368 = DIRECTION ( 'NONE',  ( -1.047444401652940007E-14, 0.000000000000000000, -1.000000000000000000 ) ) ;
#5369 = AXIS2_PLACEMENT_3D ( 'NONE', #5614, #15263, #24910 ) ;
#5370 = ORIENTED_EDGE ( 'NONE', *, *, #8979, .T. ) ;
#5371 = UNCERTAINTY_MEASURE_WITH_UNIT (LENGTH_MEASURE( 1.000000000000000082E-05 ), #4761, 'distance_accuracy_value', 'NONE');
#5372 = CARTESIAN_POINT ( 'NONE',  ( -54.44999999999997442, 0.000000000000000000, 0.000000000000000000 ) ) ;
#5374 = FACE_OUTER_BOUND ( 'NONE', #22304, .T. ) ;
#5373 = CARTESIAN_POINT ( 'NONE',  ( 15.61552784268254079, -3.561547362098998359, -4.076645242318565288 ) ) ;
#5375 = DIRECTION ( 'NONE',  ( 0.000000000000000000, 0.000000000000000000, 1.000000000000000000 ) ) ;
#5376 = AXIS2_PLACEMENT_3D ( 'NONE', #13041, #14937, #22723 ) ;
#5377 = ORIENTED_EDGE ( 'NONE', *, *, #15516, .T. ) ;
#5378 = ORIENTED_EDGE ( 'NONE', *, *, #1864, .F. ) ;
#5379 = CARTESIAN_POINT ( 'NONE',  ( -59.27703510351125260, 3.069728509726986854, 1.483074255709971867 ) ) ;
#5380 = AXIS2_PLACEMENT_3D ( 'NONE', #27947, #23054, #8773 ) ;
#5381 = AXIS2_PLACEMENT_3D ( 'NONE', #12530, #352, #26937 ) ;
#5382 = CARTESIAN_POINT ( 'NONE',  ( 34.50000000000001421, 0.000000000000000000, 0.000000000000000000 ) ) ;
#5383 = EDGE_LOOP ( 'NONE', ( #25715, #24167, #6740, #26466 ) ) ;
#5384 = AXIS2_PLACEMENT_3D ( 'NONE', #26806, #26948, #17622 ) ;
#5385 = DIRECTION ( 'NONE',  ( 1.168655815394902336E-14, 5.329070518200751394E-15, 1.000000000000000000 ) ) ;
#5386 = CARTESIAN_POINT ( 'NONE',  ( 50.33046473658143327, 1.366509374015061784, 3.854674997130605352 ) ) ;
#5387 = ADVANCED_FACE ( 'NONE', ( #27704, #27860 ), #13268, .F. ) ;
#5388 = CARTESIAN_POINT ( 'NONE',  ( -36.38012252111052902, -5.369990034204360718, -0.6654225812206043811 ) ) ;
#5389 = EDGE_LOOP ( 'NONE', ( #9825, #30740, #7516, #9625, #22269 ) ) ;
#5390 = DIRECTION ( 'NONE',  ( 1.000000000000000000, 0.000000000000000000, 0.000000000000000000 ) ) ;
#5391 = CARTESIAN_POINT ( 'NONE',  ( 58.75000000000003553, -1.320165430233233295, -1.457266603153496876 ) ) ;
#5392 = SURFACE_STYLE_FILL_AREA ( #2408 ) ;
#5393 = EDGE_CURVE ( 'NONE', #28012, #6477, #3634, .T. ) ;
#5394 = CIRCLE ( 'NONE', #24631, 0.05000000000000012768 ) ;
#5395 = AXIS2_PLACEMENT_3D ( 'NONE', #14719, #19794, #17404 ) ;
#5396 = ORIENTED_EDGE ( 'NONE', *, *, #23794, .T. ) ;
#5397 = AXIS2_PLACEMENT_3D ( 'NONE', #6996, #4915, #17124 ) ;
#5398 = CARTESIAN_POINT ( 'NONE',  ( -57.13452994616205416, 3.117691453623979481, 1.799999999999809086 ) ) ;
#5399 = CIRCLE ( 'NONE', #4902, 2.649999999999999911 ) ;
#5400 = CARTESIAN_POINT ( 'NONE',  ( 50.50000000000002842, 0.7900853852131533017, 4.025789903357282817 ) ) ;
#5401 = DIRECTION ( 'NONE',  ( -1.000000000000000000, 1.219044193948983948E-29, -3.491481338843133355E-15 ) ) ;
#5402 = CARTESIAN_POINT ( 'NONE',  ( -54.48833221701376317, -1.517896399908648553, 3.311598511234999265 ) ) ;
#5403 = AXIS2_PLACEMENT_3D ( 'NONE', #10479, #22214, #3185 ) ;
#5404 = CARTESIAN_POINT ( 'NONE',  ( 51.80000000000001137, -4.131056160354152240, -1.100000000000000533 ) ) ;
#5405 = AXIS2_PLACEMENT_3D ( 'NONE', #6731, #20535, #30168 ) ;
#5406 = DIRECTION ( 'NONE',  ( 1.000000000000000000, -1.219044193948983948E-29, 3.491481338843133355E-15 ) ) ;
#5407 = AXIS2_PLACEMENT_3D ( 'NONE', #8283, #22551, #12867 ) ;
#5409 = CARTESIAN_POINT ( 'NONE',  ( -36.42771574642738841, -0.4841707035675313908, -5.391286593723126686 ) ) ;
#5408 = CARTESIAN_POINT ( 'NONE',  ( 51.14630318392407560, -0.9364487020629673752, -1.503522130792586564 ) ) ;
#5410 = TOROIDAL_SURFACE ( 'NONE', #16548, 2.100674278852607824, 0.05000000000000000278 ) ;
#5411 = DIRECTION ( 'NONE',  ( 1.047444401652940007E-14, 0.000000000000000000, 1.000000000000000000 ) ) ;
#5412 = CARTESIAN_POINT ( 'NONE',  ( 48.45334018241208440, 1.329038565861465848, -3.861394075523872260 ) ) ;
#5414 = CARTESIAN_POINT ( 'NONE',  ( -62.09999999999997300, -2.652521544886486726, -0.2850577375623332688 ) ) ;
#5413 = CARTESIAN_POINT ( 'NONE',  ( 16.10705563471229596, 5.094475812726745545, -1.819860688632924939 ) ) ;
#5415 = ORIENTED_EDGE ( 'NONE', *, *, #27375, .T. ) ;
#5416 = DIRECTION ( 'NONE',  ( -1.000000000000000000, 0.000000000000000000, 1.047444401652940007E-14 ) ) ;
#5417 = CARTESIAN_POINT ( 'NONE',  ( -36.40793637698146057, -4.755763096844269455, -2.574151833883825624 ) ) ;
#5418 = AXIS2_PLACEMENT_3D ( 'NONE', #11222, #15681, #20896 ) ;
#5420 = CARTESIAN_POINT ( 'NONE',  ( 52.05786831706192430, 3.857808750919801355, 1.390516658560897234 ) ) ;
#5419 = CARTESIAN_POINT ( 'NONE',  ( 15.56401610563845139, 2.291889356119606536, -4.901871067649723024 ) ) ;
#5421 = CARTESIAN_POINT ( 'NONE',  ( 47.12301153005437016, -4.134673935618278229, 2.019140663349721976 ) ) ;
#5422 = VERTEX_POINT ( 'NONE', #22662 ) ;
#5423 = CARTESIAN_POINT ( 'NONE',  ( 60.88479802533564111, -0.4999999999993592348, 1.718465885608769117 ) ) ;
#5424 = CARTESIAN_POINT ( 'NONE',  ( 51.86913982414762359, 0.07429701114036996179, -4.369569592321115081 ) ) ;
#5425 = CIRCLE ( 'NONE', #23133, 0.4576450603546982632 ) ;
#5426 = CIRCLE ( 'NONE', #17571, 4.600000000000036948 ) ;
#5427 = VERTEX_POINT ( 'NONE', #10609 ) ;
#5428 = CARTESIAN_POINT ( 'NONE',  ( 15.32766723174653833, -5.374753047227047276, 0.5963205376973673699 ) ) ;
#5429 = VERTEX_POINT ( 'NONE', #15967 ) ;
#5430 = ORIENTED_EDGE ( 'NONE', *, *, #10947, .F. ) ;
#5431 = EDGE_CURVE ( 'NONE', #30058, #5273, #5528, .T. ) ;
#5432 = CARTESIAN_POINT ( 'NONE',  ( 15.41586008885036563, 5.027926281937914688, 1.353187539902049430 ) ) ;
#5433 = ORIENTED_EDGE ( 'NONE', *, *, #17085, .F. ) ;
#5434 = EDGE_CURVE ( 'NONE', #24812, #9170, #24254, .T. ) ;
#5435 = CARTESIAN_POINT ( 'NONE',  ( 30.91033855991008039, 7.142409676556906284, 1.949999999999890710 ) ) ;
#5436 = AXIS2_PLACEMENT_3D ( 'NONE', #29883, #15788, #29727 ) ;
#5437 = CARTESIAN_POINT ( 'NONE',  ( -60.82202994616204705, 2.078460969082646770, 3.599999999999791367 ) ) ;
#5438 = ORIENTED_EDGE ( 'NONE', *, *, #18029, .F. ) ;
#5439 = DIRECTION ( 'NONE',  ( -9.754918421198724481E-16, -0.9601771338024399638, -0.2793919678926571892 ) ) ;
#5440 = CIRCLE ( 'NONE', #378, 4.600000000000000533 ) ;
#5441 = EDGE_CURVE ( 'NONE', #18442, #24092, #12117, .T. ) ;
#5442 = VECTOR ( 'NONE', #1305, 1000.000000000000000 ) ;
#5443 = EDGE_LOOP ( 'NONE', ( #6142, #21561, #27785, #16734 ) ) ;
#5444 = DIRECTION ( 'NONE',  ( 1.000000000000000000, -0.000000000000000000, -1.047444401652940007E-14 ) ) ;
#5445 = CARTESIAN_POINT ( 'NONE',  ( 25.68808851946594984, 5.234409800456067963, 2.049999999999911005 ) ) ;
#5446 = ORIENTED_EDGE ( 'NONE', *, *, #12639, .F. ) ;
#5447 = CARTESIAN_POINT ( 'NONE',  ( 51.98914612709257455, 0.7788013043310292316, -1.433123603079363484 ) ) ;
#5448 = CARTESIAN_POINT ( 'NONE',  ( 53.60445531103937356, 4.614871059762981176, -2.050000000000186784 ) ) ;
#5449 = DIRECTION ( 'NONE',  ( 1.000000000000000000, 1.047444401652940007E-14, 0.000000000000000000 ) ) ;
#5450 = CIRCLE ( 'NONE', #7464, 0.09999999999999979738 ) ;
#5451 = DIRECTION ( 'NONE',  ( 1.000000000000000000, 1.047444401652940007E-14, 0.000000000000000000 ) ) ;
#5452 = CARTESIAN_POINT ( 'NONE',  ( 57.02888566337306031, -0.7456496514153734267, 2.424120212325347357 ) ) ;
#5453 = TOROIDAL_SURFACE ( 'NONE', #30718, 4.500000000000037303, 0.1000000000000000056 ) ;
#5454 = ADVANCED_FACE ( 'NONE', ( #24994 ), #1104, .T. ) ;
#5455 = AXIS2_PLACEMENT_3D ( 'NONE', #25705, #30928, #17849 ) ;
#5457 = DIRECTION ( 'NONE',  ( 1.000000000000000000, 1.047444401652940007E-14, 0.000000000000000000 ) ) ;
#5456 = CARTESIAN_POINT ( 'NONE',  ( 69.20000000000001705, -0.6441176470588234615, -1.707553061181373621 ) ) ;
#5458 = CARTESIAN_POINT ( 'NONE',  ( 51.70000000000003837, 6.982261990806648555E-14, 4.599999999999857536 ) ) ;
#5459 = CYLINDRICAL_SURFACE ( 'NONE', #18545, 0.04999999999999991257 ) ;
#5460 = AXIS2_PLACEMENT_3D ( 'NONE', #22120, #413, #17206 ) ;
#5461 = CYLINDRICAL_SURFACE ( 'NONE', #1065, 0.05000000000000143219 ) ;
#5462 = CARTESIAN_POINT ( 'NONE',  ( 51.87765138016307986, 8.698644590117595499, -2.050000000000180123 ) ) ;
#5463 = ORIENTED_EDGE ( 'NONE', *, *, #3201, .F. ) ;
#5464 = ORIENTED_EDGE ( 'NONE', *, *, #23542, .F. ) ;
#5465 = ORIENTED_EDGE ( 'NONE', *, *, #5759, .T. ) ;
#5466 = CARTESIAN_POINT ( 'NONE',  ( -62.09902692368709154, -2.508428807930398019, -0.2888567384445905328 ) ) ;
#5467 = CARTESIAN_POINT ( 'NONE',  ( -57.23542740578360366, 2.936324665650207333, 2.606018187048499080 ) ) ;
#5469 = CYLINDRICAL_SURFACE ( 'NONE', #21606, 0.1000000000000000472 ) ;
#5468 = DIRECTION ( 'NONE',  ( 0.000000000000000000, -0.2008964009354147484, 0.9796124928211139560 ) ) ;
#5470 = ORIENTED_EDGE ( 'NONE', *, *, #10588, .F. ) ;
#5471 = ORIENTED_EDGE ( 'NONE', *, *, #16202, .F. ) ;
#5472 = CARTESIAN_POINT ( 'NONE',  ( -56.09585481156723574, -2.489203624310586616, 2.804704140674918023 ) ) ;
#5473 = AXIS2_PLACEMENT_3D ( 'NONE', #13711, #30194, #10722 ) ;
#5474 = ORIENTED_EDGE ( 'NONE', *, *, #25732, .F. ) ;
#5475 = ADVANCED_FACE ( 'NONE', ( #17893 ), #27529, .T. ) ;
#5476 = CARTESIAN_POINT ( 'NONE',  ( 58.75000000000002132, 6.153735859711025284E-13, 3.111507638930570854E-58 ) ) ;
#5477 = ORIENTED_EDGE ( 'NONE', *, *, #30308, .F. ) ;
#5478 = CARTESIAN_POINT ( 'NONE',  ( 26.61920844897797167, 5.219578739559237235, -2.050000000000091305 ) ) ;
#5479 = CARTESIAN_POINT ( 'NONE',  ( -58.31249999999997868, 4.108500314926515351, -1.367561758111400128 ) ) ;
#5480 = CARTESIAN_POINT ( 'NONE',  ( -71.44999999999998863, 0.3062499654112550429, -1.493338310920502066 ) ) ;
#5481 = CARTESIAN_POINT ( 'NONE',  ( 15.41170998834774508, -5.326676561279859001, -0.9978806102896248253 ) ) ;
#5482 = CARTESIAN_POINT ( 'NONE',  ( -57.58155989232413674, -1.962990915244731571, 3.399999999999786748 ) ) ;
#5483 = CARTESIAN_POINT ( 'NONE',  ( 53.05367528747407135, 8.375580747031634132, -2.050000000000184563 ) ) ;
#5484 = FACE_OUTER_BOUND ( 'NONE', #7077, .T. ) ;
#5485 = EDGE_CURVE ( 'NONE', #23938, #1800, #26785, .T. ) ;
#5486 = CARTESIAN_POINT ( 'NONE',  ( 19.23646557533807666, -1.947877022684209034E-15, 0.000000000000000000 ) ) ;
#5487 = CYLINDRICAL_SURFACE ( 'NONE', #14977, 0.5000000000000000000 ) ;
#5488 = CARTESIAN_POINT ( 'NONE',  ( -35.98952425903313213, -3.426725954212505698, -3.937891351789589489 ) ) ;
#5489 = CIRCLE ( 'NONE', #12554, 0.1499999999999999667 ) ;
#5490 = AXIS2_PLACEMENT_3D ( 'NONE', #5911, #13312, #25370 ) ;
#5491 = DIRECTION ( 'NONE',  ( 0.000000000000000000, -1.000000000000000000, -3.491481338843252079E-15 ) ) ;
#5492 = CARTESIAN_POINT ( 'NONE',  ( 51.08379317338048509, -0.8723108729827115937, 1.374656996893404148 ) ) ;
#5493 = VERTEX_POINT ( 'NONE', #25630 ) ;
#5494 = DIRECTION ( 'NONE',  ( 1.000000000000000000, 0.000000000000000000, 0.000000000000000000 ) ) ;
#5495 = EDGE_CURVE ( 'NONE', #7645, #518, #29307, .T. ) ;
#5496 = PLANE ( 'NONE',  #16590 ) ;
#5497 = CARTESIAN_POINT ( 'NONE',  ( 54.38981447126021607, 6.361385918223966485, 2.043118800226060294 ) ) ;
#5498 = ORIENTED_EDGE ( 'NONE', *, *, #13248, .F. ) ;
#5499 = CARTESIAN_POINT ( 'NONE',  ( -44.59999999999997300, 8.366749974758367693E-15, -1.870876429524646202E-13 ) ) ;
#5500 = VERTEX_POINT ( 'NONE', #20894 ) ;
#5501 = CARTESIAN_POINT ( 'NONE',  ( 53.81176349924870550, 5.730864617276226980, 1.682988280464426722 ) ) ;
#5502 = CARTESIAN_POINT ( 'NONE',  ( -54.78335481156724285, 3.238593381231848145, 2.874284765127022023 ) ) ;
#5504 = CARTESIAN_POINT ( 'NONE',  ( -61.82790928944205433, -2.612260643635529345, -0.4142152978364393445 ) ) ;
#5503 = CARTESIAN_POINT ( 'NONE',  ( 58.66133336607590820, 0.9657121834149602346, 1.607522887372458076 ) ) ;
#5505 = ORIENTED_EDGE ( 'NONE', *, *, #3362, .F. ) ;
#5506 = CARTESIAN_POINT ( 'NONE',  ( -59.19999999999997442, 2.395752775956333291, 1.250136525132548693 ) ) ;
#5507 = ADVANCED_FACE ( 'NONE', ( #3945 ), #21382, .F. ) ;
#5508 = DIRECTION ( 'NONE',  ( -1.000000000000000000, 0.000000000000000000, 0.000000000000000000 ) ) ;
#5509 = ORIENTED_EDGE ( 'NONE', *, *, #24581, .F. ) ;
#5511 = DIRECTION ( 'NONE',  ( 0.000000000000000000, 0.000000000000000000, 1.000000000000000000 ) ) ;
#5510 = CARTESIAN_POINT ( 'NONE',  ( -35.85663232820584057, -5.086913985776159386, 1.171642053949095930 ) ) ;
#5512 = CARTESIAN_POINT ( 'NONE',  ( 46.90000000000001279, -4.131056160354152240, -1.100000000000000089 ) ) ;
#5513 = CARTESIAN_POINT ( 'NONE',  ( -57.37499999999997158, 1.184343223768590470, 3.558065644182724974 ) ) ;
#5514 = CARTESIAN_POINT ( 'NONE',  ( -62.14999999999998437, 1.152747360993128871E-15, 2.207939306294521009E-15 ) ) ;
#5515 = CARTESIAN_POINT ( 'NONE',  ( 58.72200624034153549, 1.634766674885311133, -0.9185080301418440119 ) ) ;
#5516 = COLOUR_RGB ( '', 0.66274510, 0.83137255, 0.94901961) ;
#5517 = TOROIDAL_SURFACE ( 'NONE', #9038, 2.750000000000000000, 0.1000000000000000056 ) ;
#5518 = CARTESIAN_POINT ( 'NONE',  ( -54.49999999999995737, -3.612379848390220083, -0.8198014738740030394 ) ) ;
#5519 = CARTESIAN_POINT ( 'NONE',  ( -44.49999999999999289, -1.499999999999999556, 4.029888335921975262 ) ) ;
#5520 =( BOUNDED_CURVE ( )  B_SPLINE_CURVE ( 3, ( #31297, #9628, #11986, #21674 ),
 .UNSPECIFIED., .F., .T. ) 
 B_SPLINE_CURVE_WITH_KNOTS ( ( 4, 4 ),
 ( 1.070062165543571808, 1.185496055862915066 ),
 .UNSPECIFIED. ) 
 CURVE ( )  GEOMETRIC_REPRESENTATION_ITEM ( )  RATIONAL_B_SPLINE_CURVE ( ( 1.000000000000000000, 0.9988898929684264516, 0.9988898929684264516, 1.000000000000000000 ) ) 
 REPRESENTATION_ITEM ( '' )  );
#5521 = CARTESIAN_POINT ( 'NONE',  ( 69.20000000000003126, 1.401298464324817071E-42, -7.248315259438346108E-13 ) ) ;
#5522 = CARTESIAN_POINT ( 'NONE',  ( -62.09999999999997300, -2.737532885411323669, 0.2608613065085638727 ) ) ;
#5523 = ORIENTED_EDGE ( 'NONE', *, *, #10430, .T. ) ;
#5524 = EDGE_CURVE ( 'NONE', #29235, #10512, #19723, .T. ) ;
#5525 = CARTESIAN_POINT ( 'NONE',  ( 15.95705409078441583, 3.646557212684218729, 3.995389720703451886 ) ) ;
#5526 = CIRCLE ( 'NONE', #24249, 0.1500000000000001887 ) ;
#5527 = DIRECTION ( 'NONE',  ( -1.000000000000000000, -3.053848253006669023E-16, 2.042510438544995415E-16 ) ) ;
#5528 = CIRCLE ( 'NONE', #25256, 0.09999999999999982514 ) ;
#5529 = CARTESIAN_POINT ( 'NONE',  ( 54.50000000000002132, 0.000000000000000000, -3.299999999999999822 ) ) ;
#5530 = EDGE_CURVE ( 'NONE', #7506, #28771, #6961, .T. ) ;
#5531 = CARTESIAN_POINT ( 'NONE',  ( -59.38452994616203995, 3.117691453623969711, 1.799999999999819522 ) ) ;
#5532 = DIRECTION ( 'NONE',  ( 0.000000000000000000, 0.9985773570673159849, -0.05332224631853133001 ) ) ;
#5533 = CARTESIAN_POINT ( 'NONE',  ( 30.66094943579030385, 7.112308407316297654, 2.049999999999892797 ) ) ;
#5534 = EDGE_LOOP ( 'NONE', ( #18806, #3559, #3813, #17504 ) ) ;
#5535 = AXIS2_PLACEMENT_3D ( 'NONE', #19536, #22064, #17301 ) ;
#5536 = CARTESIAN_POINT ( 'NONE',  ( -73.89999999999997726, -2.435524336289708093E-15, 4.607889071584891164E-15 ) ) ;
#5537 = EDGE_LOOP ( 'NONE', ( #10568, #7069, #10179, #17539 ) ) ;
#5538 = CARTESIAN_POINT ( 'NONE',  ( -59.18700104863290079, 2.529210612537639680, -0.9442207491878787939 ) ) ;
#5539 = B_SPLINE_CURVE_WITH_KNOTS ( 'NONE', 3,
 ( #29076, #2319, #2010, #16595, #14509, #23548, #1846, #16417, #24183, #11522, #21199, #12143, #14031, #6758, #30829, #9148, #21354, #11824, #30981 ),
 .UNSPECIFIED., .F., .F.,
 ( 4, 2, 2, 2, 1, 2, 2, 2, 2, 4 ),
 ( 0.5315346799924233201, 0.6486510099942875973, 0.7072091749952189588, 0.7364882574956834738, 0.7438080281207990474, 0.7474679134333586106, 0.7511277987459183958, 0.7657673399961579808, 0.8828836699980789904, 1.000000000000000000 ),
 .UNSPECIFIED. ) ;
#5541 = CARTESIAN_POINT ( 'NONE',  ( -35.85663232820584057, -2.199885893005943949, -4.939696249117691451 ) ) ;
#5540 = CARTESIAN_POINT ( 'NONE',  ( 60.75000000000002842, -0.7499999999993639532, -1.718465885608440269 ) ) ;
#5542 = ORIENTED_EDGE ( 'NONE', *, *, #18455, .T. ) ;
#5543 = EDGE_LOOP ( 'NONE', ( #28133, #15373, #7472, #9372 ) ) ;
#5544 = CARTESIAN_POINT ( 'NONE',  ( 51.17957687186121518, -0.9671124184258252932, 1.523623459118159440 ) ) ;
#5545 = VECTOR ( 'NONE', #26815, 1000.000000000000114 ) ;
#5546 = EDGE_CURVE ( 'NONE', #30852, #28320, #21529, .T. ) ;
#5547 = DIRECTION ( 'NONE',  ( 0.000000000000000000, 0.000000000000000000, 1.000000000000000000 ) ) ;
#5548 = ORIENTED_EDGE ( 'NONE', *, *, #10667, .F. ) ;
#5550 = FACE_OUTER_BOUND ( 'NONE', #22031, .T. ) ;
#5549 = CARTESIAN_POINT ( 'NONE',  ( -58.25952994616203284, -3.117691453623963938, -1.800000000000218092 ) ) ;
#5551 = EDGE_CURVE ( 'NONE', #19284, #9698, #16624, .T. ) ;
#5552 = CARTESIAN_POINT ( 'NONE',  ( 50.30000000000001847, 1.391941090707534023, 3.850000000000022737 ) ) ;
#5553 = ADVANCED_FACE ( 'NONE', ( #28331 ), #23275, .T. ) ;
#5554 = CARTESIAN_POINT ( 'NONE',  ( 58.75000000000002132, 6.153735859711025284E-13, 3.111507638930570854E-58 ) ) ;
#5555 = PRODUCT_CONTEXT ( 'NONE', #2661, 'mechanical' ) ;
#5556 = CARTESIAN_POINT ( 'NONE',  ( 58.75000000694009827, -1.346330794793457519, -1.381609951798280500 ) ) ;
#5557 =( BOUNDED_SURFACE ( )  B_SPLINE_SURFACE ( 3, 2, ( 
 ( #26939, #12532, #24416 ),
 ( #22058, #21914, #12682 ),
 ( #24725, #24872, #24562 ),
 ( #19981, #22362, #354 ) ),
 .UNSPECIFIED., .F., .F., .F. ) 
 B_SPLINE_SURFACE_WITH_KNOTS ( ( 4, 4 ),
 ( 3, 3 ),
 ( 6.470519842244164266E-05, 0.0002246728259156070709 ),
 ( 0.000000000000000000, 1.000000000000000000 ),
 .UNSPECIFIED. ) 
 GEOMETRIC_REPRESENTATION_ITEM ( )  RATIONAL_B_SPLINE_SURFACE ( (
 ( 1.000000000000000000, 0.5857791861290068125, 1.000000000000000000),
 ( 1.000000000000000000, 0.5849685391560944803, 1.000000000000000000),
 ( 1.000000000000000000, 0.6585504321673580908, 1.000000000000000000),
 ( 1.000000000000000000, 0.7071067811864985009, 1.000000000000000000) ) ) 
 REPRESENTATION_ITEM ( '' )  SURFACE ( )  );
#5558 = SURFACE_STYLE_USAGE ( .BOTH. , #3333 ) ;
#5559 = ORIENTED_EDGE ( 'NONE', *, *, #13622, .F. ) ;
#5560 = EDGE_CURVE ( 'NONE', #950, #29758, #21243, .T. ) ;
#5561 = AXIS2_PLACEMENT_3D ( 'NONE', #2715, #9705, #4621 ) ;
#5562 = CARTESIAN_POINT ( 'NONE',  ( -60.00952994616204705, -4.643455692769866465E-15, 3.599999999999786038 ) ) ;
#5563 = CARTESIAN_POINT ( 'NONE',  ( 53.81176349924876945, 5.730864617276189676, -2.050000000000250289 ) ) ;
#5564 = CARTESIAN_POINT ( 'NONE',  ( 48.45124641917420405, -1.383300983803864570, -3.859740869727656953 ) ) ;
#5565 = CARTESIAN_POINT ( 'NONE',  ( 15.48686146417450082, 0.1108756495953548971, 5.200000001674996319 ) ) ;
#5566 = CARTESIAN_POINT ( 'NONE',  ( -57.22499999999997300, 0.9241234443029110457, -4.506217466977124886 ) ) ;
#5567 = TOROIDAL_SURFACE ( 'NONE', #22791, 4.199999999999993072, 0.1000000000000000056 ) ;
#5568 = DIRECTION ( 'NONE',  ( 0.000000000000000000, 0.000000000000000000, 1.000000000000000000 ) ) ;
#5570 = DIRECTION ( 'NONE',  ( 0.000000000000000000, -0.5454670984325209471, -0.8381322357048476279 ) ) ;
#5569 = LINE ( 'NONE', #3032, #30204 ) ;
#5571 = EDGE_CURVE ( 'NONE', #30944, #13383, #2005, .T. ) ;
#5572 = CYLINDRICAL_SURFACE ( 'NONE', #24612, 0.1500000000000001887 ) ;
#5573 = LINE ( 'NONE', #3801, #28114 ) ;
#5575 = LINE ( 'NONE', #15069, #23580 ) ;
#5574 = DIRECTION ( 'NONE',  ( -0.000000000000000000, -0.000000000000000000, 1.000000000000000000 ) ) ;
#5576 = ORIENTED_EDGE ( 'NONE', *, *, #6988, .F. ) ;
#5577 = CIRCLE ( 'NONE', #23284, 4.849999999999999645 ) ;
#5578 = CARTESIAN_POINT ( 'NONE',  ( 50.41047473690879599, -0.7808213810458148885, -4.027268569371626583 ) ) ;
#5579 = EDGE_CURVE ( 'NONE', #4338, #29960, #23424, .T. ) ;
#5580 = CARTESIAN_POINT ( 'NONE',  ( 47.12430284249615653, -4.150085526745831643, -1.728112049830362151 ) ) ;
#5582 = DIRECTION ( 'NONE',  ( 0.000000000000000000, -1.000000000000000000, -3.491481338843131383E-15 ) ) ;
#5581 = CARTESIAN_POINT ( 'NONE',  ( 15.03925126672127810, 3.426725943139600439, -3.937891353488703228 ) ) ;
#5583 = CARTESIAN_POINT ( 'NONE',  ( 47.73576178058490171, -4.410640387331298484, 1.311048612304915428 ) ) ;
#5584 = ORIENTED_EDGE ( 'NONE', *, *, #23141, .F. ) ;
#5585 = CARTESIAN_POINT ( 'NONE',  ( -61.39999999999998437, -2.652806974455509170, 0.5026083527760007996 ) ) ;
#5586 = CARTESIAN_POINT ( 'NONE',  ( 51.80000000000001847, -4.259181259350203419, 1.099999999999999645 ) ) ;
#5587 = ORIENTED_EDGE ( 'NONE', *, *, #19396, .F. ) ;
#5588 = EDGE_CURVE ( 'NONE', #23827, #12035, #13598, .T. ) ;
#5589 = CARTESIAN_POINT ( 'NONE',  ( 69.25000000000000000, -0.6441176470588234615, -1.707553061181374066 ) ) ;
#5590 = EDGE_LOOP ( 'NONE', ( #4181, #8795, #9087, #23539, #1837 ) ) ;
#5591 = VERTEX_POINT ( 'NONE', #18995 ) ;
#5592 = EDGE_CURVE ( 'NONE', #13616, #24615, #28644, .T. ) ;
#5593 = DIRECTION ( 'NONE',  ( -2.581436205204234499E-16, 0.9796124928211140670, 0.2008964009354147762 ) ) ;
#5594 = VERTEX_POINT ( 'NONE', #23895 ) ;
#5595 =( NAMED_UNIT ( * ) PLANE_ANGLE_UNIT ( ) SI_UNIT ( $, .RADIAN. ) );
#5596 = CIRCLE ( 'NONE', #19265, 0.1000000000000000472 ) ;
#5597 = CARTESIAN_POINT ( 'NONE',  ( 33.97474581211285027, 8.173393014830729442, 1.949999999999881606 ) ) ;
#5598 = CARTESIAN_POINT ( 'NONE',  ( -55.45655989232413674, 1.962990915244722245, 3.399999999999810285 ) ) ;
#5599 = EDGE_LOOP ( 'NONE', ( #21634, #20050, #23505, #9460 ) ) ;
#5600 = DIRECTION ( 'NONE',  ( 3.304235192336781034E-15, 0.000000000000000000, 1.000000000000000000 ) ) ;
#5601 = CARTESIAN_POINT ( 'NONE',  ( 51.80000000000001137, 3.954022803064791702, -2.040489002254654682 ) ) ;
#5602 = CARTESIAN_POINT ( 'NONE',  ( 22.72181155399538355, 6.520914524688622649, 1.949999999999919575 ) ) ;
#5603 = ORIENTED_EDGE ( 'NONE', *, *, #3930, .T. ) ;
#5604 = CARTESIAN_POINT ( 'NONE',  ( 52.10126625705171222, 0.5195911883743921100, -1.546252172343136611 ) ) ;
#5605 = CARTESIAN_POINT ( 'NONE',  ( 60.75000000000001421, 0.6500000000006364020, 1.489337100860647967 ) ) ;
#5606 = DIRECTION ( 'NONE',  ( 1.000000000000000000, 1.047444401652940007E-14, 0.000000000000000000 ) ) ;
#5607 = DIRECTION ( 'NONE',  ( 0.000000000000000000, 0.000000000000000000, -1.000000000000000000 ) ) ;
#5608 = CARTESIAN_POINT ( 'NONE',  ( 51.27853981583098886, 1.002608958138269113, 1.395204572094398854 ) ) ;
#5610 = FACE_OUTER_BOUND ( 'NONE', #21742, .T. ) ;
#5609 = CARTESIAN_POINT ( 'NONE',  ( 58.75000000000001421, 0.5380862305915415922, -2.008165151417984351 ) ) ;
#5611 = EDGE_CURVE ( 'NONE', #14068, #11253, #4010, .T. ) ;
#5612 = CARTESIAN_POINT ( 'NONE',  ( 50.42215036618306812, -1.308847734660468332, -3.885629509820973659 ) ) ;
#5613 = EDGE_CURVE ( 'NONE', #24531, #9415, #13891, .T. ) ;
#5614 = CARTESIAN_POINT ( 'NONE',  ( -62.04999999999998295, 0.005353951483536231043, -0.2149229472152333897 ) ) ;
#5615 = CARTESIAN_POINT ( 'NONE',  ( -54.49983832461118283, 1.542920080254278181, -3.327619142904491234 ) ) ;
#5616 = CARTESIAN_POINT ( 'NONE',  ( 54.12924440478096244, 6.977429999421167039, -2.050000000000188116 ) ) ;
#5617 = EDGE_CURVE ( 'NONE', #7928, #31291, #9967, .T. ) ;
#5618 = ORIENTED_EDGE ( 'NONE', *, *, #26820, .F. ) ;
#5619 = CARTESIAN_POINT ( 'NONE',  ( -54.47754877553799702, 1.508273929415538062, 3.305418158118663907 ) ) ;
#5620 = ORIENTED_EDGE ( 'NONE', *, *, #16543, .T. ) ;
#5621 = ORIENTED_EDGE ( 'NONE', *, *, #21170, .F. ) ;
#5622 = CARTESIAN_POINT ( 'NONE',  ( -59.17457605456178271, 2.372231461058813107, 1.252354863327886259 ) ) ;
#5623 = CARTESIAN_POINT ( 'NONE',  ( -59.48542740578359656, 2.936324665650206445, 2.606018187048499524 ) ) ;
#5625 = CARTESIAN_POINT ( 'NONE',  ( -61.35067641704169006, -2.574083687496825590, 0.6681602693401289539 ) ) ;
#5624 = DIRECTION ( 'NONE',  ( 1.387778780781445676E-14, -1.000000000000000000, 0.000000000000000000 ) ) ;
#5626 = ORIENTED_EDGE ( 'NONE', *, *, #794, .T. ) ;
#5627 = EDGE_LOOP ( 'NONE', ( #14550, #13842, #4792, #28700 ) ) ;
#5628 = CARTESIAN_POINT ( 'NONE',  ( 53.93368044017396556, 6.673923803580072978, -1.889921144916990592 ) ) ;
#5629 = ORIENTED_EDGE ( 'NONE', *, *, #23923, .F. ) ;
#5630 = CARTESIAN_POINT ( 'NONE',  ( 51.43355796162960303, 0.9748468443439985975, -1.443681521171340520 ) ) ;
#5631 = ORIENTED_EDGE ( 'NONE', *, *, #13596, .T. ) ;
#5632 = CARTESIAN_POINT ( 'NONE',  ( 31.37624803221847358, 7.388935654832122779, -1.950000000000108091 ) ) ;
#5633 = CARTESIAN_POINT ( 'NONE',  ( -62.06710100716626499, -2.504070139480777613, -0.3244344873171103316 ) ) ;
#5634 = CARTESIAN_POINT ( 'NONE',  ( 54.36607077795603971, 6.714235712056784600, 2.039222690360789958 ) ) ;
#5635 = CARTESIAN_POINT ( 'NONE',  ( 16.07279755198655380, -5.034707333629182990, -1.977875755500475563 ) ) ;
#5636 = CARTESIAN_POINT ( 'NONE',  ( -59.76905989232412253, -2.944486372867088697, 1.699999999999776579 ) ) ;
#5637 = CARTESIAN_POINT ( 'NONE',  ( 52.02306152107793480, 3.830941655646746824, -2.050000000000181455 ) ) ;
#5638 = CARTESIAN_POINT ( 'NONE',  ( 47.12288048077186176, -3.662677325876132706, -1.845585774149762326 ) ) ;
#5639 = CARTESIAN_POINT ( 'NONE',  ( -59.19999999999997442, -2.449420067797476452, 1.250136525132531817 ) ) ;
#5640 = LINE ( 'NONE', #17989, #3382 ) ;
#5641 = CARTESIAN_POINT ( 'NONE',  ( 50.34875358082582864, 1.383300983803910089, -3.859740869727648072 ) ) ;
#5642 = DIRECTION ( 'NONE',  ( 3.491481338843133355E-15, 3.491481338843133355E-15, -1.000000000000000000 ) ) ;
#5643 = ADVANCED_FACE ( 'NONE', ( #25791 ), #4099, .F. ) ;
#5644 = CARTESIAN_POINT ( 'NONE',  ( -61.82078168762245696, -2.687023538218675345, 0.2847997227030995560 ) ) ;
#5645 = CIRCLE ( 'NONE', #29914, 0.2500000000000000000 ) ;
#5646 = LINE ( 'NONE', #23523, #3856 ) ;
#5647 = ORIENTED_EDGE ( 'NONE', *, *, #6152, .F. ) ;
#5648 = CARTESIAN_POINT ( 'NONE',  ( -77.29999999999998295, -3.473832742311974792E-15, 5.302342620690189014E-15 ) ) ;
#5649 = CARTESIAN_POINT ( 'NONE',  ( -36.27260443516964017, -3.212533369474692257, -4.093511368021621522 ) ) ;
#5650 = CARTESIAN_POINT ( 'NONE',  ( 54.33836613259588688, 6.362881108852070255, 2.049999999999810196 ) ) ;
#5651 = ORIENTED_EDGE ( 'NONE', *, *, #19296, .T. ) ;
#5652 = DIRECTION ( 'NONE',  ( 1.000000000000000000, 2.586136946169074517E-16, -0.000000000000000000 ) ) ;
#5653 = EDGE_LOOP ( 'NONE', ( #30909, #22533, #28717, #3942 ) ) ;
#5654 = CARTESIAN_POINT ( 'NONE',  ( 52.20711756518984714, -0.6499999999994533484, 1.489337100860647967 ) ) ;
#5655 = CARTESIAN_POINT ( 'NONE',  ( -54.65835481156724995, -0.8699069336946625430, 4.241846523238429256 ) ) ;
#5657 = DIRECTION ( 'NONE',  ( 1.000000000000000000, 1.047444401652940007E-14, 0.000000000000000000 ) ) ;
#5656 = CARTESIAN_POINT ( 'NONE',  ( 48.33022520384532328, -1.142230555601074116, -3.938343097974785767 ) ) ;
#5658 = ORIENTED_EDGE ( 'NONE', *, *, #21538, .F. ) ;
#5659 = DIRECTION ( 'NONE',  ( -1.000000000000000000, 1.219044193948983948E-29, -3.491481338843133355E-15 ) ) ;
#5660 = B_SPLINE_CURVE_WITH_KNOTS ( 'NONE', 3,
 ( #8560, #15372, #27731, #11094 ),
 .UNSPECIFIED., .F., .F.,
 ( 4, 4 ),
 ( 0.000000000000000000, 0.0001000467755295633628 ),
 .UNSPECIFIED. ) ;
#5661 = EDGE_CURVE ( 'NONE', #8932, #15558, #21121, .T. ) ;
#5662 = DIRECTION ( 'NONE',  ( -1.000000000000000000, -0.000000000000000000, -0.000000000000000000 ) ) ;
#5663 = ORIENTED_EDGE ( 'NONE', *, *, #15418, .F. ) ;
#5664 = CARTESIAN_POINT ( 'NONE',  ( -58.08155989232410832, -1.962990915244700707, -3.400000000000216627 ) ) ;
#5665 = ORIENTED_EDGE ( 'NONE', *, *, #16880, .F. ) ;
#5666 = ORIENTED_EDGE ( 'NONE', *, *, #26906, .F. ) ;
#5667 = CARTESIAN_POINT ( 'NONE',  ( 56.95000000000001705, 0.000000000000000000, 0.000000000000000000 ) ) ;
#5668 = CARTESIAN_POINT ( 'NONE',  ( 48.00000000000002132, -4.319730106884873244, 1.256953381662069269 ) ) ;
#5669 = CARTESIAN_POINT ( 'NONE',  ( 58.65000038048046349, 1.580579251836441435, -1.008797009996411642 ) ) ;
#5670 = CIRCLE ( 'NONE', #27905, 2.549999999999999822 ) ;
#5671 = AXIS2_PLACEMENT_3D ( 'NONE', #7054, #26203, #21465 ) ;
#5672 = LINE ( 'NONE', #24506, #9916 ) ;
#5673 = LINE ( 'NONE', #5519, #13169 ) ;
#5674 = DIRECTION ( 'NONE',  ( 0.000000000000000000, 0.000000000000000000, -1.000000000000000000 ) ) ;
#5675 = ORIENTED_EDGE ( 'NONE', *, *, #15556, .F. ) ;
#5676 = CARTESIAN_POINT ( 'NONE',  ( 15.41080140630217343, 2.595266697484422291, 4.757426534476680402 ) ) ;
#5677 = B_SPLINE_CURVE_WITH_KNOTS ( 'NONE', 3,
 ( #20641, #6208, #3824, #15563, #23167, #11108, #25211, #8720, #28041, #22529 ),
 .UNSPECIFIED., .F., .F.,
 ( 4, 2, 2, 2, 4 ),
 ( 0.000000000000000000, 0.0003600849014046848253, 0.0007201698028093696507, 0.001080254704214054368, 0.001440339605618739301 ),
 .UNSPECIFIED. ) ;
#5678 = CARTESIAN_POINT ( 'NONE',  ( -55.29792740578360366, -1.073804522883514467, -3.225979517392337126 ) ) ;
#5679 = EDGE_CURVE ( 'NONE', #13873, #14560, #21649, .T. ) ;
#5680 = DIRECTION ( 'NONE',  ( 0.000000000000000000, -1.000000000000000000, -3.491481338843132961E-15 ) ) ;
#5681 = EDGE_CURVE ( 'NONE', #6673, #13582, #7970, .T. ) ;
#5682 = CARTESIAN_POINT ( 'NONE',  ( -58.57202994616204705, 2.078460969082640997, 3.599999999999802025 ) ) ;
#5683 = CARTESIAN_POINT ( 'NONE',  ( -36.38012252111052902, 1.026563698233470268, 5.312790900508079339 ) ) ;
#5684 = CARTESIAN_POINT ( 'NONE',  ( 48.37840743871460347, 1.310166284604407760, -3.885185101012171849 ) ) ;
#5685 = EDGE_LOOP ( 'NONE', ( #25079, #457, #23739, #268 ) ) ;
#5686 = DIRECTION ( 'NONE',  ( -2.117927888850090838E-16, 0.02490330187381123786, -0.9996898646859343485 ) ) ;
#5687 = ORIENTED_EDGE ( 'NONE', *, *, #21865, .F. ) ;
#5688 = PRODUCT_DEFINITION_CONTEXT ( 'detailed design', #27395, 'design' ) ;
#5689 = CARTESIAN_POINT ( 'NONE',  ( 50.40746642207054151, -1.341874354110735634, 3.874311046529113511 ) ) ;
#5691 = CARTESIAN_POINT ( 'NONE',  ( 58.65000000000003411, -1.253243060178391932, 1.394635017527226628 ) ) ;
#5690 = CARTESIAN_POINT ( 'NONE',  ( 15.41170998834775041, -3.722832355336850529, -3.938244298533932319 ) ) ;
#5692 = ORIENTED_EDGE ( 'NONE', *, *, #9215, .T. ) ;
#5693 = ORIENTED_EDGE ( 'NONE', *, *, #17110, .F. ) ;
#5694 = DIRECTION ( 'NONE',  ( 1.000000000000000000, -1.219044193948983948E-29, 3.491481338843133355E-15 ) ) ;
#5695 = ADVANCED_FACE ( 'NONE', ( #29554 ), #29699, .T. ) ;
#5696 = DIRECTION ( 'NONE',  ( 0.000000000000000000, 0.9996898646859344595, 0.02490330187381124133 ) ) ;
#5697 = EDGE_LOOP ( 'NONE', ( #17193, #25746, #19664, #3732 ) ) ;
#5699 = CARTESIAN_POINT ( 'NONE',  ( 51.74134002894188455, -4.175606900721715142, 1.008275291528680562 ) ) ;
#5698 = CARTESIAN_POINT ( 'NONE',  ( -58.69702994616204705, 4.156921938165313080, -1.932741547809596393E-13 ) ) ;
#5700 =( BOUNDED_CURVE ( )  B_SPLINE_CURVE ( 3, ( #24137, #28884, #7343, #14306 ),
 .UNSPECIFIED., .F., .T. ) 
 B_SPLINE_CURVE_WITH_KNOTS ( ( 4, 4 ),
 ( 1.454199501120267524, 2.189070931013918031 ),
 .UNSPECIFIED. ) 
 CURVE ( )  GEOMETRIC_REPRESENTATION_ITEM ( )  RATIONAL_B_SPLINE_CURVE ( ( 1.000000000000000000, 0.9555010429016485007, 0.9555010429016485007, 1.000000000000000000 ) ) 
 REPRESENTATION_ITEM ( '' )  );
#5701 = CARTESIAN_POINT ( 'NONE',  ( 50.32627973729707094, 1.373706569044511605, 3.853361913240786585 ) ) ;
#5702 = CIRCLE ( 'NONE', #21407, 2.000000000000000000 ) ;
#5703 = CARTESIAN_POINT ( 'NONE',  ( 68.00000000000001421, 1.401298464324817071E-42, -7.122621931239992550E-13 ) ) ;
#5704 = DIRECTION ( 'NONE',  ( 1.000000000000000000, 0.000000000000000000, 0.000000000000000000 ) ) ;
#5705 = CARTESIAN_POINT ( 'NONE',  ( -59.29999999999999005, -3.566666717976950007, 0.2440603095767059916 ) ) ;
#5706 = EDGE_CURVE ( 'NONE', #26067, #26007, #895, .T. ) ;
#5707 = ORIENTED_EDGE ( 'NONE', *, *, #21609, .T. ) ;
#5708 = DIRECTION ( 'NONE',  ( 0.000000000000000000, 1.000000000000000000, 0.000000000000000000 ) ) ;
#5709 = CARTESIAN_POINT ( 'NONE',  ( 53.53640187423184216, 5.215699251213393062, -2.050000000000122835 ) ) ;
#5710 = DIRECTION ( 'NONE',  ( 0.000000000000000000, 0.2008964009354148039, -0.9796124928211140670 ) ) ;
#5711 = CARTESIAN_POINT ( 'NONE',  ( 15.76623786017542272, -0.1071614981651040632, 5.407381887150171984 ) ) ;
#5712 = CARTESIAN_POINT ( 'NONE',  ( -59.69591307118649581, -2.246549767191792668, 1.536452070276721926 ) ) ;
#5713 = EDGE_CURVE ( 'NONE', #596, #25040, #2979, .T. ) ;
#5715 = CARTESIAN_POINT ( 'NONE',  ( -35.85663232820596136, 0.7747498368337510932, -5.363501452440939232 ) ) ;
#5714 = CARTESIAN_POINT ( 'NONE',  ( -56.81249999999995737, -1.962990915244703150, -3.400000000000210409 ) ) ;
#5716 = EDGE_CURVE ( 'NONE', #9190, #23361, #26670, .T. ) ;
#5717 = AXIS2_PLACEMENT_3D ( 'NONE', #15843, #4125, #13761 ) ;
#5718 = EDGE_CURVE ( 'NONE', #16074, #5072, #27173, .T. ) ;
#5719 = DIRECTION ( 'NONE',  ( -6.842565855738836309E-15, 0.4857787595540328796, -0.8740818021021518058 ) ) ;
#5720 = CARTESIAN_POINT ( 'NONE',  ( 52.34995357322210907, 3.980947253423499532, -2.045629398349763317 ) ) ;
#5722 = CARTESIAN_POINT ( 'NONE',  ( -54.49999999999997868, 1.522428981461833253, -3.138047051316147140 ) ) ;
#5721 = DIRECTION ( 'NONE',  ( 0.000000000000000000, 1.000000000000000000, 0.000000000000000000 ) ) ;
#5723 = EDGE_LOOP ( 'NONE', ( #17170, #9498, #24346, #6791 ) ) ;
#5724 = CARTESIAN_POINT ( 'NONE',  ( 50.31907412294955861, -1.391939743175890420, -3.849999999996903899 ) ) ;
#5725 = CARTESIAN_POINT ( 'NONE',  ( -36.00197790576392265, 4.018128179617553641, -3.618665901676621388 ) ) ;
#5727 = PLANE ( 'NONE',  #21750 ) ;
#5726 = CARTESIAN_POINT ( 'NONE',  ( 15.29384114148379759, 3.378548217643521756, -3.972894518062563662 ) ) ;
#5728 = CARTESIAN_POINT ( 'NONE',  ( 15.03925126672132961, 3.275050215668553921, 2.949461045527632219 ) ) ;
#5729 = ORIENTED_EDGE ( 'NONE', *, *, #2818, .T. ) ;
#5730 = CARTESIAN_POINT ( 'NONE',  ( 61.01502350126983742, -0.5557829358550897547, 1.706838207573794453 ) ) ;
#5731 = CARTESIAN_POINT ( 'NONE',  ( -54.49999999999997868, 1.734723475976807094E-15, -4.375000000000000000 ) ) ;
#5732 = ADVANCED_FACE ( 'NONE', ( #7718 ), #24666, .T. ) ;
#5733 =( BOUNDED_CURVE ( )  B_SPLINE_CURVE ( 2, ( #23565, #21212, #13870, #6620, #26250, #18506, #11206, #6470, #16127 ),
 .UNSPECIFIED., .F., .T. ) 
 B_SPLINE_CURVE_WITH_KNOTS ( ( 3, 2, 2, 2, 3 ),
 ( 0.1944444444444444475, 0.2037037037037036924, 0.2222222222222222099, 0.2407407407407407274, 0.2500000000000000000 ),
 .UNSPECIFIED. ) 
 CURVE ( )  GEOMETRIC_REPRESENTATION_ITEM ( )  RATIONAL_B_SPLINE_CURVE ( ( 0.9330127018922192983, 0.9330127018922194093, 1.000000000000000000, 0.8660254037844387076, 1.000000000000000000, 0.8660254037844387076, 1.000000000000000000, 0.9330127018922191873, 0.9330127018922192983 ) ) 
 REPRESENTATION_ITEM ( '' )  );
#5734 = EDGE_LOOP ( 'NONE', ( #9256, #29772, #27898, #15881 ) ) ;
#5735 = CARTESIAN_POINT ( 'NONE',  ( 15.70940947763171280, -4.797009389500164644, 2.498041539401808731 ) ) ;
#5736 = EDGE_LOOP ( 'NONE', ( #1295, #10656, #15055, #28592 ) ) ;
#5737 = VERTEX_POINT ( 'NONE', #29408 ) ;
#5738 = CARTESIAN_POINT ( 'NONE',  ( 15.03925126672132606, 5.340403872473315161, 0.9205822173396651653 ) ) ;
#5739 = FACE_OUTER_BOUND ( 'NONE', #8033, .T. ) ;
#5740 = ORIENTED_EDGE ( 'NONE', *, *, #22553, .F. ) ;
#5741 =( LENGTH_UNIT ( ) NAMED_UNIT ( * ) SI_UNIT ( .MILLI., .METRE. ) );
#5742 = CARTESIAN_POINT ( 'NONE',  ( 51.37201957452462153, 0.9974676312069150619, -1.404527551348820680 ) ) ;
#5743 = CARTESIAN_POINT ( 'NONE',  ( -59.63452994616203284, 2.093608279459373297E-14, -3.600000000000211475 ) ) ;
#5744 = ORIENTED_EDGE ( 'NONE', *, *, #25274, .T. ) ;
#5745 = FACE_OUTER_BOUND ( 'NONE', #14542, .T. ) ;
#5746 = PLANE ( 'NONE',  #24814 ) ;
#5747 = AXIS2_PLACEMENT_3D ( 'NONE', #12234, #24419, #10166 ) ;
#5748 = EDGE_CURVE ( 'NONE', #23038, #26062, #22131, .T. ) ;
#5749 = CARTESIAN_POINT ( 'NONE',  ( 24.76493886322414539, 5.404133871203915973, 2.049999999999914557 ) ) ;
#5750 = EDGE_LOOP ( 'NONE', ( #22041, #3805, #23300, #4258 ) ) ;
#5751 = CARTESIAN_POINT ( 'NONE',  ( -55.18749999999996447, 1.962990915244749557, -3.400000000000187317 ) ) ;
#5752 = PLANE ( 'NONE',  #15497 ) ;
#5753 = DIRECTION ( 'NONE',  ( 0.000000000000000000, 0.000000000000000000, 1.000000000000000000 ) ) ;
#5754 = DIRECTION ( 'NONE',  ( 3.002035892788117459E-16, -0.9996898646859344595, -0.02490330187381124133 ) ) ;
#5755 = CARTESIAN_POINT ( 'NONE',  ( 58.45000000000001705, -0.7500000000000000000, 1.778341924377873751 ) ) ;
#5756 = EDGE_CURVE ( 'NONE', #11417, #9170, #374, .T. ) ;
#5758 = FACE_BOUND ( 'NONE', #23684, .T. ) ;
#5757 = DIRECTION ( 'NONE',  ( -1.000000000000000000, -3.054025858079668409E-16, 2.042474015755241579E-16 ) ) ;
#5759 = EDGE_CURVE ( 'NONE', #25198, #27301, #19312, .T. ) ;
#5760 = EDGE_CURVE ( 'NONE', #3125, #1800, #26161, .T. ) ;
#5761 = DIRECTION ( 'NONE',  ( -1.000000000000000000, 0.000000000000000000, 1.047444401652940007E-14 ) ) ;
#5762 = CARTESIAN_POINT ( 'NONE',  ( -54.39999999999996305, -1.499999999999978684, -4.029888335922192866 ) ) ;
#5763 = DIRECTION ( 'NONE',  ( 1.000000000000000000, 1.047444401652940007E-14, 0.000000000000000000 ) ) ;
#5764 = CARTESIAN_POINT ( 'NONE',  ( 58.74154451056411830, 1.390058629629814968, -1.258335925859399351 ) ) ;
#5765 = CARTESIAN_POINT ( 'NONE',  ( 59.00000000000006395, 4.898587196589412829E-16, 3.999999999999382716 ) ) ;
#5766 = TOROIDAL_SURFACE ( 'NONE', #10801, 14.70000000000000995, 10.00000000000000000 ) ;
#5767 = ORIENTED_EDGE ( 'NONE', *, *, #30368, .F. ) ;
#5768 = DIRECTION ( 'NONE',  ( -0.9993908270190957621, 0.03489949670250097613, 3.491481338843133355E-15 ) ) ;
#5769 = ORIENTED_EDGE ( 'NONE', *, *, #17993, .T. ) ;
#5770 = ORIENTED_EDGE ( 'NONE', *, *, #3647, .T. ) ;
#5771 = LINE ( 'NONE', #15596, #8326 ) ;
#5772 = CARTESIAN_POINT ( 'NONE',  ( -59.61042740578360366, 3.725040285533370632, -1.239922660687675204 ) ) ;
#5774 = CARTESIAN_POINT ( 'NONE',  ( -61.39959552429773737, -2.604566667188200846, 0.7115002142985770162 ) ) ;
#5773 = CARTESIAN_POINT ( 'NONE',  ( -55.81249999999997158, 3.925981830489463142, -1.840516183884902743E-13 ) ) ;
#5775 = EDGE_LOOP ( 'NONE', ( #17243, #15702 ) ) ;
#5776 = ORIENTED_EDGE ( 'NONE', *, *, #3230, .T. ) ;
#5777 = AXIS2_PLACEMENT_3D ( 'NONE', #26484, #31247, #11279 ) ;
#5778 = CARTESIAN_POINT ( 'NONE',  ( -55.81684846062113792, -0.2309624077929039732, -3.875409454552791733 ) ) ;
#5779 = VERTEX_POINT ( 'NONE', #2809 ) ;
#5780 = CARTESIAN_POINT ( 'NONE',  ( 48.40000000000001990, -1.409787217987148233, -3.950000000000022826 ) ) ;
#5781 = ORIENTED_EDGE ( 'NONE', *, *, #3591, .T. ) ;
#5782 = DIRECTION ( 'NONE',  ( 0.000000000000000000, 0.000000000000000000, 1.000000000000000000 ) ) ;
#5783 = DIRECTION ( 'NONE',  ( 0.000000000000000000, -1.000000000000000000, -3.491481338843137694E-15 ) ) ;
#5784 = ADVANCED_FACE ( 'NONE', ( #2353 ), #13507, .T. ) ;
#5785 = CARTESIAN_POINT ( 'NONE',  ( 48.40000000000001990, 2.428612866367529932E-14, 0.000000000000000000 ) ) ;
#5786 = AXIS2_PLACEMENT_3D ( 'NONE', #27835, #24824, #3137 ) ;
#5787 = CARTESIAN_POINT ( 'NONE',  ( 16.10624235918718128, -5.092377074781565760, -1.825725187625025780 ) ) ;
#5788 = EDGE_CURVE ( 'NONE', #24125, #16052, #26328, .T. ) ;
#5790 = CARTESIAN_POINT ( 'NONE',  ( -58.26905989232412253, -2.944486372867088697, 1.699999999999781686 ) ) ;
#5789 = TOROIDAL_SURFACE ( 'NONE', #3747, 4.284222560975607053, 0.1000000000000000056 ) ;
#5791 = CARTESIAN_POINT ( 'NONE',  ( 47.12349245989109647, -3.859221392886552859, 1.645001822843298545 ) ) ;
#5792 = CARTESIAN_POINT ( 'NONE',  ( 47.00000000000000711, -3.637377585518695611, -2.099877210783200887 ) ) ;
#5793 = DIRECTION ( 'NONE',  ( 0.000000000000000000, -1.000000000000000000, -2.603302919143007729E-15 ) ) ;
#5794 = DIRECTION ( 'NONE',  ( 0.000000000000000000, -0.1576190026614809614, 0.9875000000000001554 ) ) ;
#5796 = CARTESIAN_POINT ( 'NONE',  ( 51.41814105943718971, -4.256263374916419373, 1.450017276182312465 ) ) ;
#5795 = CARTESIAN_POINT ( 'NONE',  ( -59.47025482456093926, 3.201828568350844062, 1.352206208478290872 ) ) ;
#5797 = AXIS2_PLACEMENT_3D ( 'NONE', #31018, #14384, #4109 ) ;
#5798 = EDGE_CURVE ( 'NONE', #8746, #596, #3920, .T. ) ;
#5799 = FACE_OUTER_BOUND ( 'NONE', #6066, .T. ) ;
#5800 = DIRECTION ( 'NONE',  ( 0.5633368246415176861, -0.8262273428075422865, 0.000000000000000000 ) ) ;
#5801 = CARTESIAN_POINT ( 'NONE',  ( 51.17290532404553716, -0.9646187004837835088, 1.462925393634369353 ) ) ;
#5802 = ORIENTED_EDGE ( 'NONE', *, *, #29021, .T. ) ;
#5803 = CIRCLE ( 'NONE', #6297, 2.100000000000000089 ) ;
#5804 = VECTOR ( 'NONE', #26833, 1000.000000000000000 ) ;
#5805 = CARTESIAN_POINT ( 'NONE',  ( 51.36283714269054457, -1.001673184507024805, -1.284520656909109659 ) ) ;
#5806 = CARTESIAN_POINT ( 'NONE',  ( 54.40536566420629327, 5.987876313947340989, -1.625000000000180744 ) ) ;
#5807 = ORIENTED_EDGE ( 'NONE', *, *, #29744, .T. ) ;
#5808 = FACE_OUTER_BOUND ( 'NONE', #5697, .T. ) ;
#5809 = ORIENTED_EDGE ( 'NONE', *, *, #13059, .T. ) ;
#5810 = CARTESIAN_POINT ( 'NONE',  ( 51.59739104186229497, -1.010292945602101256, 1.272765950230260623 ) ) ;
#5811 = VECTOR ( 'NONE', #18645, 1000.000000000000000 ) ;
#5812 = DIRECTION ( 'NONE',  ( 0.000000000000000000, -0.000000000000000000, -1.000000000000000000 ) ) ;
#5814 = DIRECTION ( 'NONE',  ( 1.000000000000000000, -1.219044193948983948E-29, 3.491481338843133355E-15 ) ) ;
#5813 = FACE_OUTER_BOUND ( 'NONE', #19036, .T. ) ;
#5815 = EDGE_LOOP ( 'NONE', ( #28935, #24975, #22465, #19658 ) ) ;
#5816 = CARTESIAN_POINT ( 'NONE',  ( -57.70655989232413674, 1.962990915244717582, 3.399999999999804512 ) ) ;
#5817 = CARTESIAN_POINT ( 'NONE',  ( -62.09999999999997300, 2.749147127886321318, 0.06848408015298343421 ) ) ;
#5818 = VERTEX_POINT ( 'NONE', #9952 ) ;
#5820 = FACE_OUTER_BOUND ( 'NONE', #1144, .T. ) ;
#5819 = CARTESIAN_POINT ( 'NONE',  ( -58.14405989232411542, -2.944486372867072266, -1.700000000000223777 ) ) ;
#5821 = AXIS2_PLACEMENT_3D ( 'NONE', #517, #10173, #15084 ) ;
#5822 = EDGE_LOOP ( 'NONE', ( #25678, #16377 ) ) ;
#5823 = ORIENTED_EDGE ( 'NONE', *, *, #21949, .T. ) ;
#5824 = CARTESIAN_POINT ( 'NONE',  ( -61.18749999999996447, 3.238593381231845036, 2.874284765127022023 ) ) ;
#5825 = DIRECTION ( 'NONE',  ( 0.000000000000000000, 8.881784197001054122E-16, 1.000000000000000000 ) ) ;
#5826 = EDGE_CURVE ( 'NONE', #14710, #1490, #12172, .T. ) ;
#5827 = CARTESIAN_POINT ( 'NONE',  ( 58.74999999305995146, 1.657788420845899724, -0.9867593359914171858 ) ) ;
#5828 = EDGE_CURVE ( 'NONE', #12135, #20165, #22653, .T. ) ;
#5829 = CARTESIAN_POINT ( 'NONE',  ( -36.81959771849335539, -3.629052419422241993, 4.014440194077206314 ) ) ;
#5830 = DIRECTION ( 'NONE',  ( 1.000000000000000000, 0.000000000000000000, 0.000000000000000000 ) ) ;
#5831 = CARTESIAN_POINT ( 'NONE',  ( -55.57202994616207548, 2.078460969082646770, 3.599999999999810019 ) ) ;
#5832 = ORIENTED_EDGE ( 'NONE', *, *, #9863, .F. ) ;
#5833 = AXIS2_PLACEMENT_3D ( 'NONE', #25351, #25023, #15703 ) ;
#5834 = CARTESIAN_POINT ( 'NONE',  ( 15.48686146417447951, -2.966783028120464127, 4.272059443775220622 ) ) ;
#5835 = ORIENTED_EDGE ( 'NONE', *, *, #9587, .T. ) ;
#5836 = AXIS2_PLACEMENT_3D ( 'NONE', #30795, #9106, #18774 ) ;
#5837 = DIRECTION ( 'NONE',  ( 1.000000000000000000, 0.000000000000000000, 0.000000000000000000 ) ) ;
#5838 = EDGE_CURVE ( 'NONE', #8004, #6093, #14107, .T. ) ;
#5839 = CARTESIAN_POINT ( 'NONE',  ( 53.78583212225908738, 7.269814517959708233, -1.827186616692397791 ) ) ;
#5840 = CARTESIAN_POINT ( 'NONE',  ( -56.94702994616206126, -2.078460969082670751, 3.599999999999782041 ) ) ;
#5841 = CARTESIAN_POINT ( 'NONE',  ( 58.74999981196287280, -1.953821646384657384, -0.08499607038929953007 ) ) ;
#5842 = DIRECTION ( 'NONE',  ( 0.000000000000000000, 1.000000000000000000, 4.336808689942015369E-15 ) ) ;
#5843 = VERTEX_POINT ( 'NONE', #30025 ) ;
#5844 = DIRECTION ( 'NONE',  ( 0.000000000000000000, -0.9996898646859343485, -0.02490330187381124133 ) ) ;
#5845 = ORIENTED_EDGE ( 'NONE', *, *, #4985, .F. ) ;
#5846 = DIRECTION ( 'NONE',  ( 2.614375865348240525E-16, -0.2008964009354147762, 0.9796124928211140670 ) ) ;
#5848 = DIRECTION ( 'NONE',  ( -1.000000000000000000, 1.219044193948983948E-29, -3.491481338843133355E-15 ) ) ;
#5847 = DIRECTION ( 'NONE',  ( 0.000000000000000000, -0.9615843008030765526, -0.2745098039215693730 ) ) ;
#5849 = AXIS2_PLACEMENT_3D ( 'NONE', #8976, #6285, #18019 ) ;
#5850 = ORIENTED_EDGE ( 'NONE', *, *, #15111, .T. ) ;
#5851 = VECTOR ( 'NONE', #21513, 1000.000000000000000 ) ;
#5852 = VERTEX_POINT ( 'NONE', #5817 ) ;
#5853 = DIRECTION ( 'NONE',  ( 1.000000000000000000, 0.000000000000000000, 0.000000000000000000 ) ) ;
#5854 = CIRCLE ( 'NONE', #24535, 0.05000000000000012768 ) ;
#5855 = CARTESIAN_POINT ( 'NONE',  ( 48.50000000000002132, -1.391941090707485396, 3.750000000000022649 ) ) ;
#5856 = ORIENTED_EDGE ( 'NONE', *, *, #26317, .F. ) ;
#5858 = DIRECTION ( 'NONE',  ( -3.002035892788116966E-16, 0.9996898646859343485, 0.02490330187381123786 ) ) ;
#5857 = CARTESIAN_POINT ( 'NONE',  ( -59.75952994616203284, -3.117691453623963938, -1.800000000000223199 ) ) ;
#5859 = CARTESIAN_POINT ( 'NONE',  ( -59.17292740578360366, -3.330682475591783653, -0.6830477631804104943 ) ) ;
#5860 = AXIS2_PLACEMENT_3D ( 'NONE', #22291, #575, #12603 ) ;
#5861 = CARTESIAN_POINT ( 'NONE',  ( 60.94140446608462014, 0.5380862305989584371, -1.858165151370887669 ) ) ;
#5862 = DIRECTION ( 'NONE',  ( 0.000000000000000000, 0.000000000000000000, 1.000000000000000000 ) ) ;
#5863 = AXIS2_PLACEMENT_3D ( 'NONE', #8279, #10806, #5754 ) ;
#5864 = ADVANCED_FACE ( 'NONE', ( #13092 ), #10575, .F. ) ;
#5865 = CARTESIAN_POINT ( 'NONE',  ( 53.12796055743056911, 4.814990154991031446, -1.597383859324410516 ) ) ;
#5866 =( LENGTH_UNIT ( ) NAMED_UNIT ( * ) SI_UNIT ( .MILLI., .METRE. ) );
#5867 = TOROIDAL_SURFACE ( 'NONE', #2317, 0.2000000000000000111, 0.1000000000000000056 ) ;
#5868 = EDGE_LOOP ( 'NONE', ( #5181, #13164, #28939, #735, #7233, #19154 ) ) ;
#5869 = AXIS2_PLACEMENT_3D ( 'NONE', #21369, #27987, #11361 ) ;
#5870 = CARTESIAN_POINT ( 'NONE',  ( 47.01551613116910744, -4.158727452193214269, -1.045216533296355887 ) ) ;
#5871 = CARTESIAN_POINT ( 'NONE',  ( 53.53640187423192032, 5.215699251213354870, -1.635615235160539749 ) ) ;
#5872 = CARTESIAN_POINT ( 'NONE',  ( 48.38950019258942348, -0.7811435014052807713, -4.027217152859519089 ) ) ;
#5873 = DIRECTION ( 'NONE',  ( 1.000000000000000000, 3.054025858079668409E-16, -2.042474015755241579E-16 ) ) ;
#5874 = AXIS2_PLACEMENT_3D ( 'NONE', #12829, #17613, #10312 ) ;
#5875 = VECTOR ( 'NONE', #6536, 1000.000000000000000 ) ;
#5876 = DIRECTION ( 'NONE',  ( 3.491481338843133750E-15, 0.000000000000000000, 1.000000000000000000 ) ) ;
#5877 = EDGE_CURVE ( 'NONE', #6272, #23465, #26694, .T. ) ;
#5879 = CARTESIAN_POINT ( 'NONE',  ( 56.95000000000001705, 0.000000000000000000, 0.000000000000000000 ) ) ;
#5878 = CARTESIAN_POINT ( 'NONE',  ( -61.34999999999997300, -2.600201727571727517, 0.4583662226975599441 ) ) ;
#5880 = CIRCLE ( 'NONE', #9442, 0.2500000000000000000 ) ;
#5881 = DIRECTION ( 'NONE',  ( 0.000000000000000000, 0.000000000000000000, 1.000000000000000000 ) ) ;
#5882 = DIRECTION ( 'NONE',  ( -3.002035892788117459E-16, 0.9996898646859344595, 0.02490330187381124133 ) ) ;
#5883 = VECTOR ( 'NONE', #1860, 1000.000000000000000 ) ;
#5885 = CARTESIAN_POINT ( 'NONE',  ( -54.49999999999998579, 3.656246181855014932, -0.5009446076302894735 ) ) ;
#5884 = CARTESIAN_POINT ( 'NONE',  ( 69.25000000000000000, -0.7500000000000000000, -2.288246715074081283 ) ) ;
#5886 = VERTEX_POINT ( 'NONE', #8341 ) ;
#5887 = AXIS2_PLACEMENT_3D ( 'NONE', #9567, #11445, #4629 ) ;
#5888 = AXIS2_PLACEMENT_3D ( 'NONE', #9402, #6703, #14297 ) ;
#5889 =( BOUNDED_SURFACE ( )  B_SPLINE_SURFACE ( 3, 2, ( 
 ( #28453, #13859, #28921 ),
 ( #25916, #23719, #2489 ),
 ( #16896, #21822, #28774 ),
 ( #18965, #26391, #4219 ) ),
 .UNSPECIFIED., .F., .F., .F. ) 
 B_SPLINE_SURFACE_WITH_KNOTS ( ( 4, 4 ),
 ( 3, 3 ),
 ( 7.500129584393919939E-05, 0.0002378367988924469107 ),
 ( 0.000000000000000000, 1.000000000000000000 ),
 .UNSPECIFIED. ) 
 GEOMETRIC_REPRESENTATION_ITEM ( )  RATIONAL_B_SPLINE_SURFACE ( (
 ( 1.000000000000000000, 0.7071067811864996111, 1.000000000000000000),
 ( 1.000000000000000000, 0.7717803178830575650, 1.000000000000000000),
 ( 1.000000000000000000, 0.8407248428044677979, 1.000000000000000000),
 ( 1.000000000000000000, 0.8397191227596303431, 1.000000000000000000) ) ) 
 REPRESENTATION_ITEM ( '' )  SURFACE ( )  );
#5890 = DIRECTION ( 'NONE',  ( 1.000000000000000000, -1.219044193948983948E-29, 3.491481338843133355E-15 ) ) ;
#5892 = DIRECTION ( 'NONE',  ( -1.000000000000000000, -0.000000000000000000, 3.491481338843133355E-15 ) ) ;
#5891 = CARTESIAN_POINT ( 'NONE',  ( 16.07279755198654314, 3.436881753486524360, -4.177093996075191384 ) ) ;
#5893 = DIRECTION ( 'NONE',  ( 3.016910393003118404E-15, 0.000000000000000000, 1.000000000000000000 ) ) ;
#5894 = ORIENTED_EDGE ( 'NONE', *, *, #31020, .T. ) ;
#5895 = CARTESIAN_POINT ( 'NONE',  ( 53.05250010753326251, 4.165967808473761025, 2.049999999999814637 ) ) ;
#5896 = CARTESIAN_POINT ( 'NONE',  ( 22.32336313483204648, 6.618105965108087574, -1.550000000000077316 ) ) ;
#5897 = VERTEX_POINT ( 'NONE', #23080 ) ;
#5898 = APPLICATION_CONTEXT ( 'automotive_design' ) ;
#5899 = AXIS2_PLACEMENT_3D ( 'NONE', #28531, #31057, #4620 ) ;
#5900 = CARTESIAN_POINT ( 'NONE',  ( -58.20655989232411542, -3.399999999999991029, -2.246812820714294660E-13 ) ) ;
#5901 = VERTEX_POINT ( 'NONE', #18014 ) ;
#5902 = CARTESIAN_POINT ( 'NONE',  ( -54.54999999999998295, 0.9643027244899942119, -4.702139965541348055 ) ) ;
#5903 = DIRECTION ( 'NONE',  ( -1.000000000000000000, -0.000000000000000000, 1.047444401652940007E-14 ) ) ;
#5904 = VERTEX_POINT ( 'NONE', #25129 ) ;
#5905 =( LENGTH_UNIT ( ) NAMED_UNIT ( * ) SI_UNIT ( .MILLI., .METRE. ) );
#5906 = VECTOR ( 'NONE', #4448, 1000.000000000000000 ) ;
#5907 = CARTESIAN_POINT ( 'NONE',  ( 51.45655683570189609, 0.9591657938401617622, -1.468576096419531352 ) ) ;
#5908 = EDGE_CURVE ( 'NONE', #4682, #30038, #922, .T. ) ;
#5909 = CARTESIAN_POINT ( 'NONE',  ( -60.32202994616201863, 2.078460969082674747, -3.600000000000205258 ) ) ;
#5910 = VERTEX_POINT ( 'NONE', #20558 ) ;
#5911 = CARTESIAN_POINT ( 'NONE',  ( 68.05000000000002558, 1.401298464324817071E-42, -7.127859153248258291E-13 ) ) ;
#5912 = DIRECTION ( 'NONE',  ( 0.000000000000000000, 1.000000000000000000, 4.336808689942015369E-15 ) ) ;
#5913 = AXIS2_PLACEMENT_3D ( 'NONE', #25193, #10775, #20457 ) ;
#5914 = ORIENTED_EDGE ( 'NONE', *, *, #25882, .F. ) ;
#5915 = AXIS2_PLACEMENT_3D ( 'NONE', #11872, #11571, #23767 ) ;
#5916 = CARTESIAN_POINT ( 'NONE',  ( -56.99999999999997158, -2.944486372867089141, 1.699999999999786571 ) ) ;
#5917 = AXIS2_PLACEMENT_3D ( 'NONE', #6225, #18127, #30284 ) ;
#5918 = AXIS2_PLACEMENT_3D ( 'NONE', #20657, #11270, #25694 ) ;
#5919 = CARTESIAN_POINT ( 'NONE',  ( 58.75000000000001421, 0.5933363752225945253, -1.867039175319659572 ) ) ;
#5920 = FACE_OUTER_BOUND ( 'NONE', #20211, .T. ) ;
#5921 = CARTESIAN_POINT ( 'NONE',  ( 56.95766603241608550, -0.7209790597604740503, -1.757928312873409116 ) ) ;
#5922 = DIRECTION ( 'NONE',  ( 1.000000000000000000, -0.000000000000000000, -0.000000000000000000 ) ) ;
#5923 = EDGE_CURVE ( 'NONE', #15962, #2931, #12492, .T. ) ;
#5924 = CARTESIAN_POINT ( 'NONE',  ( -57.15835481156724285, 4.108500314926515351, -1.367561758111408343 ) ) ;
#5925 = AXIS2_PLACEMENT_3D ( 'NONE', #15521, #962, #6318 ) ;
#5926 = AXIS2_PLACEMENT_3D ( 'NONE', #2150, #28911, #28598 ) ;
#5927 = DIRECTION ( 'NONE',  ( 0.000000000000000000, 0.000000000000000000, -1.000000000000000000 ) ) ;
#5928 = CARTESIAN_POINT ( 'NONE',  ( 58.75000000000000000, 2.008165151418861427, -0.5380862305899540843 ) ) ;
#5929 = CARTESIAN_POINT ( 'NONE',  ( -59.69740665358683884, 2.094969456803113861, 1.745644717383348477 ) ) ;
#5930 = CARTESIAN_POINT ( 'NONE',  ( 58.65000045311410304, 1.383426348888211699, -1.265716300431776631 ) ) ;
#5932 = CARTESIAN_POINT ( 'NONE',  ( 52.91430282107062766, 8.434692232659099176, -2.050000000000183231 ) ) ;
#5931 = AXIS2_PLACEMENT_3D ( 'NONE', #5111, #12539, #22369 ) ;
#5933 = ORIENTED_EDGE ( 'NONE', *, *, #399, .F. ) ;
#5934 = CARTESIAN_POINT ( 'NONE',  ( 50.42115343657336268, -0.9200365198983494475, 3.998286360709618403 ) ) ;
#5935 = EDGE_CURVE ( 'NONE', #20739, #23786, #31228, .T. ) ;
#5936 = CYLINDRICAL_SURFACE ( 'NONE', #12921, 1.625000000000000222 ) ;
#5937 = ORIENTED_EDGE ( 'NONE', *, *, #18457, .T. ) ;
#5938 = CIRCLE ( 'NONE', #3431, 2.765000000000001013 ) ;
#5939 = ORIENTED_EDGE ( 'NONE', *, *, #30955, .T. ) ;
#5940 = AXIS2_PLACEMENT_3D ( 'NONE', #30248, #20306, #29935 ) ;
#5941 = TOROIDAL_SURFACE ( 'NONE', #19110, 1.524417381223824197, 0.05000000000000000278 ) ;
#5942 = DIRECTION ( 'NONE',  ( 0.000000000000000000, 0.9996898646859343485, 0.02490330187381123786 ) ) ;
#5943 = CARTESIAN_POINT ( 'NONE',  ( -57.92292740578360366, 1.073804522883521795, 3.225979517392336682 ) ) ;
#5945 = DIRECTION ( 'NONE',  ( 0.000000000000000000, 0.000000000000000000, 1.000000000000000000 ) ) ;
#5944 = CARTESIAN_POINT ( 'NONE',  ( -58.49999999999997868, -2.944486372867089141, 1.699999999999781242 ) ) ;
#5946 = VERTEX_POINT ( 'NONE', #25437 ) ;
#5947 = ORIENTED_EDGE ( 'NONE', *, *, #3718, .F. ) ;
#5948 = CARTESIAN_POINT ( 'NONE',  ( 34.50000000000001421, 0.000000000000000000, 0.000000000000000000 ) ) ;
#5949 = ORIENTED_EDGE ( 'NONE', *, *, #12259, .T. ) ;
#5950 = B_SPLINE_CURVE_WITH_KNOTS ( 'NONE', 3,
 ( #3446, #12764, #25118, #29872 ),
 .UNSPECIFIED., .F., .F.,
 ( 4, 4 ),
 ( 0.000000000000000000, 3.288265101740459116E-05 ),
 .UNSPECIFIED. ) ;
#5951 = CARTESIAN_POINT ( 'NONE',  ( 51.80000000000001137, 3.850000000000016520, -1.678541033159632434 ) ) ;
#5952 = EDGE_CURVE ( 'NONE', #10254, #13776, #11040, .T. ) ;
#5953 = VERTEX_POINT ( 'NONE', #22780 ) ;
#5954 = CARTESIAN_POINT ( 'NONE',  ( 21.97322666366011390, 8.076925076899296840, -1.950000000000075895 ) ) ;
#5955 = EDGE_CURVE ( 'NONE', #18823, #9407, #16568, .T. ) ;
#5956 = DIRECTION ( 'NONE',  ( 1.000000000000000000, 1.047444401652940007E-14, 0.000000000000000000 ) ) ;
#5957 = CIRCLE ( 'NONE', #6445, 0.04999999999999989175 ) ;
#5958 = EDGE_CURVE ( 'NONE', #25169, #468, #23140, .T. ) ;
#5959 = CARTESIAN_POINT ( 'NONE',  ( 54.31409749668479492, 6.709390224138187975, 2.049999999999810640 ) ) ;
#5960 = AXIS2_PLACEMENT_3D ( 'NONE', #17340, #17664, #22410 ) ;
#5961 = AXIS2_PLACEMENT_3D ( 'NONE', #8989, #12001, #31305 ) ;
#5962 = CARTESIAN_POINT ( 'NONE',  ( -74.39999999999997726, -2.588216748940040213E-15, 4.710014593512140639E-15 ) ) ;
#5963 = CARTESIAN_POINT ( 'NONE',  ( -59.08155989232413674, -1.962990915244731571, 3.399999999999781419 ) ) ;
#5964 = CARTESIAN_POINT ( 'NONE',  ( 52.45567523936535537, 8.517307475678972395, -1.943109374214847973 ) ) ;
#5965 = CARTESIAN_POINT ( 'NONE',  ( 58.73371041428917039, 1.267950628961455939, 1.381461519774026536 ) ) ;
#5966 = AXIS2_PLACEMENT_3D ( 'NONE', #21961, #249, #9913 ) ;
#5967 = CARTESIAN_POINT ( 'NONE',  ( 48.49162684147595570, 1.391941090707552897, 3.850000000000020517 ) ) ;
#5968 = DIRECTION ( 'NONE',  ( 1.387778780781445676E-14, -1.000000000000000000, 0.000000000000000000 ) ) ;
#5970 = FACE_OUTER_BOUND ( 'NONE', #26813, .T. ) ;
#5969 = CARTESIAN_POINT ( 'NONE',  ( -60.61250724947092294, -2.505441611314725314, 1.006360935396775069 ) ) ;
#5971 = DIRECTION ( 'NONE',  ( 1.000000000000000000, 3.054025858079668409E-16, -2.042474015755241579E-16 ) ) ;
#5972 = DIRECTION ( 'NONE',  ( 1.000000000000000000, 1.047444401652940007E-14, -0.000000000000000000 ) ) ;
#5973 = DIRECTION ( 'NONE',  ( -1.000000000000000000, 9.912705577004238501E-16, 3.469446951951483476E-15 ) ) ;
#5974 = ORIENTED_EDGE ( 'NONE', *, *, #21270, .T. ) ;
#5975 = AXIS2_PLACEMENT_3D ( 'NONE', #18425, #6228, #8599 ) ;
#5976 = EDGE_CURVE ( 'NONE', #9170, #2253, #12771, .T. ) ;
#5977 = AXIS2_PLACEMENT_3D ( 'NONE', #26353, #18923, #4656 ) ;
#5978 = FACE_OUTER_BOUND ( 'NONE', #12545, .T. ) ;
#5979 = CARTESIAN_POINT ( 'NONE',  ( 54.31535817511873176, 6.000144074150753681, 2.049999999999810196 ) ) ;
#5980 = ORIENTED_EDGE ( 'NONE', *, *, #15195, .F. ) ;
#5981 = CARTESIAN_POINT ( 'NONE',  ( -59.37009172985672478, 3.234433134214944605, -1.048065980887175730 ) ) ;
#5982 = CIRCLE ( 'NONE', #26124, 4.384222560975607585 ) ;
#5983 = EDGE_LOOP ( 'NONE', ( #2229, #9730, #15226, #28249 ) ) ;
#5984 = EDGE_CURVE ( 'NONE', #585, #779, #15314, .T. ) ;
#5985 = CARTESIAN_POINT ( 'NONE',  ( 15.03925126672132961, -0.4576450603546909357, -5.200000000000000178 ) ) ;
#5986 = CARTESIAN_POINT ( 'NONE',  ( -54.72085481156724285, 1.184343223768591580, 3.558065644182726750 ) ) ;
#5988 = CARTESIAN_POINT ( 'NONE',  ( 51.31572262954149721, 1.002608958138273554, 1.395204572094392192 ) ) ;
#5987 = CARTESIAN_POINT ( 'NONE',  ( 61.02708519082507621, -0.5631634571404888767, 1.705199831323249038 ) ) ;
#5989 = ORIENTED_EDGE ( 'NONE', *, *, #4693, .T. ) ;
#5990 = FACE_OUTER_BOUND ( 'NONE', #1966, .T. ) ;
#5991 = DIRECTION ( 'NONE',  ( -1.000000000000000000, 1.219044193948983948E-29, -3.491481338843133355E-15 ) ) ;
#5992 = VERTEX_POINT ( 'NONE', #12929 ) ;
#5994 = DIRECTION ( 'NONE',  ( 0.000000000000000000, 1.000000000000000000, 0.000000000000000000 ) ) ;
#5993 = DIRECTION ( 'NONE',  ( -9.654113257610060303E-15, 0.000000000000000000, -1.000000000000000000 ) ) ;
#5995 = PLANE ( 'NONE',  #17992 ) ;
#5996 = ORIENTED_EDGE ( 'NONE', *, *, #18752, .F. ) ;
#5997 = CARTESIAN_POINT ( 'NONE',  ( -36.04581030752768100, 5.340403874104499238, -0.9205822090004349700 ) ) ;
#5998 = EDGE_CURVE ( 'NONE', #4089, #24848, #2410, .T. ) ;
#5999 = CARTESIAN_POINT ( 'NONE',  ( 58.75000000000000711, 1.760622601996782777, 0.8948927608044729975 ) ) ;
#6000 = DIRECTION ( 'NONE',  ( 1.000000000000000000, 1.047444401652940007E-14, 0.000000000000000000 ) ) ;
#6001 = DIRECTION ( 'NONE',  ( 0.000000000000000000, -1.000000000000000000, -3.491481338843132961E-15 ) ) ;
#6002 = AXIS2_PLACEMENT_3D ( 'NONE', #620, #10280, #29294 ) ;
#6003 = ORIENTED_EDGE ( 'NONE', *, *, #16141, .F. ) ;
#6004 = AXIS2_PLACEMENT_3D ( 'NONE', #21933, #27119, #10042 ) ;
#6005 = CARTESIAN_POINT ( 'NONE',  ( 15.76675455518197211, 3.261791109367046637, 4.314133646218528462 ) ) ;
#6006 = CARTESIAN_POINT ( 'NONE',  ( -60.64918514029854180, -2.511238585898485365, 0.9917933002572968393 ) ) ;
#6007 = LINE ( 'NONE', #27513, #16985 ) ;
#6008 = ADVANCED_FACE ( 'NONE', ( #30655 ), #6458, .F. ) ;
#6009 = CARTESIAN_POINT ( 'NONE',  ( -58.38452994616204705, -3.117691453623983033, 1.799999999999769784 ) ) ;
#6010 = B_SPLINE_CURVE_WITH_KNOTS ( 'NONE', 3,
 ( #21688, #12876, #29672, #695 ),
 .UNSPECIFIED., .F., .F.,
 ( 4, 4 ),
 ( 0.000000000000000000, 0.0001494103359351912257 ),
 .UNSPECIFIED. ) ;
#6011 = CARTESIAN_POINT ( 'NONE',  ( 58.65000038048068376, -1.873220289782048686, 0.08335421200007571418 ) ) ;
#6012 = FACE_OUTER_BOUND ( 'NONE', #25519, .T. ) ;
#6013 = EDGE_CURVE ( 'NONE', #704, #10186, #11819, .T. ) ;
#6014 = ORIENTED_EDGE ( 'NONE', *, *, #19790, .T. ) ;
#6015 = CARTESIAN_POINT ( 'NONE',  ( -67.99999999999997158, -0.3264566515200493790, 1.591870300834312690 ) ) ;
#6016 = ORIENTED_EDGE ( 'NONE', *, *, #602, .F. ) ;
#6017 = UNCERTAINTY_MEASURE_WITH_UNIT (LENGTH_MEASURE( 1.000000000000000082E-05 ), #6831, 'distance_accuracy_value', 'NONE');
#6018 = EDGE_CURVE ( 'NONE', #12847, #26028, #18331, .T. ) ;
#6019 = CARTESIAN_POINT ( 'NONE',  ( -59.15159661603878050, 2.488695505467597879, -0.9494100618347165454 ) ) ;
#6021 = CARTESIAN_POINT ( 'NONE',  ( 47.00000000000002132, -3.726179070414207928, -1.000000000000002220 ) ) ;
#6020 = FACE_OUTER_BOUND ( 'NONE', #11820, .T. ) ;
#6022 = VERTEX_POINT ( 'NONE', #18647 ) ;
#6023 = EDGE_LOOP ( 'NONE', ( #3988, #12062, #15679, #11566, #29583, #12414, #7163, #22036 ) ) ;
#6024 = CARTESIAN_POINT ( 'NONE',  ( -58.99005354137801049, -3.399999999999994138, 0.9110272542655820649 ) ) ;
#6025 =( GEOMETRIC_REPRESENTATION_CONTEXT ( 3 ) GLOBAL_UNCERTAINTY_ASSIGNED_CONTEXT ( ( #22182 ) ) GLOBAL_UNIT_ASSIGNED_CONTEXT ( ( #19816, #24401, #28997 ) ) REPRESENTATION_CONTEXT ( 'NONE', 'WORKASPACE' ) );
#6026 = CIRCLE ( 'NONE', #13584, 1.975000000000001865 ) ;
#6027 = FACE_BOUND ( 'NONE', #23999, .T. ) ;
#6028 = ORIENTED_EDGE ( 'NONE', *, *, #19116, .F. ) ;
#6030 = CARTESIAN_POINT ( 'NONE',  ( -55.74986116251336199, 1.737685414808520790, -3.471684241605567323 ) ) ;
#6029 = CARTESIAN_POINT ( 'NONE',  ( -60.69702994616205416, -2.078460969082657872, 3.599999999999776712 ) ) ;
#6031 = CARTESIAN_POINT ( 'NONE',  ( -59.48542740578359656, 2.936324665650206445, 2.606018187048499524 ) ) ;
#6032 = CARTESIAN_POINT ( 'NONE',  ( 36.50000000000002132, 0.000000000000000000, -1.899999999999999911 ) ) ;
#6033 = PRODUCT_CONTEXT ( 'NONE', #22700, 'mechanical' ) ;
#6034 = CARTESIAN_POINT ( 'NONE',  ( 52.04555679422406200, 4.350000000000022737, -1.551140652419768617 ) ) ;
#6035 = VECTOR ( 'NONE', #4348, 1000.000000000000000 ) ;
#6036 = VERTEX_POINT ( 'NONE', #23541 ) ;
#6037 = CARTESIAN_POINT ( 'NONE',  ( -61.00952994616203284, 3.117691453623994580, -1.800000000000202993 ) ) ;
#6038 = CARTESIAN_POINT ( 'NONE',  ( 53.71202192472756565, 7.447163568589272309, -1.837855077339860976 ) ) ;
#6039 = LINE ( 'NONE', #18699, #6071 ) ;
#6040 = PRODUCT_DEFINITION ( 'UNKNOWN', '', #15160, #313 ) ;
#6041 = CARTESIAN_POINT ( 'NONE',  ( 15.56401610563845850, 1.027070083876111761, 5.312835761376648591 ) ) ;
#6042 = CARTESIAN_POINT ( 'NONE',  ( -71.44999999999998863, -1.380331489585512972E-15, 2.906968604901091669E-15 ) ) ;
#6043 = CIRCLE ( 'NONE', #30298, 4.099999999999992539 ) ;
#6045 = CARTESIAN_POINT ( 'NONE',  ( 58.64999999999992042, -1.077297519403624060, -1.655311165517087568 ) ) ;
#6044 = CARTESIAN_POINT ( 'NONE',  ( 22.58314801556725371, 7.622751244490530986, -1.425000000000078870 ) ) ;
#6046 = DIRECTION ( 'NONE',  ( 0.000000000000000000, 0.000000000000000000, 1.000000000000000000 ) ) ;
#6047 = CARTESIAN_POINT ( 'NONE',  ( -60.49999999999995737, 1.963826825011730345E-15, 6.704595576490977020E-16 ) ) ;
#6049 = DIRECTION ( 'NONE',  ( 1.003947306782822575E-14, 0.000000000000000000, 1.000000000000000000 ) ) ;
#6048 = CARTESIAN_POINT ( 'NONE',  ( -59.37499999999997868, -2.099645193746120606E-14, 3.399999999999788525 ) ) ;
#6050 = EDGE_CURVE ( 'NONE', #23458, #10001, #30701, .T. ) ;
#6051 = ORIENTED_EDGE ( 'NONE', *, *, #11746, .F. ) ;
#6052 = CARTESIAN_POINT ( 'NONE',  ( 50.42159256128543632, -1.310166284604358244, -3.885185101012172737 ) ) ;
#6053 = DIRECTION ( 'NONE',  ( 0.000000000000000000, -1.000000000000000000, -3.491481338843137694E-15 ) ) ;
#6055 = CARTESIAN_POINT ( 'NONE',  ( 68.95000000000003126, 1.401298464324817071E-42, -7.222129149397022450E-13 ) ) ;
#6054 = CARTESIAN_POINT ( 'NONE',  ( -77.28999999999996362, -3.470778894058966809E-15, 5.300300110251643219E-15 ) ) ;
#6056 = CARTESIAN_POINT ( 'NONE',  ( 56.99370871690835116, 0.8156862421929632623, 2.468735699563065378 ) ) ;
#6057 = ORIENTED_EDGE ( 'NONE', *, *, #6217, .F. ) ;
#6058 = CARTESIAN_POINT ( 'NONE',  ( 53.05417955289647125, 8.376364939874980209, 2.049999999999815081 ) ) ;
#6059 = CARTESIAN_POINT ( 'NONE',  ( -60.64877780295373100, -2.458847256512897150, -1.115342769719651850 ) ) ;
#6060 = AXIS2_PLACEMENT_3D ( 'NONE', #21305, #14299, #5547 ) ;
#6061 = ORIENTED_EDGE ( 'NONE', *, *, #2115, .T. ) ;
#6062 = FACE_OUTER_BOUND ( 'NONE', #18360, .T. ) ;
#6063 = VERTEX_POINT ( 'NONE', #6449 ) ;
#6064 = CYLINDRICAL_SURFACE ( 'NONE', #26918, 4.100000000000022737 ) ;
#6065 = CARTESIAN_POINT ( 'NONE',  ( -59.19999999999997442, 8.366749974758448157E-15, -2.103076948839454410E-13 ) ) ;
#6066 = EDGE_LOOP ( 'NONE', ( #10024, #28475, #28377, #9109 ) ) ;
#6067 = CARTESIAN_POINT ( 'NONE',  ( -55.82202994616203995, 2.078460969082679188, -3.600000000000186606 ) ) ;
#6068 = AXIS2_PLACEMENT_3D ( 'NONE', #3482, #18055, #25321 ) ;
#6069 = ADVANCED_FACE ( 'NONE', ( #16262 ), #25590, .T. ) ;
#6070 = CARTESIAN_POINT ( 'NONE',  ( -56.26905989232412963, 2.944486372867092250, 1.699999999999811218 ) ) ;
#6071 = VECTOR ( 'NONE', #23137, 1000.000000000000000 ) ;
#6072 = ORIENTED_EDGE ( 'NONE', *, *, #4390, .T. ) ;
#6073 = ORIENTED_EDGE ( 'NONE', *, *, #17877, .T. ) ;
#6074 = VECTOR ( 'NONE', #31087, 1000.000000000000000 ) ;
#6075 = CARTESIAN_POINT ( 'NONE',  ( -56.49999999999997868, 2.944486372867092250, 1.699999999999810774 ) ) ;
#6076 = CARTESIAN_POINT ( 'NONE',  ( 60.89136863770590224, 0.5000000000006363798, 1.718465794862841678 ) ) ;
#6077 = CARTESIAN_POINT ( 'NONE',  ( 58.65000000000003411, -1.655311165516606398, -1.077297519404007309 ) ) ;
#6078 = CARTESIAN_POINT ( 'NONE',  ( 56.98297952491088836, -0.7550874052942159187, -1.743526814789472912 ) ) ;
#6079 = CARTESIAN_POINT ( 'NONE',  ( -59.59999999999998721, -2.157671697750204842, 1.538490443495526216 ) ) ;
#6081 = CARTESIAN_POINT ( 'NONE',  ( -57.22499999999997300, 0.9241234443029104906, -4.506217466977124886 ) ) ;
#6080 = DIRECTION ( 'NONE',  ( 1.000000000000000000, 1.047444401652940007E-14, 0.000000000000000000 ) ) ;
#6082 = CARTESIAN_POINT ( 'NONE',  ( -57.22499999999997300, 2.964020293532818446E-15, 1.549317489258312010E-18 ) ) ;
#6083 = CARTESIAN_POINT ( 'NONE',  ( 51.80000000000001847, 6.982261990806648555E-14, -1.796574372350448449E-13 ) ) ;
#6084 = EDGE_CURVE ( 'NONE', #20395, #2624, #7450, .T. ) ;
#6085 = CARTESIAN_POINT ( 'NONE',  ( 58.66122797211835405, -1.615588400946606162, -0.9517229765811223707 ) ) ;
#6086 = CARTESIAN_POINT ( 'NONE',  ( 48.39188949082539892, -1.340787288841403635, 3.874691554877328858 ) ) ;
#6087 = EDGE_LOOP ( 'NONE', ( #29477, #28123, #19386, #9693, #9286, #3281, #14063 ) ) ;
#6088 = ADVANCED_FACE ( 'NONE', ( #30823 ), #14544, .T. ) ;
#6089 = CARTESIAN_POINT ( 'NONE',  ( -59.92928932188130631, -0.9643027244899888828, 4.702139965541348055 ) ) ;
#6090 = CARTESIAN_POINT ( 'NONE',  ( -36.92398358572908279, 0.2875137064281962362, -5.407399902318745788 ) ) ;
#6091 = CIRCLE ( 'NONE', #17719, 0.05000000000000009298 ) ;
#6092 = EDGE_LOOP ( 'NONE', ( #4685, #7677, #7826, #8956, #27920, #26381 ) ) ;
#6093 = VERTEX_POINT ( 'NONE', #18486 ) ;
#6094 = CARTESIAN_POINT ( 'NONE',  ( 58.75000000000002132, 6.153735859711025284E-13, 3.111507638930570854E-58 ) ) ;
#6095 = CARTESIAN_POINT ( 'NONE',  ( 64.99999999999998579, 4.286263797015736595E-16, -3.500000000000680789 ) ) ;
#6097 = CARTESIAN_POINT ( 'NONE',  ( -59.39297944956340558, 2.353586303871975982, 1.218361332808637121 ) ) ;
#6096 = CARTESIAN_POINT ( 'NONE',  ( -57.43749999999996447, 1.962990915244749557, -3.400000000000195310 ) ) ;
#6098 = ORIENTED_EDGE ( 'NONE', *, *, #16848, .F. ) ;
#6099 = VERTEX_POINT ( 'NONE', #26066 ) ;
#6100 = DIRECTION ( 'NONE',  ( 0.000000000000000000, 0.000000000000000000, -1.000000000000000000 ) ) ;
#6101 = ORIENTED_EDGE ( 'NONE', *, *, #15418, .T. ) ;
#6102 = DIRECTION ( 'NONE',  ( 6.600692696441737066E-15, -0.6683962987610915230, -0.7438053426821252812 ) ) ;
#6103 = EDGE_CURVE ( 'NONE', #7506, #4534, #15536, .T. ) ;
#6104 = ORIENTED_EDGE ( 'NONE', *, *, #29326, .F. ) ;
#6105 = CARTESIAN_POINT ( 'NONE',  ( 25.68808851946277727, 5.234409800456325534, -2.050000000000087752 ) ) ;
#6106 = LINE ( 'NONE', #6252, #11653 ) ;
#6107 = DIRECTION ( 'NONE',  ( 0.000000000000000000, 0.000000000000000000, 1.000000000000000000 ) ) ;
#6108 = VERTEX_POINT ( 'NONE', #4065 ) ;
#6109 = CARTESIAN_POINT ( 'NONE',  ( -58.43749999999997158, 0.7533615035078148336, -3.673546848079175309 ) ) ;
#6110 = CARTESIAN_POINT ( 'NONE',  ( 15.03925126672132961, -1.123735532908273216, 5.289358697221548944 ) ) ;
#6111 = CARTESIAN_POINT ( 'NONE',  ( -59.14405989232412963, -3.920666489018302546E-15, 3.399999999999788969 ) ) ;
#6112 = EDGE_CURVE ( 'NONE', #13558, #28004, #5938, .T. ) ;
#6113 = CARTESIAN_POINT ( 'NONE',  ( 47.73505020348671479, -4.023708852620726972, 1.198807875231203468 ) ) ;
#6114 = CARTESIAN_POINT ( 'NONE',  ( 58.72204580543407815, 1.341784641882211693, 1.309860786662967680 ) ) ;
#6115 = AXIS2_PLACEMENT_3D ( 'NONE', #8273, #17940, #23285 ) ;
#6116 = DIRECTION ( 'NONE',  ( 1.000000000000000000, -1.219044193948983948E-29, 3.491481338843133355E-15 ) ) ;
#6117 = CARTESIAN_POINT ( 'NONE',  ( 58.75000000000000711, 1.039502773797213120, -1.650471618823823539 ) ) ;
#6119 = CARTESIAN_POINT ( 'NONE',  ( 50.80000000000002558, -4.387164041431065087, 1.383037119376580248 ) ) ;
#6118 = CARTESIAN_POINT ( 'NONE',  ( 47.04142135623732912, -3.767600426651517065, 1.000000000000000222 ) ) ;
#6120 = CARTESIAN_POINT ( 'NONE',  ( -58.78335481156722864, 0.7533615035077975142, -3.673546848079180638 ) ) ;
#6121 = EDGE_CURVE ( 'NONE', #8161, #1297, #19626, .T. ) ;
#6122 = CARTESIAN_POINT ( 'NONE',  ( 47.06312566212017146, 8.366466760780054912, 2.049999999999835953 ) ) ;
#6123 = ADVANCED_FACE ( 'NONE', ( #2004 ), #30725, .T. ) ;
#6124 = ORIENTED_EDGE ( 'NONE', *, *, #21538, .T. ) ;
#6125 = EDGE_CURVE ( 'NONE', #17201, #5886, #9294, .T. ) ;
#6126 = CARTESIAN_POINT ( 'NONE',  ( 54.26434950415730896, 6.004763229855418771, -2.050000000000188560 ) ) ;
#6127 = VERTEX_POINT ( 'NONE', #26231 ) ;
#6128 = DIRECTION ( 'NONE',  ( 0.000000000000000000, 0.000000000000000000, 1.000000000000000000 ) ) ;
#6129 = EDGE_LOOP ( 'NONE', ( #18712, #16849, #22487, #4758 ) ) ;
#6130 = CARTESIAN_POINT ( 'NONE',  ( 15.17256654081424472, -0.4576450652446781842, -5.200000002521312226 ) ) ;
#6131 = CARTESIAN_POINT ( 'NONE',  ( -56.22085481156723574, 1.184343223768591358, 3.558065644182726750 ) ) ;
#6133 = CARTESIAN_POINT ( 'NONE',  ( -69.22071067811863543, -6.995007661688606141E-16, 2.451642053546763754E-15 ) ) ;
#6132 = CARTESIAN_POINT ( 'NONE',  ( 51.25000000000001421, 1.100000000000537215, 1.196087371390568643 ) ) ;
#6134 = ORIENTED_EDGE ( 'NONE', *, *, #11950, .T. ) ;
#6135 = CARTESIAN_POINT ( 'NONE',  ( 33.39238368996267070, 8.222114305082241614, -2.050000000000116618 ) ) ;
#6136 = DIRECTION ( 'NONE',  ( 0.000000000000000000, 0.000000000000000000, 1.000000000000000000 ) ) ;
#6137 = EDGE_CURVE ( 'NONE', #22178, #12162, #16597, .T. ) ;
#6138 = VERTEX_POINT ( 'NONE', #20864 ) ;
#6140 = DIRECTION ( 'NONE',  ( 1.000000000000000000, 2.586136946169074517E-16, -0.000000000000000000 ) ) ;
#6139 = CARTESIAN_POINT ( 'NONE',  ( 50.29999999999740368, 1.409901620923733390, 3.849999999997240518 ) ) ;
#6141 = CARTESIAN_POINT ( 'NONE',  ( -55.99005354137803181, -3.399999999999995026, 0.9110272542656013828 ) ) ;
#6142 = ORIENTED_EDGE ( 'NONE', *, *, #27708, .F. ) ;
#6143 = CARTESIAN_POINT ( 'NONE',  ( -36.48821680285229263, 5.256402525810011994, -1.287848407636733139 ) ) ;
#6144 = FACE_OUTER_BOUND ( 'NONE', #555, .T. ) ;
#6145 = DIRECTION ( 'NONE',  ( -3.491481338843133355E-15, 0.000000000000000000, -1.000000000000000000 ) ) ;
#6146 = DIRECTION ( 'NONE',  ( 0.000000000000000000, -8.881784197000848032E-16, 1.000000000000000000 ) ) ;
#6147 = CARTESIAN_POINT ( 'NONE',  ( 52.20711756518984714, -0.6499999999994510169, 1.489337100860649077 ) ) ;
#6148 = EDGE_CURVE ( 'NONE', #27932, #21024, #397, .T. ) ;
#6149 = ORIENTED_EDGE ( 'NONE', *, *, #20855, .F. ) ;
#6150 = AXIS2_PLACEMENT_3D ( 'NONE', #11215, #20888, #30517 ) ;
#6151 = CIRCLE ( 'NONE', #23852, 0.7500000000000186517 ) ;
#6152 = EDGE_CURVE ( 'NONE', #26216, #9570, #2926, .T. ) ;
#6153 = CARTESIAN_POINT ( 'NONE',  ( 33.47623932017462778, -4.374999999999999112, 0.000000000000000000 ) ) ;
#6154 = B_SPLINE_CURVE_WITH_KNOTS ( 'NONE', 3,
 ( #22881, #29507, #5466, #3237, #7821, #10679, #24774, #3083, #17497, #12731, #20363, #27309, #12879 ),
 .UNSPECIFIED., .F., .F.,
 ( 4, 3, 3, 3, 4 ),
 ( 0.000000000000000000, 1.691191182548890470E-05, 3.382457420317648886E-05, 5.072228820803683589E-05, 6.090521770676877105E-05 ),
 .UNSPECIFIED. ) ;
#6155 = FACE_OUTER_BOUND ( 'NONE', #6528, .T. ) ;
#6156 = CARTESIAN_POINT ( 'NONE',  ( 51.87987261549070439, -4.254270342444942621, 1.021450466989924477 ) ) ;
#6157 = EDGE_CURVE ( 'NONE', #15867, #10721, #30490, .T. ) ;
#6158 = EDGE_CURVE ( 'NONE', #9761, #29519, #8484, .T. ) ;
#6159 = DIRECTION ( 'NONE',  ( 3.489354422748178582E-15, -1.218509414717996338E-16, 1.000000000000000000 ) ) ;
#6160 = DIRECTION ( 'NONE',  ( 1.000000000000000000, 2.586136946169074517E-16, -0.000000000000000000 ) ) ;
#6161 = CARTESIAN_POINT ( 'NONE',  ( 31.31144479506063760, 7.468183200860340598, 2.049999999999891021 ) ) ;
#6162 = VERTEX_POINT ( 'NONE', #17347 ) ;
#6163 = AXIS2_PLACEMENT_3D ( 'NONE', #27290, #5606, #1609 ) ;
#6164 = CARTESIAN_POINT ( 'NONE',  ( 48.50000000000002132, -4.899999999999999467, -3.950000000000022826 ) ) ;
#6165 = VERTEX_POINT ( 'NONE', #31130 ) ;
#6166 = DIRECTION ( 'NONE',  ( 0.000000000000000000, 0.4295302013422852561, -0.9030524935654935526 ) ) ;
#6168 = DIRECTION ( 'NONE',  ( 0.000000000000000000, 0.8660422822663634834, -0.4999707644721521627 ) ) ;
#6167 = CARTESIAN_POINT ( 'NONE',  ( 58.75000000000000711, 0.8979909453699834732, -1.749377236609715780 ) ) ;
#6169 = ORIENTED_EDGE ( 'NONE', *, *, #26088, .F. ) ;
#6170 = ORIENTED_EDGE ( 'NONE', *, *, #15374, .F. ) ;
#6171 = CARTESIAN_POINT ( 'NONE',  ( 54.40000000000001990, -0.2842225609755594795, -1.577752156565102655E-15 ) ) ;
#6172 = AXIS2_PLACEMENT_3D ( 'NONE', #13897, #3950, #28336 ) ;
#6173 = AXIS2_PLACEMENT_3D ( 'NONE', #10920, #22828, #20301 ) ;
#6174 = CARTESIAN_POINT ( 'NONE',  ( 28.63101374161907842, 6.274379892050022001, -1.425000000000099742 ) ) ;
#6176 = FACE_OUTER_BOUND ( 'NONE', #28367, .T. ) ;
#6175 = CARTESIAN_POINT ( 'NONE',  ( -60.19702994616203995, 4.156921938165313080, -1.985113767892243204E-13 ) ) ;
#6177 = CARTESIAN_POINT ( 'NONE',  ( -56.79792740578360366, -1.073804522883517132, -3.225979517392335794 ) ) ;
#6178 = DIRECTION ( 'NONE',  ( 0.000000000000000000, 0.2008964009354147484, -0.9796124928211139560 ) ) ;
#6179 = APPLICATION_PROTOCOL_DEFINITION ( 'draft international standard', 'automotive_design', 1998, #26924 ) ;
#6180 = CARTESIAN_POINT ( 'NONE',  ( 52.59308447829369726, 4.500429781219338565, -1.566000285930613023 ) ) ;
#6181 = EDGE_CURVE ( 'NONE', #3817, #2745, #22155, .T. ) ;
#6182 = ORIENTED_EDGE ( 'NONE', *, *, #21423, .F. ) ;
#6183 = ADVANCED_FACE ( 'NONE', ( #9459 ), #21525, .F. ) ;
#6184 = CARTESIAN_POINT ( 'NONE',  ( -60.19702994616203995, 4.156921938165313080, -1.985113767892243204E-13 ) ) ;
#6185 = ADVANCED_FACE ( 'NONE', ( #2484 ), #29216, .F. ) ;
#6186 = CARTESIAN_POINT ( 'NONE',  ( 52.10572631149717182, 8.700000001568275465, -2.050000000000181455 ) ) ;
#6187 = DIRECTION ( 'NONE',  ( 1.047444401652940007E-14, -1.000000000000000000, 0.000000000000000000 ) ) ;
#6188 = CARTESIAN_POINT ( 'NONE',  ( 15.03925126672132784, 0.7747498368337703001, 5.363501452440938344 ) ) ;
#6189 = LINE ( 'NONE', #20151, #2384 ) ;
#6190 = DIRECTION ( 'NONE',  ( -3.489354422748178582E-15, 1.218509414717996338E-16, -1.000000000000000000 ) ) ;
#6191 = DIRECTION ( 'NONE',  ( 0.000000000000000000, 0.000000000000000000, -1.000000000000000000 ) ) ;
#6192 = CARTESIAN_POINT ( 'NONE',  ( -54.49999999999997158, 3.695864355900486231, -0.2535994654912652191 ) ) ;
#6193 = ORIENTED_EDGE ( 'NONE', *, *, #4275, .T. ) ;
#6194 =( BOUNDED_SURFACE ( )  B_SPLINE_SURFACE ( 3, 2, ( 
 ( #1036, #3245, #12886 ),
 ( #22575, #7684, #14954 ),
 ( #7828, #24623, #27462 ),
 ( #22271, #557, #10215 ),
 ( #19883, #29514, #17503 ),
 ( #27158, #3705, #30305 ),
 ( #1631, #15889, #25548 ),
 ( #23348, #10835, #8469 ),
 ( #23203, #13810, #20822 ),
 ( #30451, #25400, #18146 ) ),
 .UNSPECIFIED., .F., .F., .F. ) 
 B_SPLINE_SURFACE_WITH_KNOTS ( ( 4, 2, 2, 2, 4 ),
 ( 3, 3 ),
 ( -4.878909776184769953E-18, 0.0003534454412679794333, 0.0007068908825359637455, 0.001060336323803948112, 0.001413781765071932478 ),
 ( 0.000000000000000000, 1.000000000000000000 ),
 .UNSPECIFIED. ) 
 GEOMETRIC_REPRESENTATION_ITEM ( )  RATIONAL_B_SPLINE_SURFACE ( (
 ( 1.000000000000000000, 0.6992058987801016423, 1.000000000000000000),
 ( 1.000000000000000000, 0.6992660572530883245, 1.000000000000000000),
 ( 1.000000000000000000, 0.6974033530225959288, 1.000000000000000000),
 ( 1.000000000000000000, 0.6920435876578637791, 1.000000000000000000),
 ( 1.000000000000000000, 0.6885661196046906074, 1.000000000000000000),
 ( 1.000000000000000000, 0.6845372766840260859, 1.000000000000000000),
 ( 1.000000000000000000, 0.6841195446886403353, 1.000000000000000000),
 ( 1.000000000000000000, 0.6902705495948038283, 1.000000000000000000),
 ( 1.000000000000000000, 0.6968978290748681914, 1.000000000000000000),
 ( 1.000000000000000000, 0.7071067811865727748, 1.000000000000000000) ) ) 
 REPRESENTATION_ITEM ( '' )  SURFACE ( )  );
#6195 = DIRECTION ( 'NONE',  ( 1.000000000000000000, 1.047444401652940007E-14, 0.000000000000000000 ) ) ;
#6196 = CARTESIAN_POINT ( 'NONE',  ( -35.85663232820584057, 4.018128179617551865, -3.618665901676622720 ) ) ;
#6197 = AXIS2_PLACEMENT_3D ( 'NONE', #27143, #23998, #29361 ) ;
#6199 = CARTESIAN_POINT ( 'NONE',  ( -59.69142724121850563, -2.412383461849193278, -1.233589124872107146 ) ) ;
#6198 = LINE ( 'NONE', #16326, #24605 ) ;
#6200 = CARTESIAN_POINT ( 'NONE',  ( 15.03925126672127988, -5.086913985776152280, 1.171642053949085494 ) ) ;
#6201 = VERTEX_POINT ( 'NONE', #7381 ) ;
#6202 = CARTESIAN_POINT ( 'NONE',  ( 52.18319145150646676, 8.687974897284844289, 2.049999999999818190 ) ) ;
#6203 = CARTESIAN_POINT ( 'NONE',  ( 47.04714695228949495, -4.172892586174061336, 1.014428651009327442 ) ) ;
#6204 = EDGE_LOOP ( 'NONE', ( #235, #8965, #1890, #9902 ) ) ;
#6205 = B_SPLINE_CURVE_WITH_KNOTS ( 'NONE', 3,
 ( #2, #20063, #9669, #27326, #8018, #27473 ),
 .UNSPECIFIED., .F., .F.,
 ( 4, 2, 4 ),
 ( 0.000000000000000000, 0.0001614717865051737596, 0.0003229435730103475191 ),
 .UNSPECIFIED. ) ;
#6206 = ORIENTED_EDGE ( 'NONE', *, *, #2618, .T. ) ;
#6207 = CARTESIAN_POINT ( 'NONE',  ( 58.75000000000000711, 0.8948927608039202175, -1.760622601996761460 ) ) ;
#6208 = CARTESIAN_POINT ( 'NONE',  ( 47.87911513861941870, -4.387164041431065975, -1.383037119376925972 ) ) ;
#6209 = VERTEX_POINT ( 'NONE', #24626 ) ;
#6210 = FILL_AREA_STYLE ('',( #4291 ) ) ;
#6211 = CARTESIAN_POINT ( 'NONE',  ( -55.95655989232412963, -3.925981830489445379, -2.129311736262419800E-13 ) ) ;
#6212 = ORIENTED_EDGE ( 'NONE', *, *, #20691, .F. ) ;
#6213 = CARTESIAN_POINT ( 'NONE',  ( -54.44999999999997442, 2.818925648462311528E-15, 9.856100559121352825E-17 ) ) ;
#6214 = VERTEX_POINT ( 'NONE', #12427 ) ;
#6215 = ADVANCED_FACE ( 'NONE', ( #19745 ), #21493, .T. ) ;
#6216 = ORIENTED_EDGE ( 'NONE', *, *, #19892, .F. ) ;
#6217 = EDGE_CURVE ( 'NONE', #25275, #10297, #26992, .T. ) ;
#6218 = CARTESIAN_POINT ( 'NONE',  ( -56.62499999999996447, 2.944486372867106905, -1.700000000000188471 ) ) ;
#6219 = ADVANCED_FACE ( 'NONE', ( #21816 ), #105, .F. ) ;
#6220 = CARTESIAN_POINT ( 'NONE',  ( 61.25000000000004263, -1.800471618824687869, 1.039502773796719959 ) ) ;
#6221 = DIRECTION ( 'NONE',  ( 1.000000000000000000, 1.047444401652940007E-14, -0.000000000000000000 ) ) ;
#6222 = CONICAL_SURFACE ( 'NONE', #27953, 1.875000000000001776, 0.7853981633974510546 ) ;
#6223 = DIRECTION ( 'NONE',  ( -2.614375865348240525E-16, 0.2008964009354147484, -0.9796124928211139560 ) ) ;
#6224 = CARTESIAN_POINT ( 'NONE',  ( -54.39999999999997726, -3.624999999999988010, -2.339607799264337154E-13 ) ) ;
#6226 = CARTESIAN_POINT ( 'NONE',  ( 47.00000000000002132, 1.734723475976807094E-15, 0.000000000000000000 ) ) ;
#6225 = CARTESIAN_POINT ( 'NONE',  ( 17.21035195517769267, -2.471857751707523654E-15, 0.000000000000000000 ) ) ;
#6227 = CYLINDRICAL_SURFACE ( 'NONE', #842, 3.624999999999996447 ) ;
#6228 = DIRECTION ( 'NONE',  ( -1.000000000000000000, -0.000000000000000000, -0.000000000000000000 ) ) ;
#6229 = DIRECTION ( 'NONE',  ( -0.000000000000000000, 8.673617379884032317E-15, 1.000000000000000000 ) ) ;
#6230 = EDGE_CURVE ( 'NONE', #6099, #7928, #29376, .T. ) ;
#6231 = CARTESIAN_POINT ( 'NONE',  ( 58.75000018595672913, -1.701752411746506821, -0.9248597378502191324 ) ) ;
#6232 = DIRECTION ( 'NONE',  ( 0.000000000000000000, 0.000000000000000000, 1.000000000000000000 ) ) ;
#6233 = CARTESIAN_POINT ( 'NONE',  ( 53.90826771765248537, 6.078164526406591328, -1.689602626210267466 ) ) ;
#6234 = VERTEX_POINT ( 'NONE', #17059 ) ;
#6235 = CYLINDRICAL_SURFACE ( 'NONE', #25222, 2.000000000000000000 ) ;
#6236 = CARTESIAN_POINT ( 'NONE',  ( -59.09999999999997300, 8.366749974758448157E-15, -2.099585467500611340E-13 ) ) ;
#6237 = ORIENTED_EDGE ( 'NONE', *, *, #28141, .T. ) ;
#6238 = FACE_OUTER_BOUND ( 'NONE', #23691, .T. ) ;
#6239 = PRODUCT_DEFINITION ( 'UNKNOWN', '', #17706, #17737 ) ;
#6240 = AXIS2_PLACEMENT_3D ( 'NONE', #15812, #25461, #1403 ) ;
#6241 = CARTESIAN_POINT ( 'NONE',  ( 59.00000000000002132, 1.401298464324817071E-42, -6.179921969752347932E-13 ) ) ;
#6243 = CARTESIAN_POINT ( 'NONE',  ( -73.89999999999997726, -2.435524336289708093E-15, 4.607889071584891164E-15 ) ) ;
#6242 = CARTESIAN_POINT ( 'NONE',  ( -57.74999999999997158, -2.944486372867089141, 1.699999999999783906 ) ) ;
#6244 = ORIENTED_EDGE ( 'NONE', *, *, #24488, .F. ) ;
#6245 = CIRCLE ( 'NONE', #3213, 0.1000000000000000472 ) ;
#6246 = ORIENTED_EDGE ( 'NONE', *, *, #2171, .F. ) ;
#6247 = LINE ( 'NONE', #28251, #30070 ) ;
#6248 = EDGE_LOOP ( 'NONE', ( #30369, #13520, #8307, #27484 ) ) ;
#6249 = DIRECTION ( 'NONE',  ( -1.000000000000000000, -4.939082069373669245E-17, 1.520093157366878429E-16 ) ) ;
#6250 = EDGE_LOOP ( 'NONE', ( #15388, #10119, #22275 ) ) ;
#6251 = CARTESIAN_POINT ( 'NONE',  ( 23.88937650878775543, 5.720041404659518491, -2.050000000000081979 ) ) ;
#6252 = CARTESIAN_POINT ( 'NONE',  ( -62.06710100716625789, -2.641521085243120570, -0.3278585316293294305 ) ) ;
#6253 = DIRECTION ( 'NONE',  ( 0.000000000000000000, 0.000000000000000000, 1.000000000000000000 ) ) ;
#6254 = ORIENTED_EDGE ( 'NONE', *, *, #1875, .F. ) ;
#6255 = EDGE_CURVE ( 'NONE', #11263, #16493, #25161, .T. ) ;
#6256 = CARTESIAN_POINT ( 'NONE',  ( 47.00000000000002842, -4.131056160354152240, -1.099999999999999867 ) ) ;
#6257 = CARTESIAN_POINT ( 'NONE',  ( -73.89999999999996305, 1.301636140808604125, 0.03242509391110788564 ) ) ;
#6258 = CARTESIAN_POINT ( 'NONE',  ( 51.14630318392396902, -0.9364487020628400327, 1.503522130792752209 ) ) ;
#6259 = DIRECTION ( 'NONE',  ( 0.000000000000000000, -0.9996898646859344595, -0.02490330187381124133 ) ) ;
#6260 = CARTESIAN_POINT ( 'NONE',  ( 15.32766723174653123, 2.228024565339362439, 4.927420728799238425 ) ) ;
#6261 = CARTESIAN_POINT ( 'NONE',  ( -59.19999999999997442, -2.444956024269904660, 1.250136525132532261 ) ) ;
#6262 = DIRECTION ( 'NONE',  ( 0.000000000000000000, -1.000000000000000000, -3.491481338843133355E-15 ) ) ;
#6264 = CARTESIAN_POINT ( 'NONE',  ( 51.80000000000003268, -3.994423162662135152, 2.070282222599607813 ) ) ;
#6263 = DIRECTION ( 'NONE',  ( 1.000000000000000000, 1.047444401652940007E-14, 0.000000000000000000 ) ) ;
#6265 = AXIS2_PLACEMENT_3D ( 'NONE', #9048, #16177, #13461 ) ;
#6266 = CARTESIAN_POINT ( 'NONE',  ( 51.80000000000001137, -4.131056160354152240, 1.099999999999999423 ) ) ;
#6267 = DIRECTION ( 'NONE',  ( -2.085103575917242148E-15, -0.9615843008030771077, 0.2745098039215673746 ) ) ;
#6268 = EDGE_CURVE ( 'NONE', #133, #7683, #19127, .T. ) ;
#6269 = CARTESIAN_POINT ( 'NONE',  ( 61.25000000000004263, -1.960427193527463086, 0.3958853607744572956 ) ) ;
#6270 = ORIENTED_EDGE ( 'NONE', *, *, #11386, .T. ) ;
#6271 = CARTESIAN_POINT ( 'NONE',  ( 54.27670628353131121, 6.362024822791419787, -2.050000000000186340 ) ) ;
#6272 = VERTEX_POINT ( 'NONE', #26386 ) ;
#6273 = CARTESIAN_POINT ( 'NONE',  ( 51.79699096306529782, -3.614067288481912499, 1.940243272267534902 ) ) ;
#6274 = VERTEX_POINT ( 'NONE', #7229 ) ;
#6275 = CARTESIAN_POINT ( 'NONE',  ( 52.41186875581716720, 8.643425072357743488, 2.049999999999817302 ) ) ;
#6276 = CARTESIAN_POINT ( 'NONE',  ( -58.59585481156723574, 3.673546848079181970, 0.7533615035078067290 ) ) ;
#6277 = DIRECTION ( 'NONE',  ( -1.000000000000000000, -3.054025858079668409E-16, 2.042474015755241579E-16 ) ) ;
#6278 = ORIENTED_EDGE ( 'NONE', *, *, #12527, .F. ) ;
#6279 = ORIENTED_EDGE ( 'NONE', *, *, #10194, .T. ) ;
#6280 = CARTESIAN_POINT ( 'NONE',  ( 26.91677043723410989, 5.349113832900135534, -2.050000000000093525 ) ) ;
#6281 = CARTESIAN_POINT ( 'NONE',  ( 52.13000000000003098, -0.4999999999994542144, 1.718465885608440491 ) ) ;
#6282 = VERTEX_POINT ( 'NONE', #26533 ) ;
#6284 = CARTESIAN_POINT ( 'NONE',  ( -54.39999999999999147, -1.400000000000006795, 3.959797974644449603 ) ) ;
#6283 = DIRECTION ( 'NONE',  ( 1.000000000000000000, 0.000000000000000000, 0.000000000000000000 ) ) ;
#6285 = DIRECTION ( 'NONE',  ( -1.520093157366894206E-16, 0.5877852522924802425, -0.8090169943749422332 ) ) ;
#6286 = ORIENTED_EDGE ( 'NONE', *, *, #11078, .F. ) ;
#6287 = CIRCLE ( 'NONE', #24473, 0.1000000000000001027 ) ;
#6288 = CARTESIAN_POINT ( 'NONE',  ( -60.24999999999997868, 0.6177564328764024726, -3.012308415424925556 ) ) ;
#6289 = CARTESIAN_POINT ( 'NONE',  ( 58.74160516400052501, 1.784764912520735214, -0.5747049900151632862 ) ) ;
#6290 = EDGE_CURVE ( 'NONE', #9260, #18734, #19135, .T. ) ;
#6291 = DIRECTION ( 'NONE',  ( 0.000000000000000000, 0.000000000000000000, 1.000000000000000000 ) ) ;
#6292 = LINE ( 'NONE', #1683, #13720 ) ;
#6293 = CARTESIAN_POINT ( 'NONE',  ( -56.57202994616203995, 2.078460969082674747, -3.600000000000191935 ) ) ;
#6294 = AXIS2_PLACEMENT_3D ( 'NONE', #16937, #24055, #24676 ) ;
#6295 = EDGE_CURVE ( 'NONE', #4182, #23309, #8796, .T. ) ;
#6296 = CARTESIAN_POINT ( 'NONE',  ( 58.75000000000002842, -1.039502773796102897, -1.800471618824325493 ) ) ;
#6297 = AXIS2_PLACEMENT_3D ( 'NONE', #17662, #551, #13197 ) ;
#6298 = CARTESIAN_POINT ( 'NONE',  ( -58.73542740578359656, 2.936324665650196675, 2.606018187048510626 ) ) ;
#6299 = ADVANCED_FACE ( 'NONE', ( #27624 ), #27160, .T. ) ;
#6300 = CARTESIAN_POINT ( 'NONE',  ( -56.78335481156722864, -4.108500314926509134, 1.367561758111407455 ) ) ;
#6301 = CIRCLE ( 'NONE', #5282, 0.7500000000000002220 ) ;
#6302 = DIRECTION ( 'NONE',  ( 0.000000000000000000, 0.000000000000000000, -1.000000000000000000 ) ) ;
#6303 = CARTESIAN_POINT ( 'NONE',  ( -59.69999999999997442, -3.399999999999991473, -2.235080921937235780E-13 ) ) ;
#6304 = FACE_OUTER_BOUND ( 'NONE', #18155, .T. ) ;
#6305 = ORIENTED_EDGE ( 'NONE', *, *, #1277, .T. ) ;
#6306 = DIRECTION ( 'NONE',  ( 0.000000000000000000, 0.000000000000000000, -1.000000000000000000 ) ) ;
#6307 = VERTEX_POINT ( 'NONE', #3571 ) ;
#6308 = AXIS2_PLACEMENT_3D ( 'NONE', #22996, #10949, #20637 ) ;
#6309 = DIRECTION ( 'NONE',  ( 1.000000000000000000, 1.047444401652940007E-14, 0.000000000000000000 ) ) ;
#6311 = FACE_OUTER_BOUND ( 'NONE', #10214, .T. ) ;
#6310 = CARTESIAN_POINT ( 'NONE',  ( 48.33046193264123502, 1.143620537822834349, 3.937943076466140724 ) ) ;
#6312 = EDGE_CURVE ( 'NONE', #9733, #10218, #15567, .T. ) ;
#6313 = ORIENTED_EDGE ( 'NONE', *, *, #19533, .F. ) ;
#6314 = VERTEX_POINT ( 'NONE', #15606 ) ;
#6315 = CARTESIAN_POINT ( 'NONE',  ( 53.91582462592152325, 6.672259099522126036, -1.484311132272649436 ) ) ;
#6316 = DIRECTION ( 'NONE',  ( -1.000000000000000000, -3.053848253006669023E-16, 2.042510438544995169E-16 ) ) ;
#6318 = DIRECTION ( 'NONE',  ( 0.000000000000000000, 0.2008964009354162750, -0.9796124928211136229 ) ) ;
#6317 = DIRECTION ( 'NONE',  ( 1.000000000000000000, 1.047444401652940007E-14, 0.000000000000000000 ) ) ;
#6319 = ORIENTED_EDGE ( 'NONE', *, *, #23410, .F. ) ;
#6320 = CARTESIAN_POINT ( 'NONE',  ( -58.17292740578360366, 2.256877952708268964, -2.542931754211925188 ) ) ;
#6321 = CARTESIAN_POINT ( 'NONE',  ( -36.40793637698146767, 2.334444681449654446, 4.877899991435294957 ) ) ;
#6322 = CONTEXT_DEPENDENT_SHAPE_REPRESENTATION ( #29602, #25769 ) ;
#6323 = CARTESIAN_POINT ( 'NONE',  ( -59.35358983848620795, 2.308634493194285486, 1.301040651491357503 ) ) ;
#6324 = EDGE_CURVE ( 'NONE', #7871, #27840, #26185, .T. ) ;
#6325 = AXIS2_PLACEMENT_3D ( 'NONE', #6402, #20973, #3866 ) ;
#6326 = CARTESIAN_POINT ( 'NONE',  ( 22.32354329814791782, 7.018810584857204660, 1.949999999999922240 ) ) ;
#6327 = ADVANCED_FACE ( 'NONE', ( #1180 ), #11019, .F. ) ;
#6328 = ORIENTED_EDGE ( 'NONE', *, *, #19699, .T. ) ;
#6329 = FACE_OUTER_BOUND ( 'NONE', #9620, .T. ) ;
#6330 = TOROIDAL_SURFACE ( 'NONE', #765, 1.375000000000001332, 0.2500000000000000000 ) ;
#6331 = CARTESIAN_POINT ( 'NONE',  ( 61.25000000000001421, 0.9840188032656856931, -1.660129320691967614 ) ) ;
#6332 = CARTESIAN_POINT ( 'NONE',  ( -59.69999999999998153, 2.121207708687718352, 1.750136525132546472 ) ) ;
#6333 = CARTESIAN_POINT ( 'NONE',  ( 58.75000000000000711, 1.791164585742715198, 0.8897917884450912140 ) ) ;
#6334 = DIRECTION ( 'NONE',  ( -1.000000000000000000, -3.054025858079668409E-16, 2.042474015755241579E-16 ) ) ;
#6336 = CARTESIAN_POINT ( 'NONE',  ( -54.49999999999996447, -1.557046979865753578, -3.273565289175143445 ) ) ;
#6335 = DIRECTION ( 'NONE',  ( 0.000000000000000000, 1.000000000000000000, -8.673617379884030739E-15 ) ) ;
#6337 = AXIS2_PLACEMENT_3D ( 'NONE', #30395, #15539, #18239 ) ;
#6338 = DIRECTION ( 'NONE',  ( 0.000000000000000000, 0.2008964009354147762, -0.9796124928211139560 ) ) ;
#6340 = CARTESIAN_POINT ( 'NONE',  ( -54.49999999999997868, 3.673546848079182858, 0.7533615035078058408 ) ) ;
#6339 = DIRECTION ( 'NONE',  ( -1.000000000000000000, -2.586136946169074517E-16, 0.000000000000000000 ) ) ;
#6341 = VECTOR ( 'NONE', #25701, 1000.000000000000000 ) ;
#6342 = ORIENTED_EDGE ( 'NONE', *, *, #3470, .F. ) ;
#6343 = CARTESIAN_POINT ( 'NONE',  ( 60.75000000000002842, -0.4999999999993638977, -1.718465885608440047 ) ) ;
#6344 = DIRECTION ( 'NONE',  ( 0.000000000000000000, 0.000000000000000000, 1.000000000000000000 ) ) ;
#6346 = LINE ( 'NONE', #16005, #29810 ) ;
#6345 = CARTESIAN_POINT ( 'NONE',  ( 58.75000000000000000, 1.834410884276219234, 0.3880228184671279945 ) ) ;
#6347 = DIRECTION ( 'NONE',  ( -9.654113257610060303E-15, 0.000000000000000000, -1.000000000000000000 ) ) ;
#6348 = EDGE_CURVE ( 'NONE', #23319, #20985, #19245, .T. ) ;
#6349 = ORIENTED_EDGE ( 'NONE', *, *, #9159, .T. ) ;
#6350 = CARTESIAN_POINT ( 'NONE',  ( 53.04927178323141845, 4.171861402708406885, 2.049999999999814637 ) ) ;
#6351 = DIRECTION ( 'NONE',  ( 1.000000000000000000, 2.586136946169074517E-16, -0.000000000000000000 ) ) ;
#6352 = CIRCLE ( 'NONE', #29093, 0.2000000000000000944 ) ;
#6353 = ORIENTED_EDGE ( 'NONE', *, *, #21694, .F. ) ;
#6354 = ADVANCED_FACE ( 'NONE', ( #12739 ), #27809, .T. ) ;
#6355 = DIRECTION ( 'NONE',  ( 1.000000000000000000, 1.047444401652940007E-14, 0.000000000000000000 ) ) ;
#6356 = EDGE_LOOP ( 'NONE', ( #15149, #7411, #7301, #24469, #14305, #8492, #28636, #19032, #5835 ) ) ;
#6357 = DIRECTION ( 'NONE',  ( -1.000000000000000000, -0.000000000000000000, -0.000000000000000000 ) ) ;
#6358 = CYLINDRICAL_SURFACE ( 'NONE', #22070, 0.04999999999999991257 ) ;
#6359 = EDGE_LOOP ( 'NONE', ( #28626, #729, #24440, #4760 ) ) ;
#6360 = CARTESIAN_POINT ( 'NONE',  ( 23.82615635345663563, 5.749986595043423243, 1.949999999999916689 ) ) ;
#6361 = CARTESIAN_POINT ( 'NONE',  ( -56.95655989232412963, 1.962990915244722245, 3.399999999999804956 ) ) ;
#6362 = ORIENTED_EDGE ( 'NONE', *, *, #16089, .T. ) ;
#6363 = CYLINDRICAL_SURFACE ( 'NONE', #26727, 3.750000000000000444 ) ;
#6364 = ORIENTED_EDGE ( 'NONE', *, *, #6152, .T. ) ;
#6365 = EDGE_CURVE ( 'NONE', #19303, #3444, #8158, .T. ) ;
#6366 = AXIS2_PLACEMENT_3D ( 'NONE', #11355, #21044, #16429 ) ;
#6367 = VERTEX_POINT ( 'NONE', #15433 ) ;
#6368 = AXIS2_PLACEMENT_3D ( 'NONE', #2872, #22045, #7315 ) ;
#6369 = CARTESIAN_POINT ( 'NONE',  ( -57.93749999999998579, 1.962990915244722689, 3.399999999999801847 ) ) ;
#6370 = CARTESIAN_POINT ( 'NONE',  ( 56.96117471280891209, -0.7619384116854249767, 2.485869561276773165 ) ) ;
#6371 = CARTESIAN_POINT ( 'NONE',  ( 26.41339658680652391, 5.213169555504945762, -1.425000000000092637 ) ) ;
#6372 = AXIS2_PLACEMENT_3D ( 'NONE', #4069, #8799, #11338 ) ;
#6373 = LINE ( 'NONE', #16036, #5875 ) ;
#6374 = CIRCLE ( 'NONE', #18501, 0.1500000000000001887 ) ;
#6375 = CARTESIAN_POINT ( 'NONE',  ( 57.04707324256202128, 0.7500000000000492939, 2.421260002560643443 ) ) ;
#6376 = AXIS2_PLACEMENT_3D ( 'NONE', #19403, #21942, #26968 ) ;
#6377 = CIRCLE ( 'NONE', #6907, 4.279289321881344144 ) ;
#6378 =( BOUNDED_CURVE ( )  B_SPLINE_CURVE ( 2, ( #25064, #3551, #3397, #15876, #13188, #3848, #18426, #11131, #29827 ),
 .UNSPECIFIED., .F., .T. ) 
 B_SPLINE_CURVE_WITH_KNOTS ( ( 3, 2, 2, 2, 3 ),
 ( 0.1388888888888888951, 0.1481481481481481399, 0.1666666666666666574, 0.1851851851851851749, 0.1944444444444444475 ),
 .UNSPECIFIED. ) 
 CURVE ( )  GEOMETRIC_REPRESENTATION_ITEM ( )  RATIONAL_B_SPLINE_CURVE ( ( 0.9330127018922192983, 0.9330127018922194093, 1.000000000000000000, 0.8660254037844387076, 1.000000000000000000, 0.8660254037844387076, 1.000000000000000000, 0.9330127018922191873, 0.9330127018922192983 ) ) 
 REPRESENTATION_ITEM ( '' )  );
#6379 = COLOUR_RGB ( '', 0.72549020, 0.75294118, 0.79215686) ;
#6381 = LINE ( 'NONE', #28060, #9851 ) ;
#6380 = CARTESIAN_POINT ( 'NONE',  ( -36.40878371307407946, 4.755985070912289281, -2.573747172434650121 ) ) ;
#6382 = DIRECTION ( 'NONE',  ( 1.000000000000000000, 3.054025858079668409E-16, -2.042474015755241579E-16 ) ) ;
#6383 = CARTESIAN_POINT ( 'NONE',  ( -59.68033635780795976, -2.213242577962092117, 1.527458850614529018 ) ) ;
#6384 = DIRECTION ( 'NONE',  ( -3.002035892788116966E-16, 0.9996898646859343485, 0.02490330187381123786 ) ) ;
#6385 = CARTESIAN_POINT ( 'NONE',  ( -61.34999999999997300, -2.574153985709302539, -0.5872647410103332133 ) ) ;
#6386 = ORIENTED_EDGE ( 'NONE', *, *, #3415, .F. ) ;
#6387 = CARTESIAN_POINT ( 'NONE',  ( 47.00000000000002132, -3.726179070414207928, 1.100000000000000311 ) ) ;
#6388 = EDGE_CURVE ( 'NONE', #1635, #24203, #1492, .T. ) ;
#6389 = CIRCLE ( 'NONE', #24097, 4.299999999999998046 ) ;
#6390 = CARTESIAN_POINT ( 'NONE',  ( -35.85663232820584057, -1.123735532908306523, -5.289358697221545391 ) ) ;
#6391 = EDGE_CURVE ( 'NONE', #24892, #20124, #12630, .T. ) ;
#6392 = AXIS2_PLACEMENT_3D ( 'NONE', #12568, #17654, #21801 ) ;
#6393 = VERTEX_POINT ( 'NONE', #25085 ) ;
#6394 = EDGE_CURVE ( 'NONE', #2692, #24817, #21254, .T. ) ;
#6395 = CARTESIAN_POINT ( 'NONE',  ( -54.49999999999997868, -3.524999999999988365, -2.339607799264337154E-13 ) ) ;
#6396 = CARTESIAN_POINT ( 'NONE',  ( -60.86042740578358945, -0.7887156198831608567, 3.845940847736174728 ) ) ;
#6398 = CARTESIAN_POINT ( 'NONE',  ( -44.49999999999997868, 6.542789527549899840E-15, -1.397091617737396343E-15 ) ) ;
#6397 = CARTESIAN_POINT ( 'NONE',  ( -57.49999999999995737, 2.023778652682507790E-14, -3.400000000000204636 ) ) ;
#6399 = ORIENTED_EDGE ( 'NONE', *, *, #20748, .T. ) ;
#6400 = CIRCLE ( 'NONE', #318, 0.05000000000000012768 ) ;
#6401 = EDGE_LOOP ( 'NONE', ( #21385, #1269, #7225, #17277 ) ) ;
#6402 = CARTESIAN_POINT ( 'NONE',  ( -59.29999999999997584, 2.330309927981285032E-15, 4.253626757584724400E-16 ) ) ;
#6403 = ORIENTED_EDGE ( 'NONE', *, *, #7742, .T. ) ;
#6404 = AXIS2_PLACEMENT_3D ( 'NONE', #22902, #8020, #5310 ) ;
#6406 = DIRECTION ( 'NONE',  ( 0.000000000000000000, -7.105427357601001859E-15, 1.000000000000000000 ) ) ;
#6405 = CIRCLE ( 'NONE', #24108, 0.05000000000000014849 ) ;
#6407 = CARTESIAN_POINT ( 'NONE',  ( -61.34999999999997300, -2.551764585593653489, 0.6636807913650824009 ) ) ;
#6408 = ORIENTED_EDGE ( 'NONE', *, *, #8812, .F. ) ;
#6409 = CARTESIAN_POINT ( 'NONE',  ( 24.76493886322366222, 5.404133871204292561, -2.050000000000152589 ) ) ;
#6410 = CIRCLE ( 'NONE', #10967, 4.835355339059328017 ) ;
#6411 = DIRECTION ( 'NONE',  ( -1.000000000000000000, 1.219044193948984088E-29, -3.491481338843133750E-15 ) ) ;
#6412 = CARTESIAN_POINT ( 'NONE',  ( -44.59999999999996589, 1.500000000000021538, -3.363870538531645416 ) ) ;
#6413 = ORIENTED_EDGE ( 'NONE', *, *, #26831, .T. ) ;
#6414 = ORIENTED_EDGE ( 'NONE', *, *, #21399, .F. ) ;
#6415 = ADVANCED_FACE ( 'NONE', ( #8306 ), #17440, .T. ) ;
#6416 = CARTESIAN_POINT ( 'NONE',  ( 69.20000000000004547, -0.6617647058823530326, 1.754335336828708902 ) ) ;
#6417 = CARTESIAN_POINT ( 'NONE',  ( 51.59739104186229497, -1.010292945602100367, -1.272765950230261067 ) ) ;
#6418 = CARTESIAN_POINT ( 'NONE',  ( 51.41321594800584194, -0.9846907464474132787, 1.426729742943413148 ) ) ;
#6419 = AXIS2_PLACEMENT_3D ( 'NONE', #28950, #4101, #13740 ) ;
#6420 = CARTESIAN_POINT ( 'NONE',  ( 47.12894858146291455, -3.772456960769013712, 1.610749547355264433 ) ) ;
#6421 = DIRECTION ( 'NONE',  ( -1.000000000000000000, 0.000000000000000000, 3.491481338843133355E-15 ) ) ;
#6422 = CIRCLE ( 'NONE', #18075, 0.09999999999999997780 ) ;
#6423 = CARTESIAN_POINT ( 'NONE',  ( -54.39999999999997726, -6.102218906431378987E-14, -2.213041600731275921E-13 ) ) ;
#6424 = AXIS2_PLACEMENT_3D ( 'NONE', #23148, #10777, #5721 ) ;
#6425 = CARTESIAN_POINT ( 'NONE',  ( 61.25000000000002132, 6.415596960124259844E-13, 3.111507638930570854E-58 ) ) ;
#6427 = FACE_OUTER_BOUND ( 'NONE', #18244, .T. ) ;
#6426 = CARTESIAN_POINT ( 'NONE',  ( -36.22955757456062287, -2.840625797033914157, 4.363718033548201092 ) ) ;
#6428 = CIRCLE ( 'NONE', #1786, 2.000000000000000000 ) ;
#6429 = CIRCLE ( 'NONE', #18577, 1.000000000000000000 ) ;
#6430 = CARTESIAN_POINT ( 'NONE',  ( 51.80000000000001137, -4.227689052994008101, 1.125730994152044362 ) ) ;
#6431 = FACE_OUTER_BOUND ( 'NONE', #29309, .T. ) ;
#6432 = DIRECTION ( 'NONE',  ( -2.581436205204234499E-16, 0.9796124928211140670, 0.2008964009354147762 ) ) ;
#6433 = AXIS2_PLACEMENT_3D ( 'NONE', #25572, #1358, #15455 ) ;
#6434 = FACE_OUTER_BOUND ( 'NONE', #16540, .T. ) ;
#6435 = CIRCLE ( 'NONE', #25111, 0.05000000000000012768 ) ;
#6436 = ORIENTED_EDGE ( 'NONE', *, *, #9419, .F. ) ;
#6437 = ORIENTED_EDGE ( 'NONE', *, *, #22825, .F. ) ;
#6438 = EDGE_CURVE ( 'NONE', #29220, #11262, #18709, .T. ) ;
#6439 = CYLINDRICAL_SURFACE ( 'NONE', #18911, 2.000000000000000000 ) ;
#6440 = ORIENTED_EDGE ( 'NONE', *, *, #18781, .T. ) ;
#6441 = CARTESIAN_POINT ( 'NONE',  ( 53.90340377275678918, 6.895264694548083995, 1.787725782035106459 ) ) ;
#6442 = CARTESIAN_POINT ( 'NONE',  ( -56.84585481156722864, -2.489203624310586616, 2.804704140674918467 ) ) ;
#6444 = CARTESIAN_POINT ( 'NONE',  ( 50.93192783270057333, -3.937842570012147547, -1.145831914963376219 ) ) ;
#6443 = CARTESIAN_POINT ( 'NONE',  ( -69.18535533905931345, -6.887031541980249260E-16, 2.444420817412074983E-15 ) ) ;
#6445 = AXIS2_PLACEMENT_3D ( 'NONE', #16265, #18808, #26234 ) ;
#6446 = ORIENTED_EDGE ( 'NONE', *, *, #3672, .T. ) ;
#6447 = CARTESIAN_POINT ( 'NONE',  ( 25.08846173237438748, 5.428824289251027224, -2.050000000000087308 ) ) ;
#6448 = AXIS2_PLACEMENT_3D ( 'NONE', #19119, #31288, #26225 ) ;
#6449 = CARTESIAN_POINT ( 'NONE',  ( -60.49999999999995737, 0.8596938233273154761, -4.192045280110956895 ) ) ;
#6450 = AXIS2_PLACEMENT_3D ( 'NONE', #22988, #20631, #27418 ) ;
#6451 = ORIENTED_EDGE ( 'NONE', *, *, #17555, .F. ) ;
#6453 = CARTESIAN_POINT ( 'NONE',  ( -41.12388279035661753, 5.147405183146855023, 0.000000000000000000 ) ) ;
#6452 = CARTESIAN_POINT ( 'NONE',  ( 50.25000000000002842, -1.039502773797060131, 1.800471618824829756 ) ) ;
#6454 = CARTESIAN_POINT ( 'NONE',  ( 51.87765138016307986, 8.698644590117595499, -2.050000000000180123 ) ) ;
#6455 = ORIENTED_EDGE ( 'NONE', *, *, #22698, .T. ) ;
#6456 = DIRECTION ( 'NONE',  ( 0.000000000000000000, 0.000000000000000000, 1.000000000000000000 ) ) ;
#6457 = CARTESIAN_POINT ( 'NONE',  ( 58.72204580543391472, 1.805265037612412860, -0.5070891929463556824 ) ) ;
#6458 = TOROIDAL_SURFACE ( 'NONE', #24160, 2.750000000000000444, 0.05000000000000000278 ) ;
#6459 = EDGE_CURVE ( 'NONE', #12851, #18483, #25872, .T. ) ;
#6460 = CARTESIAN_POINT ( 'NONE',  ( -57.22499999999997300, 0.8236752438352032968, -4.016411220566568296 ) ) ;
#6461 = DIRECTION ( 'NONE',  ( -1.000000000000000000, 0.000000000000000000, 1.047444401652940007E-14 ) ) ;
#6462 = AXIS2_PLACEMENT_3D ( 'NONE', #24159, #28901, #4195 ) ;
#6463 = VECTOR ( 'NONE', #29007, 1000.000000000000000 ) ;
#6464 = CARTESIAN_POINT ( 'NONE',  ( -56.88452994616205416, -3.117691453623976816, 1.799999999999785993 ) ) ;
#6465 = DIRECTION ( 'NONE',  ( 0.000000000000000000, 0.2008964009354147207, -0.9796124928211139560 ) ) ;
#6466 = AXIS2_PLACEMENT_3D ( 'NONE', #21868, #22171, #22007 ) ;
#6467 = AXIS2_PLACEMENT_3D ( 'NONE', #21315, #16711, #2122 ) ;
#6468 = CARTESIAN_POINT ( 'NONE',  ( -58.11042740578360366, 3.725040285533373741, -1.239922660687669209 ) ) ;
#6469 = AXIS2_PLACEMENT_3D ( 'NONE', #4857, #9479, #14042 ) ;
#6470 = CARTESIAN_POINT ( 'NONE',  ( -55.92306624327023457, -3.399999999999986589, -0.9110272542660333706 ) ) ;
#6471 = LINE ( 'NONE', #16128, #19540 ) ;
#6472 = CARTESIAN_POINT ( 'NONE',  ( 52.59308920433354473, 4.500431172231105670, 1.566000610716282271 ) ) ;
#6473 = CARTESIAN_POINT ( 'NONE',  ( 48.40000000000002700, 0.6462379109121004772, -4.048750000000028493 ) ) ;
#6474 = ORIENTED_EDGE ( 'NONE', *, *, #20748, .F. ) ;
#6475 = ADVANCED_FACE ( 'NONE', ( #15892 ), #2276, .F. ) ;
#6476 = CARTESIAN_POINT ( 'NONE',  ( -56.97099364905386665, -3.399999999999994138, 0.9110272542655981631 ) ) ;
#6477 = VERTEX_POINT ( 'NONE', #18446 ) ;
#6479 = CARTESIAN_POINT ( 'NONE',  ( 58.45000000000001705, 0.000000000000000000, 0.000000000000000000 ) ) ;
#6478 = CARTESIAN_POINT ( 'NONE',  ( 48.46244267249164039, 1.426738769040801769, 3.843750315111145621 ) ) ;
#6480 = ORIENTED_EDGE ( 'NONE', *, *, #14822, .F. ) ;
#6481 = CARTESIAN_POINT ( 'NONE',  ( 53.91582462592150193, 6.672259099522118042, -0.8960560664367791528 ) ) ;
#6482 = CARTESIAN_POINT ( 'NONE',  ( 51.25000000000002842, -1.099999999999459410, -1.001327244211406953 ) ) ;
#6484 = CARTESIAN_POINT ( 'NONE',  ( -59.29999999999997584, 0.7533615035078071731, -3.673546848079177529 ) ) ;
#6483 = CARTESIAN_POINT ( 'NONE',  ( 58.45000000000001705, -0.7500000000000000000, -1.778341924377873751 ) ) ;
#6485 = EDGE_LOOP ( 'NONE', ( #17135, #21062, #12411 ) ) ;
#6486 = CARTESIAN_POINT ( 'NONE',  ( -57.61042740578359656, -2.936324665650201116, -2.606018187048497747 ) ) ;
#6487 = CARTESIAN_POINT ( 'NONE',  ( -36.79682133506352670, 3.614202567155919255, 4.024415706308089646 ) ) ;
#6488 = CIRCLE ( 'NONE', #20140, 0.05000000000000012768 ) ;
#6489 = ADVANCED_FACE ( 'NONE', ( #20824 ), #16542, .F. ) ;
#6490 = CARTESIAN_POINT ( 'NONE',  ( 51.80000000000001137, 4.350000000000017408, -1.550321101314903194 ) ) ;
#6491 = CARTESIAN_POINT ( 'NONE',  ( 51.90000000000001279, -1.084202172485504434E-16, 4.374999999999999112 ) ) ;
#6492 = CARTESIAN_POINT ( 'NONE',  ( -62.09999999999998010, -2.687391533643786801, 0.2606275981160442456 ) ) ;
#6493 = ORIENTED_EDGE ( 'NONE', *, *, #7831, .T. ) ;
#6494 = DIRECTION ( 'NONE',  ( 0.000000000000000000, 0.9996898646859345705, 0.02490330187381124133 ) ) ;
#6495 = ORIENTED_EDGE ( 'NONE', *, *, #13708, .F. ) ;
#6496 = CARTESIAN_POINT ( 'NONE',  ( 61.25000000000001421, 1.000000000000641709, -1.655766640117574795 ) ) ;
#6497 = CARTESIAN_POINT ( 'NONE',  ( -59.39321376305881728, 3.357136383570068272, 1.250136525132546916 ) ) ;
#6498 = DIRECTION ( 'NONE',  ( 0.000000000000000000, 0.000000000000000000, -1.000000000000000000 ) ) ;
#6499 = EDGE_CURVE ( 'NONE', #8955, #25147, #11002, .T. ) ;
#6500 = CARTESIAN_POINT ( 'NONE',  ( 15.59055531549694074, -0.9785522574021975339, -5.318456145981289573 ) ) ;
#6502 = FACE_OUTER_BOUND ( 'NONE', #694, .T. ) ;
#6501 = CARTESIAN_POINT ( 'NONE',  ( 33.47623932017462778, 2.199885893005919968, 4.939696249117695892 ) ) ;
#6503 = AXIS2_PLACEMENT_3D ( 'NONE', #28358, #11579, #14097 ) ;
#6504 = CARTESIAN_POINT ( 'NONE',  ( 47.44367304408061869, -4.328087698693956931, -1.560456010858677356 ) ) ;
#6506 = CARTESIAN_POINT ( 'NONE',  ( -59.64494627086173040, 2.036191742483342448, 1.711547443303939264 ) ) ;
#6505 = DIRECTION ( 'NONE',  ( -1.000000000000000000, -0.000000000000000000, -0.000000000000000000 ) ) ;
#6507 = VERTEX_POINT ( 'NONE', #25551 ) ;
#6508 = CIRCLE ( 'NONE', #1969, 3.300781342844381072 ) ;
#6509 = EDGE_CURVE ( 'NONE', #30058, #6673, #14082, .T. ) ;
#6510 = DIRECTION ( 'NONE',  ( 0.7071067811865455743, 7.406550393246774337E-15, 0.7071067811865493491 ) ) ;
#6511 = EDGE_CURVE ( 'NONE', #21983, #12582, #5700, .T. ) ;
#6512 = CARTESIAN_POINT ( 'NONE',  ( 15.03925126672132961, 1.793057972834757541, 4.026191436120407197 ) ) ;
#6514 = CARTESIAN_POINT ( 'NONE',  ( 58.75000000000004263, -2.008165151418633165, 0.5380862305909606125 ) ) ;
#6513 = CARTESIAN_POINT ( 'NONE',  ( 22.54717926605044198, 7.740376438784147162, -1.425000000000078204 ) ) ;
#6516 = ADVANCED_FACE ( 'NONE', ( #21784 ), #17016, .F. ) ;
#6515 = CARTESIAN_POINT ( 'NONE',  ( 51.29335235176148444, 1.002608958138273554, -1.584424273060082378 ) ) ;
#6517 = ORIENTED_EDGE ( 'NONE', *, *, #13276, .T. ) ;
#6518 = CARTESIAN_POINT ( 'NONE',  ( 52.16611735465127708, 8.588510181879298599, 2.049999999999818190 ) ) ;
#6519 = DIRECTION ( 'NONE',  ( 0.7071067811865484609, 0.1420552074174031565, -0.6926906366088668721 ) ) ;
#6520 = ORIENTED_EDGE ( 'NONE', *, *, #16270, .F. ) ;
#6521 = CARTESIAN_POINT ( 'NONE',  ( -54.49999999999996447, -1.399999999999979039, -3.959797974644881258 ) ) ;
#6522 = EDGE_LOOP ( 'NONE', ( #5031, #9393, #7409, #12142 ) ) ;
#6523 = CARTESIAN_POINT ( 'NONE',  ( -59.69999999999996732, -1.873569517744609447, -3.074042495181142698 ) ) ;
#6524 = ORIENTED_EDGE ( 'NONE', *, *, #14724, .T. ) ;
#6525 = CARTESIAN_POINT ( 'NONE',  ( -54.46614378277664059, -2.255560380866761250, -2.805788190199900889 ) ) ;
#6526 = EDGE_CURVE ( 'NONE', #11900, #16762, #4970, .T. ) ;
#6527 = CARTESIAN_POINT ( 'NONE',  ( -56.83155989232414385, -1.962990915244731571, 3.399999999999789413 ) ) ;
#6528 = EDGE_LOOP ( 'NONE', ( #12930, #12887, #23737, #23974, #21927 ) ) ;
#6529 = SURFACE_STYLE_USAGE ( .BOTH. , #28526 ) ;
#6530 = ORIENTED_EDGE ( 'NONE', *, *, #9032, .T. ) ;
#6531 = EDGE_LOOP ( 'NONE', ( #5201, #2281, #21691, #24953 ) ) ;
#6532 = AXIS2_PLACEMENT_3D ( 'NONE', #2555, #623, #10283 ) ;
#6533 = CARTESIAN_POINT ( 'NONE',  ( -54.94702994616205416, 4.156921938165313080, -1.801810997602979365E-13 ) ) ;
#6534 = CARTESIAN_POINT ( 'NONE',  ( -54.89405989232412963, 2.944486372867106461, -1.700000000000182254 ) ) ;
#6535 = CARTESIAN_POINT ( 'NONE',  ( 68.00000000000004263, -0.7500000000000000000, 1.988246715072645943 ) ) ;
#6536 = DIRECTION ( 'NONE',  ( 1.000000000000000000, -0.000000000000000000, -0.000000000000000000 ) ) ;
#6537 = EDGE_CURVE ( 'NONE', #30937, #125, #19082, .T. ) ;
#6538 = LINE ( 'NONE', #27761, #30206 ) ;
#6539 = EDGE_CURVE ( 'NONE', #6201, #6507, #21456, .T. ) ;
#6540 = CARTESIAN_POINT ( 'NONE',  ( -36.72207054450174724, 4.892019442464198953, -2.306425897665967728 ) ) ;
#6541 = CIRCLE ( 'NONE', #12114, 2.374999999999998668 ) ;
#6542 = DIRECTION ( 'NONE',  ( -0.9993908270190956511, 0.03489949670250202390, 3.491481338843132961E-15 ) ) ;
#6543 = CARTESIAN_POINT ( 'NONE',  ( -35.85663232820584057, 3.056483311920803025, 4.206888370749761741 ) ) ;
#6544 = CARTESIAN_POINT ( 'NONE',  ( 15.61033468494287391, 5.277035221755904892, -1.205525476379225136 ) ) ;
#6545 = DIRECTION ( 'NONE',  ( -1.000000000000000000, -0.000000000000000000, -0.000000000000000000 ) ) ;
#6547 = VECTOR ( 'NONE', #10908, 1000.000000000000000 ) ;
#6546 = CARTESIAN_POINT ( 'NONE',  ( 48.40000000000001990, 2.428612866367529932E-14, 0.000000000000000000 ) ) ;
#6548 = EDGE_CURVE ( 'NONE', #19690, #21812, #16165, .T. ) ;
#6549 = LINE ( 'NONE', #4315, #11807 ) ;
#6550 = ORIENTED_EDGE ( 'NONE', *, *, #25868, .T. ) ;
#6552 = DIRECTION ( 'NONE',  ( 1.000000000000000000, 1.047444401652940007E-14, 0.000000000000000000 ) ) ;
#6551 = CARTESIAN_POINT ( 'NONE',  ( 51.13858604272873976, -1.070913481528389166, -1.222302725805714640 ) ) ;
#6553 = EDGE_CURVE ( 'NONE', #23458, #16137, #16707, .T. ) ;
#6554 = AXIS2_PLACEMENT_3D ( 'NONE', #28478, #26097, #24040 ) ;
#6555 = ORIENTED_EDGE ( 'NONE', *, *, #3740, .T. ) ;
#6556 = LINE ( 'NONE', #20672, #16938 ) ;
#6557 = DIRECTION ( 'NONE',  ( -1.047444401652940007E-14, 0.000000000000000000, -1.000000000000000000 ) ) ;
#6558 = CARTESIAN_POINT ( 'NONE',  ( -54.94702994616205416, 4.156921938165313080, -1.801810997602979365E-13 ) ) ;
#6559 = VERTEX_POINT ( 'NONE', #2444 ) ;
#6560 = ORIENTED_EDGE ( 'NONE', *, *, #3561, .T. ) ;
#6561 = DIRECTION ( 'NONE',  ( -2.581436205204234499E-16, 0.9796124928211140670, 0.2008964009354147762 ) ) ;
#6562 = ORIENTED_EDGE ( 'NONE', *, *, #3891, .F. ) ;
#6563 = CIRCLE ( 'NONE', #13606, 1.000000000000000000 ) ;
#6564 = CARTESIAN_POINT ( 'NONE',  ( 58.65000000000004121, -1.671477153793470727, 0.8495817349404540808 ) ) ;
#6565 = DIRECTION ( 'NONE',  ( -1.000000000000000000, -0.000000000000000000, 3.491481338843133355E-15 ) ) ;
#6566 = ORIENTED_EDGE ( 'NONE', *, *, #9072, .F. ) ;
#6567 = CARTESIAN_POINT ( 'NONE',  ( 51.70000000000001705, -3.826179070414207573, -1.000000000000000000 ) ) ;
#6568 = CARTESIAN_POINT ( 'NONE',  ( 58.65000000000003411, -1.874116925334127881, -0.06656272211242116044 ) ) ;
#6569 = DIRECTION ( 'NONE',  ( -0.9977167620779626711, 0.06753712067201277092, 8.270911865460929665E-18 ) ) ;
#6570 = ORIENTED_EDGE ( 'NONE', *, *, #5788, .F. ) ;
#6571 = EDGE_LOOP ( 'NONE', ( #2028, #8639, #1491, #20747, #4328, #10607, #22377, #5105, #28423, #19541 ) ) ;
#6572 =( BOUNDED_SURFACE ( )  B_SPLINE_SURFACE ( 3, 2, ( 
 ( #29607, #13144, #10923 ),
 ( #3027, #20304, #25012 ),
 ( #12671, #22352, #15833 ),
 ( #13282, #27401, #25341 ),
 ( #8095, #3340, #20615 ),
 ( #18078, #22971, #27722 ),
 ( #17604, #12819, #643 ),
 ( #17907, #17762, #8551 ),
 ( #29933, #5711, #15691 ),
 ( #27547, #15363, #19972 ),
 ( #10303, #27248, #5565 ),
 ( #12992, #3502, #1260 ),
 ( #1120, #10625, #30245 ),
 ( #6041, #18235, #27870 ),
 ( #15214, #24860, #22831 ),
 ( #22677, #6188, #974 ) ),
 .UNSPECIFIED., .F., .F., .F. ) 
 B_SPLINE_SURFACE_WITH_KNOTS ( ( 4, 2, 2, 2, 2, 2, 2, 4 ),
 ( 3, 3 ),
 ( 0.001780502285214199260, 0.002558945925323781977, 0.002753556835351177439, 0.002948167745378572902, 0.003337389565433364260, 0.003726611385488155619, 0.004115833205542946543, 0.004894276845652529261 ),
 ( 0.000000000000000000, 1.000000000000000000 ),
 .UNSPECIFIED. ) 
 GEOMETRIC_REPRESENTATION_ITEM ( )  RATIONAL_B_SPLINE_SURFACE ( (
 ( 1.000000000000000000, 0.9418517008537227175, 1.000000000000000000),
 ( 1.000000000000000000, 0.9417987965884856427, 1.000000000000000000),
 ( 1.000000000000000000, 0.9418198861734362604, 1.000000000000000000),
 ( 1.000000000000000000, 0.9434060303845490658, 1.000000000000000000),
 ( 1.000000000000000000, 0.9437939819948191200, 1.000000000000000000),
 ( 1.000000000000000000, 0.9445989566712758023, 1.000000000000000000),
 ( 1.000000000000000000, 0.9450169930049898692, 1.000000000000000000),
 ( 1.000000000000000000, 0.9461610507673464676, 1.000000000000000000),
 ( 1.000000000000000000, 0.9467217966427202702, 1.000000000000000000),
 ( 1.000000000000000000, 0.9467345476124352510, 1.000000000000000000),
 ( 1.000000000000000000, 0.9461964028052861631, 1.000000000000000000),
 ( 1.000000000000000000, 0.9446801822473912535, 1.000000000000000000),
 ( 1.000000000000000000, 0.9437582546536892325, 1.000000000000000000),
 ( 1.000000000000000000, 0.9418129560294941083, 1.000000000000000000),
 ( 1.000000000000000000, 0.9418016889778025869, 1.000000000000000000),
 ( 1.000000000000000000, 0.9418517008537231616, 1.000000000000000000) ) ) 
 REPRESENTATION_ITEM ( '' )  SURFACE ( )  );
#6573 = CARTESIAN_POINT ( 'NONE',  ( 46.92075145057400931, -4.254543194710153742, -1.020305229671234937 ) ) ;
#6574 = CARTESIAN_POINT ( 'NONE',  ( -55.68749999999999289, 1.962990915244720691, 3.399999999999810285 ) ) ;
#6575 = CARTESIAN_POINT ( 'NONE',  ( -64.28602961791190751, -2.263268244922574279, -0.05638033785850377760 ) ) ;
#6576 = CARTESIAN_POINT ( 'NONE',  ( 58.65000000000001279, 0.5811678240972328879, 1.782657835995121287 ) ) ;
#6577 = EDGE_CURVE ( 'NONE', #22982, #14560, #14773, .T. ) ;
#6578 = DIRECTION ( 'NONE',  ( 0.000000000000000000, -1.000000000000000000, 0.000000000000000000 ) ) ;
#6579 = EDGE_CURVE ( 'NONE', #9403, #6667, #4652, .T. ) ;
#6580 = VECTOR ( 'NONE', #28443, 1000.000000000000000 ) ;
#6581 = LINE ( 'NONE', #25887, #6035 ) ;
#6582 = EDGE_CURVE ( 'NONE', #1060, #16210, #21260, .T. ) ;
#6583 = CARTESIAN_POINT ( 'NONE',  ( 57.04037853559506743, 0.7490840064628494499, -1.779165039991060571 ) ) ;
#6585 = CARTESIAN_POINT ( 'NONE',  ( 58.72427158855742135, -0.8981388483288218483, 1.646019958200248157 ) ) ;
#6584 = CARTESIAN_POINT ( 'NONE',  ( 58.66122389686788807, -0.5174758696799709456, -1.802487374212213167 ) ) ;
#6586 = AXIS2_PLACEMENT_3D ( 'NONE', #12108, #13988, #7200 ) ;
#6587 = CARTESIAN_POINT ( 'NONE',  ( -73.90999999999998238, -2.438578184542714499E-15, 4.609931582023435380E-15 ) ) ;
#6588 = CARTESIAN_POINT ( 'NONE',  ( -56.12499999999997868, 2.489203624310595497, -2.804704140674914470 ) ) ;
#6589 = LINE ( 'NONE', #6902, #2653 ) ;
#6590 = LINE ( 'NONE', #3894, #26627 ) ;
#6591 = ORIENTED_EDGE ( 'NONE', *, *, #25600, .F. ) ;
#6592 = ORIENTED_EDGE ( 'NONE', *, *, #23511, .T. ) ;
#6593 = ORIENTED_EDGE ( 'NONE', *, *, #8216, .F. ) ;
#6594 = CARTESIAN_POINT ( 'NONE',  ( 51.67089510066356439, -3.772469189071185003, 1.610667359469496240 ) ) ;
#6595 = ORIENTED_EDGE ( 'NONE', *, *, #10298, .F. ) ;
#6596 = CARTESIAN_POINT ( 'NONE',  ( 52.09213388422766400, 8.600000000000108002, 1.949999998429079895 ) ) ;
#6597 = CARTESIAN_POINT ( 'NONE',  ( -56.78335481156722864, -4.108500314926510022, 1.367561758111407455 ) ) ;
#6599 = FACE_OUTER_BOUND ( 'NONE', #21055, .T. ) ;
#6598 = CARTESIAN_POINT ( 'NONE',  ( 52.20711756518984714, -0.6499999999994533484, 1.489337100860647967 ) ) ;
#6600 = ORIENTED_EDGE ( 'NONE', *, *, #7794, .T. ) ;
#6601 = CARTESIAN_POINT ( 'NONE',  ( 31.33115571983777770, 7.478201237066244289, -2.050000000000108180 ) ) ;
#6602 = ORIENTED_EDGE ( 'NONE', *, *, #17242, .T. ) ;
#6603 = CARTESIAN_POINT ( 'NONE',  ( -62.39999999999998437, 1.076401154667962023E-15, 2.259002067258145746E-15 ) ) ;
#6604 = VERTEX_POINT ( 'NONE', #15244 ) ;
#6606 = DIRECTION ( 'NONE',  ( 2.459562394685744772E-16, -0.9510565162951523099, -0.3090169943749515591 ) ) ;
#6605 = CARTESIAN_POINT ( 'NONE',  ( 58.45000000000001705, -0.8000000000000000444, 2.421260002560649660 ) ) ;
#6607 = ORIENTED_EDGE ( 'NONE', *, *, #21461, .T. ) ;
#6608 = CARTESIAN_POINT ( 'NONE',  ( -35.85663232820584057, 0.9159215771380343485, -4.311190327365813424 ) ) ;
#6609 = CARTESIAN_POINT ( 'NONE',  ( 58.74999999999999289, 1.834410884276637566, -0.3880228184651508538 ) ) ;
#6610 = AXIS2_PLACEMENT_3D ( 'NONE', #2534, #17105, #2678 ) ;
#6611 = DIRECTION ( 'NONE',  ( 0.000000000000000000, 0.000000000000000000, 1.000000000000000000 ) ) ;
#6612 = CARTESIAN_POINT ( 'NONE',  ( 50.25000000000002132, 5.263408118306026973E-13, 3.111507638930570854E-58 ) ) ;
#6613 = CARTESIAN_POINT ( 'NONE',  ( -59.63452994616203284, 2.093608279459373297E-14, -3.600000000000211475 ) ) ;
#6614 = LINE ( 'NONE', #9308, #10951 ) ;
#6615 = EDGE_CURVE ( 'NONE', #11900, #21791, #1008, .T. ) ;
#6616 = EDGE_CURVE ( 'NONE', #13291, #25147, #26793, .T. ) ;
#6617 = CARTESIAN_POINT ( 'NONE',  ( 57.05000000000001847, 0.8000000000000000444, 2.421260002560649660 ) ) ;
#6618 = CARTESIAN_POINT ( 'NONE',  ( 50.49738912176885464, 0.9335627837658418970, -3.994936164801341061 ) ) ;
#6619 = CARTESIAN_POINT ( 'NONE',  ( -56.92292740578359656, -3.330682475591782765, -0.6830477631804132699 ) ) ;
#6620 = CARTESIAN_POINT ( 'NONE',  ( -55.70655989232411542, 1.962990915244752888, -3.400000000000186873 ) ) ;
#6621 = CIRCLE ( 'NONE', #3836, 2.374999999999998668 ) ;
#6622 = ORIENTED_EDGE ( 'NONE', *, *, #22288, .T. ) ;
#6623 = CARTESIAN_POINT ( 'NONE',  ( 46.90000000000001279, 1.734723475976807094E-15, 0.000000000000000000 ) ) ;
#6624 = CARTESIAN_POINT ( 'NONE',  ( -59.63452994616203284, 2.710830266229639327E-14, -3.600000000000211475 ) ) ;
#6625 = CARTESIAN_POINT ( 'NONE',  ( -36.56390771145571961, -0.2088129849843483599, 5.405094643512490471 ) ) ;
#6626 = CARTESIAN_POINT ( 'NONE',  ( 48.40000000000002700, 0.6304760106459513791, -3.950000000000022826 ) ) ;
#6627 = ORIENTED_EDGE ( 'NONE', *, *, #6438, .T. ) ;
#6628 = EDGE_CURVE ( 'NONE', #18794, #11503, #28829, .T. ) ;
#6629 = ORIENTED_EDGE ( 'NONE', *, *, #8145, .T. ) ;
#6630 = DIRECTION ( 'NONE',  ( -2.459562394685737870E-16, 0.9510565162951500895, 0.3090169943749582204 ) ) ;
#6632 = CARTESIAN_POINT ( 'NONE',  ( 58.75000000000004263, -2.008165151418373373, -0.5380862305909229759 ) ) ;
#6631 = CARTESIAN_POINT ( 'NONE',  ( -77.29999999999998295, -3.473832742311974792E-15, 5.302342620690189014E-15 ) ) ;
#6633 = VERTEX_POINT ( 'NONE', #15566 ) ;
#6634 = ORIENTED_EDGE ( 'NONE', *, *, #13644, .T. ) ;
#6635 = CYLINDRICAL_SURFACE ( 'NONE', #8801, 3.625000000000000444 ) ;
#6636 = CARTESIAN_POINT ( 'NONE',  ( 50.25000000000002842, -1.039502773796191937, -1.650471618824325359 ) ) ;
#6638 = DIRECTION ( 'NONE',  ( -1.000000000000000000, 0.000000000000000000, -3.491481338843153471E-15 ) ) ;
#6637 = DIRECTION ( 'NONE',  ( 0.000000000000000000, 0.000000000000000000, -1.000000000000000000 ) ) ;
#6639 = ORIENTED_EDGE ( 'NONE', *, *, #16474, .F. ) ;
#6640 = CARTESIAN_POINT ( 'NONE',  ( -56.56249999999997158, -0.8699069336946623210, 4.241846523238426592 ) ) ;
#6641 = DIRECTION ( 'NONE',  ( 1.003947306782822575E-14, 0.000000000000000000, 1.000000000000000000 ) ) ;
#6642 = COLOUR_RGB ( '', 0.31764706, 0.68627451, 0.89019608) ;
#6643 = SHAPE_DEFINITION_REPRESENTATION ( #17390, #30888 ) ;
#6644 = CARTESIAN_POINT ( 'NONE',  ( 61.25000000000002132, 6.415596960124259844E-13, 3.111507638930570854E-58 ) ) ;
#6645 = FACE_OUTER_BOUND ( 'NONE', #28908, .T. ) ;
#6646 = DIRECTION ( 'NONE',  ( -1.000000000000000000, 0.000000000000000000, -0.000000000000000000 ) ) ;
#6647 = VERTEX_POINT ( 'NONE', #27115 ) ;
#6648 = EDGE_CURVE ( 'NONE', #12844, #29437, #15171, .T. ) ;
#6649 = CARTESIAN_POINT ( 'NONE',  ( 57.00000000000001421, -0.7059996929583092218, 1.815412393553804460 ) ) ;
#6650 = CARTESIAN_POINT ( 'NONE',  ( -36.56390771145525775, 3.345968172200181279, -4.250076229745598511 ) ) ;
#6651 = CARTESIAN_POINT ( 'NONE',  ( 58.65000000000003411, -1.589751505945435239, -0.9947034709617927906 ) ) ;
#6652 = EDGE_CURVE ( 'NONE', #21568, #1882, #8175, .T. ) ;
#6653 = CARTESIAN_POINT ( 'NONE',  ( -69.22071067811863543, -6.995007661688606141E-16, 2.451642053546763754E-15 ) ) ;
#6654 = CIRCLE ( 'NONE', #9198, 0.1000000000000002970 ) ;
#6656 = CARTESIAN_POINT ( 'NONE',  ( 58.74154451056428883, -1.784780193103109092, -0.5746581230773456506 ) ) ;
#6655 = CARTESIAN_POINT ( 'NONE',  ( 58.45000000000001705, 0.8156862745098041323, 2.468735688885368873 ) ) ;
#6657 = DIRECTION ( 'NONE',  ( -0.000000000000000000, -0.000000000000000000, -1.000000000000000000 ) ) ;
#6659 = CARTESIAN_POINT ( 'NONE',  ( -59.63444153017528748, 2.031330036680259354, 1.710319191226306712 ) ) ;
#6658 = CARTESIAN_POINT ( 'NONE',  ( 34.50000000000001421, 0.000000000000000000, 0.000000000000000000 ) ) ;
#6660 = ORIENTED_EDGE ( 'NONE', *, *, #13138, .T. ) ;
#6661 = VECTOR ( 'NONE', #4387, 1000.000000000000000 ) ;
#6662 = CARTESIAN_POINT ( 'NONE',  ( 58.75000000000002132, 6.153735859711025284E-13, 3.111507638930570854E-58 ) ) ;
#6663 = CARTESIAN_POINT ( 'NONE',  ( 51.70000000000001705, 3.851905453475298113, -1.404572667215154835 ) ) ;
#6665 = CARTESIAN_POINT ( 'NONE',  ( -36.30424252565904197, 4.911231426340481931, 1.712337380313478707 ) ) ;
#6664 = CARTESIAN_POINT ( 'NONE',  ( -57.77499999999997016, 0.9743475445367644205, -4.751120590182402736 ) ) ;
#6666 = CARTESIAN_POINT ( 'NONE',  ( 15.56401610563846027, -4.735424960531449123, 2.618558234550369956 ) ) ;
#6667 = VERTEX_POINT ( 'NONE', #22856 ) ;
#6668 = VERTEX_POINT ( 'NONE', #19848 ) ;
#6669 = CARTESIAN_POINT ( 'NONE',  ( -36.48821680285229974, -5.256402525809805049, 1.287848407636970061 ) ) ;
#6670 = CARTESIAN_POINT ( 'NONE',  ( -54.39999999999999147, 1.399999999999996136, 3.959797974644420737 ) ) ;
#6671 = EDGE_LOOP ( 'NONE', ( #29685, #5707, #3053, #672 ) ) ;
#6672 = CARTESIAN_POINT ( 'NONE',  ( 58.73868664959847052, 0.5000000000006151746, 1.844330893389497072 ) ) ;
#6673 = VERTEX_POINT ( 'NONE', #25213 ) ;
#6674 = FACE_OUTER_BOUND ( 'NONE', #22562, .T. ) ;
#6675 = ORIENTED_EDGE ( 'NONE', *, *, #25846, .T. ) ;
#6676 = CARTESIAN_POINT ( 'NONE',  ( -56.89405989232413674, -3.920666489018330156E-15, 3.399999999999796962 ) ) ;
#6677 = ORIENTED_EDGE ( 'NONE', *, *, #6790, .F. ) ;
#6678 =( NAMED_UNIT ( * ) PLANE_ANGLE_UNIT ( ) SI_UNIT ( $, .RADIAN. ) );
#6679 = ORIENTED_EDGE ( 'NONE', *, *, #26346, .F. ) ;
#6680 = CIRCLE ( 'NONE', #24378, 0.04999999999999969746 ) ;
#6681 = ORIENTED_EDGE ( 'NONE', *, *, #12126, .F. ) ;
#6682 = EDGE_CURVE ( 'NONE', #3316, #29446, #28309, .T. ) ;
#6683 = CARTESIAN_POINT ( 'NONE',  ( -54.63452994616206126, -3.117691453623976816, 1.799999999999793765 ) ) ;
#6684 = EDGE_CURVE ( 'NONE', #25704, #2692, #20751, .T. ) ;
#6685 = CARTESIAN_POINT ( 'NONE',  ( 58.45000000000001705, -0.7794871794871796045, 1.732743413496389939 ) ) ;
#6686 = CARTESIAN_POINT ( 'NONE',  ( 58.75000000000002132, 6.153735859711025284E-13, 3.111507638930570854E-58 ) ) ;
#6688 = EDGE_CURVE ( 'NONE', #247, #23319, #20232, .T. ) ;
#6687 = DIRECTION ( 'NONE',  ( -1.282749433769087582E-30, 1.000000000000000000, -1.224646799147353207E-16 ) ) ;
#6689 = CARTESIAN_POINT ( 'NONE',  ( 61.25000000000002132, 0.8718791990819803051, 1.626461527140064423 ) ) ;
#6691 = CARTESIAN_POINT ( 'NONE',  ( -57.81249999999997158, -3.238593381231830381, -2.874284765127031793 ) ) ;
#6690 = DIRECTION ( 'NONE',  ( -1.000000000000000000, -3.054025858079668409E-16, 2.042474015755241579E-16 ) ) ;
#6692 = CIRCLE ( 'NONE', #6197, 0.2000000000000000944 ) ;
#6693 =( NAMED_UNIT ( * ) SI_UNIT ( $, .STERADIAN. ) SOLID_ANGLE_UNIT ( ) );
#6694 = DIRECTION ( 'NONE',  ( 0.000000000000000000, 0.000000000000000000, -1.000000000000000000 ) ) ;
#6695 = LINE ( 'NONE', #14289, #31170 ) ;
#6696 = CARTESIAN_POINT ( 'NONE',  ( 56.95606009725792518, 0.7486802684473473635, 2.489875068279050918 ) ) ;
#6697 = EDGE_CURVE ( 'NONE', #5233, #20006, #1391, .T. ) ;
#6698 = DIRECTION ( 'NONE',  ( 1.000000000000000000, -0.000000000000000000, -0.000000000000000000 ) ) ;
#6699 = CARTESIAN_POINT ( 'NONE',  ( 51.25000000000001421, 1.163569835200988601E-28, -1.789384186157106949E-13 ) ) ;
#6700 = ORIENTED_EDGE ( 'NONE', *, *, #9300, .T. ) ;
#6702 = CARTESIAN_POINT ( 'NONE',  ( 48.43364830228694018, -1.250438735127598955, -3.874838289045730910 ) ) ;
#6701 = DIRECTION ( 'NONE',  ( 0.000000000000000000, 0.000000000000000000, -1.000000000000000000 ) ) ;
#6703 = DIRECTION ( 'NONE',  ( 1.000000000000000000, 1.047444401652940007E-14, 0.000000000000000000 ) ) ;
#6704 = ORIENTED_EDGE ( 'NONE', *, *, #7271, .F. ) ;
#6705 = DIRECTION ( 'NONE',  ( -3.489354422748178582E-15, 1.218509414717996338E-16, -1.000000000000000000 ) ) ;
#6706 = CARTESIAN_POINT ( 'NONE',  ( -60.37499999999995737, 2.944486372867106905, -1.700000000000201794 ) ) ;
#6707 = ORIENTED_EDGE ( 'NONE', *, *, #10930, .F. ) ;
#6708 = ADVANCED_FACE ( 'NONE', ( #27748 ), #18570, .T. ) ;
#6709 = ORIENTED_EDGE ( 'NONE', *, *, #25661, .T. ) ;
#6710 = CARTESIAN_POINT ( 'NONE',  ( 69.20000000000000284, -0.8382352941176473005, -2.222158093318006067 ) ) ;
#6711 = VERTEX_POINT ( 'NONE', #23315 ) ;
#6712 = CARTESIAN_POINT ( 'NONE',  ( 58.74999981404335614, -1.649595783783118774, 1.050697058759348934 ) ) ;
#6713 = CARTESIAN_POINT ( 'NONE',  ( 54.19030381964616083, 6.697848500921247172, -2.050000000000189004 ) ) ;
#6714 = ORIENTED_EDGE ( 'NONE', *, *, #24173, .F. ) ;
#6715 = CARTESIAN_POINT ( 'NONE',  ( -62.04999999999998295, 2.699162634652024106, 0.06723891505929237289 ) ) ;
#6716 =( BOUNDED_CURVE ( )  B_SPLINE_CURVE ( 2, ( #29691, #2780, #12432, #24630, #27320, #5479, #7835, #17350, #563 ),
 .UNSPECIFIED., .F., .T. ) 
 B_SPLINE_CURVE_WITH_KNOTS ( ( 3, 2, 2, 2, 3 ),
 ( 0.5277777777777777901, 0.5370370370370370905, 0.5555555555555555802, 0.5740740740740740700, 0.5833333333333333703 ),
 .UNSPECIFIED. ) 
 CURVE ( )  GEOMETRIC_REPRESENTATION_ITEM ( )  RATIONAL_B_SPLINE_CURVE ( ( 0.9330127018922194093, 0.9330127018922194093, 1.000000000000000000, 0.8660254037844387076, 1.000000000000000000, 0.8660254037844387076, 1.000000000000000000, 0.9330127018922189652, 0.9330127018922194093 ) ) 
 REPRESENTATION_ITEM ( '' )  );
#6717 = CARTESIAN_POINT ( 'NONE',  ( 49.05000000000002558, 1.401298464324817071E-42, -5.137714790107672405E-13 ) ) ;
#6718 = CARTESIAN_POINT ( 'NONE',  ( -60.59999999999997300, 1.626093840209163176E-15, 1.891350188320046374E-15 ) ) ;
#6719 = ORIENTED_EDGE ( 'NONE', *, *, #21241, .F. ) ;
#6720 = VERTEX_POINT ( 'NONE', #11259 ) ;
#6721 = EDGE_CURVE ( 'NONE', #16489, #10532, #3493, .T. ) ;
#6722 = DIRECTION ( 'NONE',  ( -1.000000000000000000, 0.000000000000000000, 0.000000000000000000 ) ) ;
#6723 = ADVANCED_FACE ( 'NONE', ( #24835 ), #10969, .T. ) ;
#6724 = CARTESIAN_POINT ( 'NONE',  ( -57.22499999999997300, -0.9241234443029057166, 4.506217466977124886 ) ) ;
#6725 = CARTESIAN_POINT ( 'NONE',  ( 51.45655683570191741, -0.9591657938390835136, 1.468576096419531574 ) ) ;
#6726 = ORIENTED_EDGE ( 'NONE', *, *, #17179, .T. ) ;
#6728 = ADVANCED_FACE ( 'NONE', ( #18492 ), #17194, .T. ) ;
#6727 = LINE ( 'NONE', #14167, #1771 ) ;
#6729 = CARTESIAN_POINT ( 'NONE',  ( 56.95000000000001705, 0.6917305289283675052, 1.769637370168020141 ) ) ;
#6730 = CARTESIAN_POINT ( 'NONE',  ( 58.64999999999999858, 1.760622601996781667, 0.8948927608044729975 ) ) ;
#6731 = CARTESIAN_POINT ( 'NONE',  ( 41.48619405472010868, -151.3359592902261852, 1.424999999999836175 ) ) ;
#6733 = CARTESIAN_POINT ( 'NONE',  ( 58.75000018803720536, -1.010830333486641974, 1.651902078983862321 ) ) ;
#6732 = CARTESIAN_POINT ( 'NONE',  ( -36.21152527658241382, -2.821511581828405557, 4.377605326016305476 ) ) ;
#6734 = DIRECTION ( 'NONE',  ( 0.000000000000000000, 0.000000000000000000, 1.000000000000000000 ) ) ;
#6735 = CARTESIAN_POINT ( 'NONE',  ( 67.99999999999997158, 1.401298464324817071E-42, -4.000000000000712319 ) ) ;
#6736 = DIRECTION ( 'NONE',  ( -3.491481338843133355E-15, -1.216509871872716567E-14, 1.000000000000000000 ) ) ;
#6737 = VECTOR ( 'NONE', #9169, 1000.000000000000000 ) ;
#6738 = VERTEX_POINT ( 'NONE', #30032 ) ;
#6739 = CIRCLE ( 'NONE', #27980, 4.849999999999999645 ) ;
#6740 = ORIENTED_EDGE ( 'NONE', *, *, #20319, .F. ) ;
#6741 = CARTESIAN_POINT ( 'NONE',  ( 51.13341687362841270, 0.9248174436456687575, 1.495576127288423818 ) ) ;
#6742 = VERTEX_POINT ( 'NONE', #6288 ) ;
#6743 = CARTESIAN_POINT ( 'NONE',  ( 54.16075265905998748, 5.605215124043997577, 2.049999999999811084 ) ) ;
#6744 = CARTESIAN_POINT ( 'NONE',  ( -56.09585481156723574, -2.489203624310586616, 2.804704140674918023 ) ) ;
#6746 = CARTESIAN_POINT ( 'NONE',  ( 51.35673058052184103, -3.851351755029094104, -1.408485093545058575 ) ) ;
#6745 = CYLINDRICAL_SURFACE ( 'NONE', #11487, 2.000000000000000000 ) ;
#6747 = ORIENTED_EDGE ( 'NONE', *, *, #21625, .F. ) ;
#6748 = EDGE_CURVE ( 'NONE', #30343, #3572, #9612, .T. ) ;
#6749 = DIRECTION ( 'NONE',  ( 1.000000000000000000, 0.000000000000000000, 0.000000000000000000 ) ) ;
#6750 = ORIENTED_EDGE ( 'NONE', *, *, #1110, .F. ) ;
#6751 = DIRECTION ( 'NONE',  ( 0.000000000000000000, 0.000000000000000000, 1.000000000000000000 ) ) ;
#6752 =( BOUNDED_SURFACE ( )  B_SPLINE_SURFACE ( 3, 2, ( 
 ( #4415, #4098, #26102 ),
 ( #23582, #1558, #9176 ),
 ( #16446, #23423, #18362 ),
 ( #1705, #9008, #14064 ) ),
 .UNSPECIFIED., .F., .F., .F. ) 
 B_SPLINE_SURFACE_WITH_KNOTS ( ( 4, 4 ),
 ( 3, 3 ),
 ( 1.069308579029437212, 1.196413504413466500 ),
 ( 0.000000000000000000, 1.000000000000000000 ),
 .UNSPECIFIED. ) 
 GEOMETRIC_REPRESENTATION_ITEM ( )  RATIONAL_B_SPLINE_SURFACE ( (
 ( 1.000000000000000000, 0.8415238966082415617, 1.000000000000000000),
 ( 1.000000000000000000, 0.8319656872388342395, 1.000000000000000000),
 ( 1.000000000000000000, 0.8219112105083486997, 1.000000000000000000),
 ( 1.000000000000000000, 0.8113889037030929119, 1.000000000000000000) ) ) 
 REPRESENTATION_ITEM ( '' )  SURFACE ( )  );
#6753 = EDGE_LOOP ( 'NONE', ( #28633, #16768, #20848, #28641 ) ) ;
#6755 = PLANE ( 'NONE',  #25149 ) ;
#6754 = LINE ( 'NONE', #21671, #14045 ) ;
#6756 = EDGE_CURVE ( 'NONE', #22777, #7189, #15938, .T. ) ;
#6757 = ORIENTED_EDGE ( 'NONE', *, *, #17649, .F. ) ;
#6758 = CARTESIAN_POINT ( 'NONE',  ( 53.29836137858970346, 7.982254241276255158, 1.892848342821848995 ) ) ;
#6759 = CARTESIAN_POINT ( 'NONE',  ( 58.75000000000000000, 1.922112613535394310, -0.4146634982021765170 ) ) ;
#6760 = CARTESIAN_POINT ( 'NONE',  ( 47.76052902567371916, -4.379874851678566827, 1.406750166670421631 ) ) ;
#6761 = CARTESIAN_POINT ( 'NONE',  ( 56.99137905793185155, 0.7079296279778910517, -1.763407125847052725 ) ) ;
#6763 = CARTESIAN_POINT ( 'NONE',  ( -58.63452994616204705, 3.117691453623979481, 1.799999999999803757 ) ) ;
#6762 = AXIS2_PLACEMENT_3D ( 'NONE', #10644, #662, #3522 ) ;
#6765 = EDGE_CURVE ( 'NONE', #20590, #17963, #6563, .T. ) ;
#6764 = CARTESIAN_POINT ( 'NONE',  ( -59.10063086805173072, -2.465840246036694161, -0.9706348448640983451 ) ) ;
#6766 = CARTESIAN_POINT ( 'NONE',  ( -35.85663232820583346, -4.383220986679497777, 0.4611378927914391301 ) ) ;
#6767 = CARTESIAN_POINT ( 'NONE',  ( -56.34585481156723574, 3.673546848079182858, 0.7533615035078061739 ) ) ;
#6768 = CARTESIAN_POINT ( 'NONE',  ( -56.36042740578360366, -0.7887156198831688503, 3.845940847736172064 ) ) ;
#6769 = DIRECTION ( 'NONE',  ( -1.499696682456171775E-15, 0.9030524935654854479, 0.4295302013423024645 ) ) ;
#6770 = ORIENTED_EDGE ( 'NONE', *, *, #21112, .F. ) ;
#6771 = CYLINDRICAL_SURFACE ( 'NONE', #5913, 0.5000000000000000000 ) ;
#6772 = DIRECTION ( 'NONE',  ( 0.000000000000000000, 0.000000000000000000, 1.000000000000000000 ) ) ;
#6773 = CARTESIAN_POINT ( 'NONE',  ( -36.89250464418362441, -0.3169205264059772320, 5.400007398663888125 ) ) ;
#6774 = DIRECTION ( 'NONE',  ( 0.000000000000000000, 0.3589743589743593088, -0.9333474217026304087 ) ) ;
#6775 = EDGE_LOOP ( 'NONE', ( #28527, #19278, #13329, #25635 ) ) ;
#6776 = CARTESIAN_POINT ( 'NONE',  ( 68.00000000000000000, 0.8382352941176474115, -2.222158093317993632 ) ) ;
#6777 = ORIENTED_EDGE ( 'NONE', *, *, #28050, .F. ) ;
#6778 = DIRECTION ( 'NONE',  ( 0.9993908270190958731, -0.03489949670249358621, -4.336808689942082423E-15 ) ) ;
#6779 = AXIS2_PLACEMENT_3D ( 'NONE', #12653, #20286, #10905 ) ;
#6781 = DIRECTION ( 'NONE',  ( 0.000000000000000000, 0.000000000000000000, 1.000000000000000000 ) ) ;
#6780 = DIRECTION ( 'NONE',  ( 0.000000000000000000, 0.9663289263986323263, -0.2573099415204678220 ) ) ;
#6782 = VERTEX_POINT ( 'NONE', #25765 ) ;
#6783 = EDGE_CURVE ( 'NONE', #7611, #24164, #23772, .T. ) ;
#6784 = ORIENTED_EDGE ( 'NONE', *, *, #304, .T. ) ;
#6785 = B_SPLINE_CURVE_WITH_KNOTS ( 'NONE', 3,
 ( #24559, #26645, #3186, #12827, #4949, #14605, #2581, #10160, #15067, #651, #7946, #24270, #17611, #9853, #27256, #19525 ),
 .UNSPECIFIED., .F., .F.,
 ( 4, 2, 2, 2, 2, 2, 2, 4 ),
 ( 1.734723475976806902E-18, 0.0004351083927046452463, 0.0008702167854092887579, 0.001740433570818576648, 0.002175541963523220865, 0.002610650356227864864, 0.003045758748932509297, 0.003480867141637153730 ),
 .UNSPECIFIED. ) ;
#6786 = LINE ( 'NONE', #30699, #30542 ) ;
#6787 = ADVANCED_FACE ( 'NONE', ( #3463 ), #3540, .T. ) ;
#6788 = CARTESIAN_POINT ( 'NONE',  ( 51.90000000000001279, 1.734723475976807094E-15, 0.000000000000000000 ) ) ;
#6789 = CARTESIAN_POINT ( 'NONE',  ( 58.66107449606931823, -1.349793924521457855, 1.301839550768250753 ) ) ;
#6790 = EDGE_CURVE ( 'NONE', #23830, #24402, #5520, .T. ) ;
#6791 = ORIENTED_EDGE ( 'NONE', *, *, #21208, .F. ) ;
#6792 = CARTESIAN_POINT ( 'NONE',  ( -55.93749999999997868, 3.238593381231845481, 2.874284765127021579 ) ) ;
#6793 = CIRCLE ( 'NONE', #18945, 0.2999999999999999334 ) ;
#6794 = CARTESIAN_POINT ( 'NONE',  ( 15.03925126672133139, -4.683225679163337318, -2.703237727951242508 ) ) ;
#6795 = TOROIDAL_SURFACE ( 'NONE', #22464, 1.975000000000001865, 0.1000000000000000056 ) ;
#6796 = CARTESIAN_POINT ( 'NONE',  ( 69.23535533905935324, 4.557543281186736018E-17, -7.252018534634969470E-13 ) ) ;
#6797 = DIRECTION ( 'NONE',  ( -1.000000000000000000, 0.000000000000000000, 3.491481338843133750E-15 ) ) ;
#6798 = ORIENTED_EDGE ( 'NONE', *, *, #26658, .T. ) ;
#6799 = ADVANCED_FACE ( 'NONE', ( #21025 ), #26236, .T. ) ;
#6800 = CARTESIAN_POINT ( 'NONE',  ( 57.00529107662529782, -0.7231510886217332734, 1.801575813826951533 ) ) ;
#6801 = CARTESIAN_POINT ( 'NONE',  ( -36.92443669619591873, 3.305069970238394994, -4.282766538619357632 ) ) ;
#6802 = DIRECTION ( 'NONE',  ( 1.000000000000000000, 1.047444401652940007E-14, 0.000000000000000000 ) ) ;
#6803 = AXIS2_PLACEMENT_3D ( 'NONE', #19590, #4840, #9292 ) ;
#6804 = CARTESIAN_POINT ( 'NONE',  ( 47.00000000000002132, 6.982261990806648555E-14, -1.628983268085978048E-13 ) ) ;
#6805 = DIRECTION ( 'NONE',  ( 0.000000000000000000, -0.000000000000000000, 1.000000000000000000 ) ) ;
#6807 = DIRECTION ( 'NONE',  ( -0.9993908270190958731, 0.03489949670250096919, 3.491595022110081325E-15 ) ) ;
#6806 = DIRECTION ( 'NONE',  ( 0.000000000000000000, 0.000000000000000000, 1.000000000000000000 ) ) ;
#6808 = PRODUCT_RELATED_PRODUCT_CATEGORY ( 'part', '', ( #16191 ) ) ;
#6809 = CARTESIAN_POINT ( 'NONE',  ( 47.02041791374344371, -4.146195171497997656, -1.996297985640646644 ) ) ;
#6811 = CARTESIAN_POINT ( 'NONE',  ( -63.84999999999997300, -2.699162634652022774, -0.06723891505928747403 ) ) ;
#6810 = LINE ( 'NONE', #2064, #28669 ) ;
#6812 = EDGE_LOOP ( 'NONE', ( #21115, #13090, #6719, #27620 ) ) ;
#6813 = CARTESIAN_POINT ( 'NONE',  ( 51.84772254680353143, 0.6924618999072389425, 1.653428777428159746 ) ) ;
#6814 = DIRECTION ( 'NONE',  ( -1.000000000000000000, 0.000000000000000000, 1.047444401652940007E-14 ) ) ;
#6816 = CARTESIAN_POINT ( 'NONE',  ( -36.63359589171323449, 5.330414537250494966, 0.9106291984479393253 ) ) ;
#6815 = CARTESIAN_POINT ( 'NONE',  ( 15.86395258069112835, -2.563573972737278606, -4.761506352252398599 ) ) ;
#6817 = CARTESIAN_POINT ( 'NONE',  ( 15.48686146417454523, -4.911231426340524564, 1.712337380313389001 ) ) ;
#6818 = AXIS2_PLACEMENT_3D ( 'NONE', #19737, #6913, #26223 ) ;
#6819 = ORIENTED_EDGE ( 'NONE', *, *, #27991, .T. ) ;
#6820 = CIRCLE ( 'NONE', #24510, 0.2500000000000000000 ) ;
#6821 = ORIENTED_EDGE ( 'NONE', *, *, #13887, .T. ) ;
#6822 = CARTESIAN_POINT ( 'NONE',  ( -36.22818246778668083, -4.895960019030552779, 2.323379425334354043 ) ) ;
#6823 = DIRECTION ( 'NONE',  ( -2.459562394685738363E-16, 0.9510565162951500895, 0.3090169943749582759 ) ) ;
#6824 = EDGE_CURVE ( 'NONE', #9750, #24313, #10114, .T. ) ;
#6825 = EDGE_LOOP ( 'NONE', ( #17014, #8090, #2733 ) ) ;
#6826 = CIRCLE ( 'NONE', #8335, 0.4600000000000000755 ) ;
#6827 = DIRECTION ( 'NONE',  ( -1.000000000000000000, -0.000000000000000000, 1.047444401652940007E-14 ) ) ;
#6828 = ORIENTED_EDGE ( 'NONE', *, *, #15834, .F. ) ;
#6829 = CARTESIAN_POINT ( 'NONE',  ( 58.75000000694004854, 1.928945400590568626, 0.02494613115323923019 ) ) ;
#6830 = ORIENTED_EDGE ( 'NONE', *, *, #25732, .T. ) ;
#6831 =( LENGTH_UNIT ( ) NAMED_UNIT ( * ) SI_UNIT ( .MILLI., .METRE. ) );
#6832 = DIRECTION ( 'NONE',  ( 1.000000000000000000, -1.219044193948983948E-29, 3.491481338843133355E-15 ) ) ;
#6833 = ORIENTED_EDGE ( 'NONE', *, *, #10888, .T. ) ;
#6834 = FILL_AREA_STYLE ('',( #4615 ) ) ;
#6835 = CIRCLE ( 'NONE', #30073, 1.599188152294417131 ) ;
#6836 = ORIENTED_EDGE ( 'NONE', *, *, #1905, .T. ) ;
#6837 = PRODUCT_DEFINITION_SHAPE ( 'NONE', 'NONE',  #2956 ) ;
#6838 = ORIENTED_EDGE ( 'NONE', *, *, #23497, .F. ) ;
#6839 = EDGE_CURVE ( 'NONE', #29380, #7998, #7084, .T. ) ;
#6840 = CARTESIAN_POINT ( 'NONE',  ( -60.81249999999997868, -1.962990915244731793, 3.399999999999776090 ) ) ;
#6841 = CARTESIAN_POINT ( 'NONE',  ( 56.95000000000001705, -0.7137254901960785602, 2.500119182087999548 ) ) ;
#6842 = DIRECTION ( 'NONE',  ( -1.000000000000000000, 0.000000000000000000, 1.047444401652940007E-14 ) ) ;
#6843 = PLANE ( 'NONE',  #9912 ) ;
#6844 = TOROIDAL_SURFACE ( 'NONE', #760, 1.975000000000001865, 0.1000000000000000056 ) ;
#6845 = AXIS2_PLACEMENT_3D ( 'NONE', #10027, #5250, #11919 ) ;
#6847 = DIRECTION ( 'NONE',  ( 0.000000000000000000, 1.000000000000000000, -8.673617379884030739E-15 ) ) ;
#6846 = DIRECTION ( 'NONE',  ( 0.000000000000000000, -0.2008964009354147484, 0.9796124928211138450 ) ) ;
#6848 = EDGE_CURVE ( 'NONE', #21838, #596, #7587, .T. ) ;
#6849 = CARTESIAN_POINT ( 'NONE',  ( 47.07338444802540778, -4.179189466084497262, 0.9999999999999988898 ) ) ;
#6850 = CYLINDRICAL_SURFACE ( 'NONE', #4861, 0.2500000000000002220 ) ;
#6851 = AXIS2_PLACEMENT_3D ( 'NONE', #6889, #21325, #16388 ) ;
#6852 = CARTESIAN_POINT ( 'NONE',  ( 15.81621483022862407, 5.330414537250522500, -0.9106291984478636081 ) ) ;
#6853 = EDGE_LOOP ( 'NONE', ( #7710, #24653, #9877, #11549 ) ) ;
#6854 = DIRECTION ( 'NONE',  ( 0.000000000000000000, 0.000000000000000000, 1.000000000000000000 ) ) ;
#6855 = AXIS2_PLACEMENT_3D ( 'NONE', #15685, #28009, #11227 ) ;
#6856 = CARTESIAN_POINT ( 'NONE',  ( 53.56883702301119143, 7.945158945316190824, 2.049999999999813305 ) ) ;
#6857 = B_SPLINE_CURVE_WITH_KNOTS ( 'NONE', 3,
 ( #9067, #1301, #20799, #10971, #20654, #11123 ),
 .UNSPECIFIED., .F., .F.,
 ( 4, 2, 4 ),
 ( 0.000000000000000000, 0.0001000270069606238189, 0.0002000540139212476378 ),
 .UNSPECIFIED. ) ;
#6858 = ORIENTED_EDGE ( 'NONE', *, *, #12693, .F. ) ;
#6860 = CARTESIAN_POINT ( 'NONE',  ( 61.25000000000003553, -1.039502773796944890, 1.800471618824829756 ) ) ;
#6859 = CARTESIAN_POINT ( 'NONE',  ( 53.96142581635486124, 5.170113101904351360, 2.049999999999811529 ) ) ;
#6861 = CARTESIAN_POINT ( 'NONE',  ( -58.93749999999997158, 3.238593381231834378, 2.874284765127034014 ) ) ;
#6862 = FACE_OUTER_BOUND ( 'NONE', #30137, .T. ) ;
#6863 = ADVANCED_FACE ( 'NONE', ( #110 ), #5889, .T. ) ;
#6864 = ORIENTED_EDGE ( 'NONE', *, *, #7588, .T. ) ;
#6865 = CARTESIAN_POINT ( 'NONE',  ( 22.58314801556729634, 7.622751244490449274, 1.424999999999920997 ) ) ;
#6866 = DIRECTION ( 'NONE',  ( 1.000000000000000000, -0.000000000000000000, -1.047444401652940007E-14 ) ) ;
#6867 = CARTESIAN_POINT ( 'NONE',  ( -58.93749999999995737, 1.962990915244749557, -3.400000000000200640 ) ) ;
#6868 = ORIENTED_EDGE ( 'NONE', *, *, #4153, .T. ) ;
#6869 = ORIENTED_EDGE ( 'NONE', *, *, #26722, .T. ) ;
#6870 = AXIS2_PLACEMENT_3D ( 'NONE', #20880, #21366, #30993 ) ;
#6871 = DIRECTION ( 'NONE',  ( 0.000000000000000000, 1.000000000000000000, 3.491481338843132961E-15 ) ) ;
#6872 = ORIENTED_EDGE ( 'NONE', *, *, #18887, .T. ) ;
#6873 = AXIS2_PLACEMENT_3D ( 'NONE', #21591, #9560, #14430 ) ;
#6874 = CARTESIAN_POINT ( 'NONE',  ( 50.95599726996783829, 0.9532299437236954054, -1.316046228059489120 ) ) ;
#6875 = CARTESIAN_POINT ( 'NONE',  ( -57.63452994616205416, -3.117691453623976816, 1.799999999999783329 ) ) ;
#6876 = EDGE_LOOP ( 'NONE', ( #5474, #6254, #25928, #30692, #19504 ) ) ;
#6877 = DIRECTION ( 'NONE',  ( -0.000000000000000000, -0.000000000000000000, -1.000000000000000000 ) ) ;
#6878 = LINE ( 'NONE', #11786, #24290 ) ;
#6879 = CARTESIAN_POINT ( 'NONE',  ( 31.86617018594176898, 7.736336509539437856, 2.049999999999888800 ) ) ;
#6880 = ORIENTED_EDGE ( 'NONE', *, *, #7097, .F. ) ;
#6881 = ORIENTED_EDGE ( 'NONE', *, *, #24152, .F. ) ;
#6882 = CIRCLE ( 'NONE', #20546, 0.1500000000000001887 ) ;
#6883 = ADVANCED_FACE ( 'NONE', ( #31137 ), #9096, .F. ) ;
#6884 = DIRECTION ( 'NONE',  ( 1.000000000000000000, 0.000000000000000000, 0.000000000000000000 ) ) ;
#6885 = VECTOR ( 'NONE', #19636, 1000.000000000000114 ) ;
#6886 = CARTESIAN_POINT ( 'NONE',  ( -62.09999999999997300, -2.736522795516423301, 0.2343065891546179669 ) ) ;
#6887 = CARTESIAN_POINT ( 'NONE',  ( 56.96003682719288008, -0.7597908294545935304, -2.486534234876009553 ) ) ;
#6888 = ORIENTED_EDGE ( 'NONE', *, *, #22226, .T. ) ;
#6889 = CARTESIAN_POINT ( 'NONE',  ( 50.50000000000002132, 5.291762632692320630E-13, -1.996089927833914146 ) ) ;
#6890 = B_SPLINE_CURVE_WITH_KNOTS ( 'NONE', 3,
 ( #6725, #23839, #6418, #11015, #20693, #16081, #30318, #8626, #27942, #6258 ),
 .UNSPECIFIED., .F., .F.,
 ( 4, 2, 2, 2, 4 ),
 ( 0.000000000000000000, 9.706686070839353657E-05, 0.0001941337214167870731, 0.0002912005821251806097, 0.0003882674428335743089 ),
 .UNSPECIFIED. ) ;
#6891 = FACE_OUTER_BOUND ( 'NONE', #5653, .T. ) ;
#6892 = DIRECTION ( 'NONE',  ( 0.000000000000000000, 0.000000000000000000, -1.000000000000000000 ) ) ;
#6893 = CIRCLE ( 'NONE', #14481, 3.399999999999999911 ) ;
#6894 = CARTESIAN_POINT ( 'NONE',  ( 58.65000000000004121, -1.793224408421451477, 0.5487562170608006884 ) ) ;
#6896 = PLANE ( 'NONE',  #10856 ) ;
#6895 = CARTESIAN_POINT ( 'NONE',  ( 58.65000000000001990, -0.5811678240976237975, -1.782657835994593487 ) ) ;
#6897 = EDGE_CURVE ( 'NONE', #25072, #6720, #26538, .T. ) ;
#6898 = AXIS2_PLACEMENT_3D ( 'NONE', #26729, #9482, #14206 ) ;
#6899 = CARTESIAN_POINT ( 'NONE',  ( 51.31943556899493331, 1.088761256244167086, 1.206353010735628395 ) ) ;
#6900 = CARTESIAN_POINT ( 'NONE',  ( -57.65835481156722864, -0.7533615035078039535, 3.673546848079178861 ) ) ;
#6902 = CARTESIAN_POINT ( 'NONE',  ( 58.50000000000001421, -0.8156862745098042433, -2.468735688885369317 ) ) ;
#6901 = AXIS2_PLACEMENT_3D ( 'NONE', #26975, #7670, #2760 ) ;
#6903 = EDGE_LOOP ( 'NONE', ( #18949, #6072, #12690 ) ) ;
#6904 = AXIS2_PLACEMENT_3D ( 'NONE', #29826, #17810, #1159 ) ;
#6905 = AXIS2_PLACEMENT_3D ( 'NONE', #31304, #4554, #21972 ) ;
#6906 = ORIENTED_EDGE ( 'NONE', *, *, #24354, .F. ) ;
#6907 = AXIS2_PLACEMENT_3D ( 'NONE', #6047, #20622, #6338 ) ;
#6908 = EDGE_CURVE ( 'NONE', #6782, #8527, #5539, .T. ) ;
#6909 = DIRECTION ( 'NONE',  ( -1.000000000000000000, -0.000000000000000000, -0.000000000000000000 ) ) ;
#6910 = ORIENTED_EDGE ( 'NONE', *, *, #23146, .F. ) ;
#6911 = ADVANCED_FACE ( 'NONE', ( #26072 ), #4381, .F. ) ;
#6912 =( BOUNDED_CURVE ( )  B_SPLINE_CURVE ( 2, ( #11866, #16642, #4727, #21394, #23436, #9342, #21547, #26281, #1573 ),
 .UNSPECIFIED., .F., .T. ) 
 B_SPLINE_CURVE_WITH_KNOTS ( ( 3, 2, 2, 2, 3 ),
 ( 0.3611111111111111605, 0.3703703703703703498, 0.3888888888888888951, 0.4074074074074073848, 0.4166666666666666852 ),
 .UNSPECIFIED. ) 
 CURVE ( )  GEOMETRIC_REPRESENTATION_ITEM ( )  RATIONAL_B_SPLINE_CURVE ( ( 0.9330127018922194093, 0.9330127018922197424, 1.000000000000000000, 0.8660254037844387076, 1.000000000000000000, 0.8660254037844387076, 1.000000000000000000, 0.9330127018922191873, 0.9330127018922194093 ) ) 
 REPRESENTATION_ITEM ( '' )  );
#6913 = DIRECTION ( 'NONE',  ( -1.000000000000000000, 1.219044193948983948E-29, -3.491481338843133355E-15 ) ) ;
#6914 = CARTESIAN_POINT ( 'NONE',  ( -60.40835481156722153, -3.238593381231841928, -2.874284765127021579 ) ) ;
#6916 = CARTESIAN_POINT ( 'NONE',  ( -35.85663232820581925, 3.779372838781723587, 3.883777296072584484 ) ) ;
#6915 = CARTESIAN_POINT ( 'NONE',  ( 51.70000000000002416, 2.428612866367529932E-14, -1.805095852181900386E-13 ) ) ;
#6917 = ADVANCED_FACE ( 'NONE', ( #19133 ), #5567, .T. ) ;
#6918 = ORIENTED_EDGE ( 'NONE', *, *, #5083, .F. ) ;
#6919 = CARTESIAN_POINT ( 'NONE',  ( 22.20365324802978435, 7.487628413149166384, -2.050000000000077538 ) ) ;
#6920 = VERTEX_POINT ( 'NONE', #29520 ) ;
#6921 = CARTESIAN_POINT ( 'NONE',  ( -59.69999999999998153, -3.161828374300064581, 1.538811659727342462 ) ) ;
#6922 = ORIENTED_EDGE ( 'NONE', *, *, #21431, .F. ) ;
#6924 = LINE ( 'NONE', #23393, #28711 ) ;
#6923 = CARTESIAN_POINT ( 'NONE',  ( 50.42159256128543632, 1.310166284604407760, 3.885185101012171849 ) ) ;
#6925 = CIRCLE ( 'NONE', #24602, 0.1000000000000001027 ) ;
#6926 = ORIENTED_EDGE ( 'NONE', *, *, #1170, .T. ) ;
#6927 = CIRCLE ( 'NONE', #20581, 2.764644660940665855 ) ;
#6928 = CARTESIAN_POINT ( 'NONE',  ( 58.75000000000000000, 1.782657835995382190, -0.5811678240976815291 ) ) ;
#6929 = B_SPLINE_CURVE_WITH_KNOTS ( 'NONE', 3,
 ( #22371, #10034, #2593, #7500 ),
 .UNSPECIFIED., .F., .F.,
 ( 4, 4 ),
 ( 6.653267247438212099E-05, 0.0002183616642542154668 ),
 .UNSPECIFIED. ) ;
#6930 = CARTESIAN_POINT ( 'NONE',  ( -59.40875807382336404, 3.366278345796976268, 1.250136525132555798 ) ) ;
#6931 = AXIS2_PLACEMENT_3D ( 'NONE', #25492, #27555, #20459 ) ;
#6932 = CARTESIAN_POINT ( 'NONE',  ( 57.05000000000001137, 0.7500000000000001110, -1.778341924377885963 ) ) ;
#6933 = CARTESIAN_POINT ( 'NONE',  ( -58.07202994616203995, 2.078460969082674747, -3.600000000000197709 ) ) ;
#6934 = CIRCLE ( 'NONE', #15005, 0.09999999999999986677 ) ;
#6935 = CARTESIAN_POINT ( 'NONE',  ( 68.00000000000001421, 1.401298464324817071E-42, -7.122621931239992550E-13 ) ) ;
#6936 = AXIS2_PLACEMENT_3D ( 'NONE', #25566, #16085, #23369 ) ;
#6937 = AXIS2_PLACEMENT_3D ( 'NONE', #20346, #1612, #6846 ) ;
#6939 = AXIS2_PLACEMENT_3D ( 'NONE', #4347, #14480, #7356 ) ;
#6938 = CARTESIAN_POINT ( 'NONE',  ( -58.47099364905386665, -3.399999999999994138, 0.9110272542655848405 ) ) ;
#6940 = CARTESIAN_POINT ( 'NONE',  ( -60.59999999999997300, -2.426837276046140079, -1.064406330116907329 ) ) ;
#6941 = EDGE_CURVE ( 'NONE', #19844, #17127, #15403, .T. ) ;
#6942 = CARTESIAN_POINT ( 'NONE',  ( -55.86042740578360366, 3.725040285533371520, -1.239922660687672540 ) ) ;
#6943 = EDGE_CURVE ( 'NONE', #26007, #10689, #27163, .T. ) ;
#6944 = ORIENTED_EDGE ( 'NONE', *, *, #15111, .F. ) ;
#6945 = CIRCLE ( 'NONE', #30187, 3.200000000000000178 ) ;
#6946 = CARTESIAN_POINT ( 'NONE',  ( -35.85663232820584057, 1.123735532908267665, -5.289358697221546279 ) ) ;
#6947 = AXIS2_PLACEMENT_3D ( 'NONE', #12616, #5184, #27021 ) ;
#6948 = CARTESIAN_POINT ( 'NONE',  ( 52.04553598140720538, 4.350000000000022737, 1.551140582956726632 ) ) ;
#6949 = CARTESIAN_POINT ( 'NONE',  ( 48.38568300895507690, 1.130504494894958745, -3.941663789486467895 ) ) ;
#6950 = VERTEX_POINT ( 'NONE', #5633 ) ;
#6951 = CARTESIAN_POINT ( 'NONE',  ( -35.85663232820583346, -4.683225679163361299, 2.703237727951226077 ) ) ;
#6952 = AXIS2_PLACEMENT_3D ( 'NONE', #989, #18249, #25668 ) ;
#6953 = ORIENTED_EDGE ( 'NONE', *, *, #4164, .F. ) ;
#6955 = DIRECTION ( 'NONE',  ( 1.000000000000000000, 0.000000000000000000, 0.000000000000000000 ) ) ;
#6954 = CARTESIAN_POINT ( 'NONE',  ( -57.34599364905385954, 3.400000000000012346, -0.9110272542660015072 ) ) ;
#6956 = EDGE_CURVE ( 'NONE', #24434, #23157, #23796, .T. ) ;
#6957 = ORIENTED_EDGE ( 'NONE', *, *, #7264, .F. ) ;
#6958 = ORIENTED_EDGE ( 'NONE', *, *, #6324, .F. ) ;
#6959 = FACE_OUTER_BOUND ( 'NONE', #2357, .T. ) ;
#6960 = VECTOR ( 'NONE', #3285, 1000.000000000000000 ) ;
#6961 = LINE ( 'NONE', #18840, #30824 ) ;
#6962 = AXIS2_PLACEMENT_3D ( 'NONE', #903, #26440, #2381 ) ;
#6964 = CARTESIAN_POINT ( 'NONE',  ( -64.31974649313019654, 4.901397072418226544E-16, 2.651112292416007398E-15 ) ) ;
#6963 = DIRECTION ( 'NONE',  ( -1.000000000000000000, -3.053848253006669023E-16, 2.042510438544995415E-16 ) ) ;
#6965 = AXIS2_PLACEMENT_3D ( 'NONE', #5566, #12222, #189 ) ;
#6966 = ORIENTED_EDGE ( 'NONE', *, *, #31098, .F. ) ;
#6967 = CARTESIAN_POINT ( 'NONE',  ( -60.92292740578359656, 1.073804522883521351, 3.225979517392337570 ) ) ;
#6968 = CARTESIAN_POINT ( 'NONE',  ( 15.03925126672132961, 4.018128179617565188, -3.618665901676623164 ) ) ;
#6969 = CARTESIAN_POINT ( 'NONE',  ( -54.65835481156722864, -0.7533615035078032873, 3.673546848079177973 ) ) ;
#6970 = DIRECTION ( 'NONE',  ( 1.037591611799212092E-14, 0.000000000000000000, 1.000000000000000000 ) ) ;
#6971 = CARTESIAN_POINT ( 'NONE',  ( -59.69999999999997442, 8.366749974758454467E-15, -2.120534355533670266E-13 ) ) ;
#6972 = PLANE ( 'NONE',  #16215 ) ;
#6973 = CARTESIAN_POINT ( 'NONE',  ( 51.80000000000002558, 6.475000000000062705, 2.049999999999819522 ) ) ;
#6974 = AXIS2_PLACEMENT_3D ( 'NONE', #27831, #6140, #5994 ) ;
#6975 = ORIENTED_EDGE ( 'NONE', *, *, #3807, .T. ) ;
#6976 = CIRCLE ( 'NONE', #30235, 1.875000000000001776 ) ;
#6977 = FACE_OUTER_BOUND ( 'NONE', #13420, .T. ) ;
#6978 = AXIS2_PLACEMENT_3D ( 'NONE', #11281, #8908, #18905 ) ;
#6979 = CARTESIAN_POINT ( 'NONE',  ( -36.48174642953001978, 2.847679722116494005, -4.601476325142689561 ) ) ;
#6980 = CARTESIAN_POINT ( 'NONE',  ( 48.40000000000001279, 0.7619326981554777056, 3.939508824314740032 ) ) ;
#6981 = CARTESIAN_POINT ( 'NONE',  ( -59.43788607448336592, 2.385332005665378841, -1.158943404468661731 ) ) ;
#6982 = EDGE_CURVE ( 'NONE', #16343, #29981, #25297, .T. ) ;
#6983 = EDGE_CURVE ( 'NONE', #11953, #13554, #20219, .T. ) ;
#6984 = CARTESIAN_POINT ( 'NONE',  ( -59.19999999999997442, 4.156921938165309527, 1.250136525132554910 ) ) ;
#6985 = AXIS2_PLACEMENT_3D ( 'NONE', #5476, #13206, #13058 ) ;
#6988 = EDGE_CURVE ( 'NONE', #9283, #30937, #5010, .T. ) ;
#6987 = DIRECTION ( 'NONE',  ( 0.000000000000000000, 0.2008964009354147762, -0.9796124928211139560 ) ) ;
#6986 = CARTESIAN_POINT ( 'NONE',  ( 54.31409749668478071, 6.709390224138188863, -2.050000000000189004 ) ) ;
#6989 = CARTESIAN_POINT ( 'NONE',  ( 48.00000000000001421, -4.417905791132255899, -1.285520503972909623 ) ) ;
#6991 = CARTESIAN_POINT ( 'NONE',  ( -59.62365256889266618, 2.027865038274679232, 1.710353782976151482 ) ) ;
#6990 = CARTESIAN_POINT ( 'NONE',  ( -59.40743313238012036, 2.395752775956333291, 1.250136525132548027 ) ) ;
#6992 = VERTEX_POINT ( 'NONE', #22278 ) ;
#6993 = CARTESIAN_POINT ( 'NONE',  ( 58.74154451056429593, -1.832994048937183429, 0.3947215634758409197 ) ) ;
#6994 = UNCERTAINTY_MEASURE_WITH_UNIT (LENGTH_MEASURE( 1.000000000000000082E-05 ), #26465, 'distance_accuracy_value', 'NONE');
#6995 = DIRECTION ( 'NONE',  ( 0.000000000000000000, 0.2008964009354147484, -0.9796124928211139560 ) ) ;
#6997 = CARTESIAN_POINT ( 'NONE',  ( -36.56242893520595061, 5.206628483174555733, 1.466363261642575466 ) ) ;
#6996 = CARTESIAN_POINT ( 'NONE',  ( -44.59999999999996589, 1.400000000000023670, -3.959797974644836405 ) ) ;
#6998 = CARTESIAN_POINT ( 'NONE',  ( 15.68751737981894578, -5.244794032782597704, 1.329291831544269664 ) ) ;
#6999 = ORIENTED_EDGE ( 'NONE', *, *, #28902, .T. ) ;
#7000 = ORIENTED_EDGE ( 'NONE', *, *, #11316, .T. ) ;
#7001 = DIRECTION ( 'NONE',  ( 1.000000000000000000, 0.000000000000000000, 0.000000000000000000 ) ) ;
#7002 = AXIS2_PLACEMENT_3D ( 'NONE', #5190, #27027, #2981 ) ;
#7003 = EDGE_CURVE ( 'NONE', #11632, #21265, #6716, .T. ) ;
#7004 = ORIENTED_EDGE ( 'NONE', *, *, #15291, .F. ) ;
#7005 = CARTESIAN_POINT ( 'NONE',  ( 56.99229849798533820, -0.7794861535680733811, -1.732743875013533108 ) ) ;
#7006 = DIRECTION ( 'NONE',  ( 0.000000000000000000, 0.000000000000000000, 1.000000000000000000 ) ) ;
#7007 = ORIENTED_EDGE ( 'NONE', *, *, #4821, .F. ) ;
#7008 = FACE_OUTER_BOUND ( 'NONE', #21008, .T. ) ;
#7009 = ORIENTED_EDGE ( 'NONE', *, *, #19784, .T. ) ;
#7010 = CARTESIAN_POINT ( 'NONE',  ( 69.00000000000001421, 4.557543281186736018E-17, -7.227366371405287181E-13 ) ) ;
#7011 = ORIENTED_EDGE ( 'NONE', *, *, #3740, .F. ) ;
#7012 = ORIENTED_EDGE ( 'NONE', *, *, #677, .T. ) ;
#7013 = ORIENTED_EDGE ( 'NONE', *, *, #8735, .T. ) ;
#7014 = CARTESIAN_POINT ( 'NONE',  ( -54.75952994616206837, -4.643455692769931152E-15, 3.599999999999804245 ) ) ;
#7015 = DIRECTION ( 'NONE',  ( 1.000000000000000000, 0.000000000000000000, -1.047444401652940007E-14 ) ) ;
#7016 = FACE_OUTER_BOUND ( 'NONE', #29348, .T. ) ;
#7017 = DIRECTION ( 'NONE',  ( 0.000000000000000000, 0.000000000000000000, 1.000000000000000000 ) ) ;
#7018 = AXIS2_PLACEMENT_3D ( 'NONE', #16441, #18987, #21375 ) ;
#7019 = CARTESIAN_POINT ( 'NONE',  ( -60.87073935753598164, -2.495861326358214782, -1.035156648315508354 ) ) ;
#7020 = AXIS2_PLACEMENT_3D ( 'NONE', #13815, #17175, #29481 ) ;
#7021 = EDGE_CURVE ( 'NONE', #4586, #16552, #2910, .T. ) ;
#7023 = CARTESIAN_POINT ( 'NONE',  ( 61.25000000000002132, 6.415596960124259844E-13, 3.111507638930570854E-58 ) ) ;
#7022 = DIRECTION ( 'NONE',  ( -2.614375865348240525E-16, 0.2008964009354147762, -0.9796124928211140670 ) ) ;
#7024 = DIRECTION ( 'NONE',  ( 0.000000000000000000, -0.3333333333333469706, -0.9428090415820586934 ) ) ;
#7025 = CARTESIAN_POINT ( 'NONE',  ( 52.20711756518984004, -0.4999999999994533817, 1.718465885608440491 ) ) ;
#7026 = DIRECTION ( 'NONE',  ( -1.000000000000000000, 0.000000000000000000, 0.000000000000000000 ) ) ;
#7027 = ORIENTED_EDGE ( 'NONE', *, *, #14666, .T. ) ;
#7028 = B_SPLINE_CURVE_WITH_KNOTS ( 'NONE', 3,
 ( #18493, #28136, #1681, #11342 ),
 .UNSPECIFIED., .F., .F.,
 ( 4, 4 ),
 ( 5.935267624065488723E-05, 0.0002061672048306624071 ),
 .UNSPECIFIED. ) ;
#7029 = CARTESIAN_POINT ( 'NONE',  ( -57.22499999999997300, 2.964020293532818446E-15, 1.549317489258312010E-18 ) ) ;
#7030 = DIRECTION ( 'NONE',  ( -1.000000000000000000, -0.000000000000000000, 3.491481338843133355E-15 ) ) ;
#7031 = VERTEX_POINT ( 'NONE', #26853 ) ;
#7033 = CARTESIAN_POINT ( 'NONE',  ( 50.33290990662630549, -1.365599538210731767, 3.854893000251053081 ) ) ;
#7032 = CARTESIAN_POINT ( 'NONE',  ( 58.65000000000002700, -0.8948927608030060599, -1.760622601996600922 ) ) ;
#7034 = CARTESIAN_POINT ( 'NONE',  ( 54.44213315155518274, 6.358439074249562672, -1.988253509196054036 ) ) ;
#7035 = DIRECTION ( 'NONE',  ( -1.000000000000000000, 0.000000000000000000, 1.047444401652940007E-14 ) ) ;
#7036 = EDGE_CURVE ( 'NONE', #14986, #1995, #29341, .T. ) ;
#7037 = EDGE_LOOP ( 'NONE', ( #21995, #18003, #29146, #13715 ) ) ;
#7038 = CARTESIAN_POINT ( 'NONE',  ( 34.56702326949726256, 8.213851659285209550, 1.949999999999879385 ) ) ;
#7039 = CARTESIAN_POINT ( 'NONE',  ( -71.49999999999998579, -1.395601618875910821E-15, 2.917180974979867506E-15 ) ) ;
#7040 = CARTESIAN_POINT ( 'NONE',  ( -55.32202994616205416, -4.156921938165296204, -2.115361882398036228E-13 ) ) ;
#7041 = VERTEX_POINT ( 'NONE', #24788 ) ;
#7042 = ORIENTED_EDGE ( 'NONE', *, *, #15952, .F. ) ;
#7043 = FACE_OUTER_BOUND ( 'NONE', #27892, .T. ) ;
#7044 = VERTEX_POINT ( 'NONE', #17674 ) ;
#7045 = CARTESIAN_POINT ( 'NONE',  ( 48.43966969621122587, -1.282137971188096914, 3.869545987293864453 ) ) ;
#7046 = CIRCLE ( 'NONE', #2472, 0.1000000000000000472 ) ;
#7047 = SHAPE_REPRESENTATION ( 'MAS-683', ( #18680, #8552, #14121, #19705, #999, #26266, #30804, #27773, #16675, #30297, #20727, #18702 ), #24258 ) ;
#7048 = CARTESIAN_POINT ( 'NONE',  ( -55.50952994616206126, -4.643455692769921685E-15, 3.599999999999801581 ) ) ;
#7049 = ORIENTED_EDGE ( 'NONE', *, *, #18215, .F. ) ;
#7050 = LINE ( 'NONE', #24140, #14561 ) ;
#7051 = CARTESIAN_POINT ( 'NONE',  ( 58.65000000000001990, 6.143261415694495821E-13, 3.111507638930570854E-58 ) ) ;
#7052 = DIRECTION ( 'NONE',  ( 0.000000000000000000, 0.000000000000000000, -1.000000000000000000 ) ) ;
#7053 = ORIENTED_EDGE ( 'NONE', *, *, #10648, .F. ) ;
#7054 = CARTESIAN_POINT ( 'NONE',  ( -59.29999999999997584, 2.330309927981285032E-15, 4.253626757584724400E-16 ) ) ;
#7055 = CARTESIAN_POINT ( 'NONE',  ( -62.09999999999997300, -2.712337243103304374, 0.1831892273270349092 ) ) ;
#7056 = CARTESIAN_POINT ( 'NONE',  ( 58.75000000694009117, -0.9428687169905247689, -1.682988785000552934 ) ) ;
#7057 = ORIENTED_EDGE ( 'NONE', *, *, #29281, .T. ) ;
#7058 = AXIS2_PLACEMENT_3D ( 'NONE', #28664, #7133, #572 ) ;
#7059 = CARTESIAN_POINT ( 'NONE',  ( -59.69999999999997442, -2.455304892039217091, -1.238538609462283446 ) ) ;
#7060 = DIRECTION ( 'NONE',  ( -1.000000000000000000, -0.000000000000000000, -0.000000000000000000 ) ) ;
#7061 = EDGE_CURVE ( 'NONE', #13972, #21159, #14383, .T. ) ;
#7062 = CYLINDRICAL_SURFACE ( 'NONE', #17557, 4.000000000000000000 ) ;
#7064 = DIRECTION ( 'NONE',  ( 1.000000000000000000, 0.000000000000000000, -0.000000000000000000 ) ) ;
#7063 = CARTESIAN_POINT ( 'NONE',  ( 58.75000000000002132, -0.4991218602006210481, -1.863314270025920649 ) ) ;
#7065 = CARTESIAN_POINT ( 'NONE',  ( 58.72153194576689117, -0.4999999999993851585, 1.827449685319723738 ) ) ;
#7066 = CARTESIAN_POINT ( 'NONE',  ( 50.25000000000000000, 1.996089927834441502, -0.1249999999989956784 ) ) ;
#7067 = AXIS2_PLACEMENT_3D ( 'NONE', #12800, #16959, #14577 ) ;
#7068 = DIRECTION ( 'NONE',  ( 0.000000000000000000, 0.000000000000000000, 1.000000000000000000 ) ) ;
#7069 = ORIENTED_EDGE ( 'NONE', *, *, #10658, .T. ) ;
#7070 = CARTESIAN_POINT ( 'NONE',  ( -59.14778739134288799, -2.353873335156955182, 1.243527661805360340 ) ) ;
#7071 = ORIENTED_EDGE ( 'NONE', *, *, #23641, .T. ) ;
#7072 = CARTESIAN_POINT ( 'NONE',  ( -60.49999999999995737, -0.8596938233273121455, 4.192045280110958672 ) ) ;
#7073 = CARTESIAN_POINT ( 'NONE',  ( -59.59585481156723574, -1.184343223768586695, -3.558065644182724974 ) ) ;
#7075 = CARTESIAN_POINT ( 'NONE',  ( -36.11122220296839203, 3.378548217643384977, 3.972894518062678237 ) ) ;
#7074 = CARTESIAN_POINT ( 'NONE',  ( 22.07280086217093640, 8.086143481909152442, -1.950000000000076339 ) ) ;
#7076 = ORIENTED_EDGE ( 'NONE', *, *, #3807, .F. ) ;
#7077 = EDGE_LOOP ( 'NONE', ( #26156, #6349, #312, #948, #13259 ) ) ;
#7078 = CARTESIAN_POINT ( 'NONE',  ( 60.87997700083086272, 0.6727827007665463377, -1.479885446458162113 ) ) ;
#7079 = VERTEX_POINT ( 'NONE', #418 ) ;
#7080 = CARTESIAN_POINT ( 'NONE',  ( 47.00000000000002842, -4.137422847598536180, 2.245380186108497433 ) ) ;
#7081 = VERTEX_POINT ( 'NONE', #15283 ) ;
#7082 = CARTESIAN_POINT ( 'NONE',  ( -36.52757395963740095, 5.349060760730894870, 0.7993770229879135769 ) ) ;
#7083 = ORIENTED_EDGE ( 'NONE', *, *, #14371, .T. ) ;
#7084 = LINE ( 'NONE', #2161, #24266 ) ;
#7085 = EDGE_CURVE ( 'NONE', #24984, #4847, #5596, .T. ) ;
#7086 = DIRECTION ( 'NONE',  ( -1.000000000000000000, -3.054025858079668409E-16, 2.042474015755241579E-16 ) ) ;
#7087 = VECTOR ( 'NONE', #29550, 1000.000000000000000 ) ;
#7088 = DIRECTION ( 'NONE',  ( 1.000000000000000000, 1.047444401652940007E-14, -0.000000000000000000 ) ) ;
#7089 = CIRCLE ( 'NONE', #14648, 0.1000000000000028644 ) ;
#7090 = DIRECTION ( 'NONE',  ( 0.000000000000000000, 1.000000000000000000, 3.491481338843132961E-15 ) ) ;
#7091 = CARTESIAN_POINT ( 'NONE',  ( -60.69702994616205416, -2.078460969082657872, 3.599999999999776712 ) ) ;
#7092 = DIRECTION ( 'NONE',  ( -1.000000000000000000, 0.000000000000000000, 1.047444401652940007E-14 ) ) ;
#7093 = AXIS2_PLACEMENT_3D ( 'NONE', #10837, #27464, #707 ) ;
#7094 = EDGE_CURVE ( 'NONE', #23157, #11667, #23274, .T. ) ;
#7095 = CARTESIAN_POINT ( 'NONE',  ( 17.21035195517769267, -24.59258869922087243, -3.011723503324820852E-15 ) ) ;
#7096 = FACE_OUTER_BOUND ( 'NONE', #1243, .T. ) ;
#7097 = EDGE_CURVE ( 'NONE', #26416, #10954, #13178, .T. ) ;
#7098 = SURFACE_STYLE_USAGE ( .BOTH. , #9931 ) ;
#7099 = AXIS2_PLACEMENT_3D ( 'NONE', #11157, #27792, #25556 ) ;
#7100 = CARTESIAN_POINT ( 'NONE',  ( -36.52679053911622020, -0.8934212604923426060, 5.334164326942878454 ) ) ;
#7101 = ORIENTED_EDGE ( 'NONE', *, *, #3891, .T. ) ;
#7102 = CARTESIAN_POINT ( 'NONE',  ( 57.03821272586434787, -0.7500000328843418052, -2.490438846756156899 ) ) ;
#7103 = CARTESIAN_POINT ( 'NONE',  ( -54.45495050826418293, 1.499999999999999112, 3.300094695611021756 ) ) ;
#7104 = CARTESIAN_POINT ( 'NONE',  ( 53.91582462592158720, 6.672259099522137582, -2.142504121165067499E-08 ) ) ;
#7105 = ORIENTED_EDGE ( 'NONE', *, *, #28039, .F. ) ;
#7106 = ADVANCED_FACE ( 'NONE', ( #1182 ), #3558, .F. ) ;
#7107 = CARTESIAN_POINT ( 'NONE',  ( -54.46895629856896903, 1.503487923075246480, 4.032311158269683560 ) ) ;
#7108 = ORIENTED_EDGE ( 'NONE', *, *, #29412, .T. ) ;
#7109 = CARTESIAN_POINT ( 'NONE',  ( 15.29954477411491354, 1.123735554575626461, -5.289358692618272073 ) ) ;
#7111 = FACE_OUTER_BOUND ( 'NONE', #10832, .T. ) ;
#7110 = CARTESIAN_POINT ( 'NONE',  ( 58.72419296898065255, 0.9760445624820607291, -1.601054456121077330 ) ) ;
#7112 = PRODUCT_DEFINITION_SHAPE ( 'NONE', 'NONE',  #15141 ) ;
#7113 = ORIENTED_EDGE ( 'NONE', *, *, #7190, .T. ) ;
#7114 = DIRECTION ( 'NONE',  ( -1.000000000000000000, 1.219044193948983948E-29, -3.491481338843133355E-15 ) ) ;
#7115 = TOROIDAL_SURFACE ( 'NONE', #12150, 4.199999999999993072, 0.1000000000000000056 ) ;
#7116 = DIRECTION ( 'NONE',  ( 0.000000000000000000, 0.000000000000000000, -1.000000000000000000 ) ) ;
#7118 = CARTESIAN_POINT ( 'NONE',  ( -62.09999999999997300, 1.168016602258162478E-15, 2.197726754101795588E-15 ) ) ;
#7117 = CARTESIAN_POINT ( 'NONE',  ( 52.20711756518982583, 0.7500000000005468959, -1.718465885608440269 ) ) ;
#7119 = ORIENTED_EDGE ( 'NONE', *, *, #12535, .F. ) ;
#7120 = CARTESIAN_POINT ( 'NONE',  ( -60.29792740578359656, 3.330682475591789427, 0.6830477631804114935 ) ) ;
#7121 = DIRECTION ( 'NONE',  ( 1.000000000000000000, -0.000000000000000000, -0.000000000000000000 ) ) ;
#7122 = CARTESIAN_POINT ( 'NONE',  ( 46.90000000000001990, -4.241638912518125082, -1.073342218585543684 ) ) ;
#7123 = EDGE_CURVE ( 'NONE', #12424, #1382, #28853, .T. ) ;
#7124 = FACE_OUTER_BOUND ( 'NONE', #7188, .T. ) ;
#7125 = DIRECTION ( 'NONE',  ( 0.000000000000000000, 0.8381322357044638238, 0.5454670984331106975 ) ) ;
#7126 = DIRECTION ( 'NONE',  ( -3.491481338843133355E-15, 0.000000000000000000, -1.000000000000000000 ) ) ;
#7127 = EDGE_CURVE ( 'NONE', #30388, #25072, #17218, .T. ) ;
#7128 = CARTESIAN_POINT ( 'NONE',  ( -54.49853245345825314, 1.536420219664552667, -4.055116445457033869 ) ) ;
#7129 = ORIENTED_EDGE ( 'NONE', *, *, #3888, .F. ) ;
#7130 = DIRECTION ( 'NONE',  ( 1.000000000000000000, -0.000000000000000000, -1.047444401652940007E-14 ) ) ;
#7131 = FACE_OUTER_BOUND ( 'NONE', #14913, .T. ) ;
#7132 = EDGE_CURVE ( 'NONE', #23389, #15285, #20829, .T. ) ;
#7133 = DIRECTION ( 'NONE',  ( -1.000000000000000000, 1.219044193948983948E-29, -3.491481338843133355E-15 ) ) ;
#7134 = CARTESIAN_POINT ( 'NONE',  ( -73.89999999999997726, -2.435524336289708093E-15, 4.607889071584891164E-15 ) ) ;
#7135 = ADVANCED_FACE ( 'NONE', ( #8475 ), #13210, .T. ) ;
#7136 = VECTOR ( 'NONE', #74, 1000.000000000000000 ) ;
#7137 = CARTESIAN_POINT ( 'NONE',  ( -62.06730027881287981, -2.642931028823815254, 0.1961448473822917093 ) ) ;
#7139 = DIRECTION ( 'NONE',  ( 3.491481338843133355E-15, 3.491481338843133355E-15, -1.000000000000000000 ) ) ;
#7138 = CARTESIAN_POINT ( 'NONE',  ( -44.59999999999995879, -1.399999999999978817, -4.029888335922158227 ) ) ;
#7140 = CARTESIAN_POINT ( 'NONE',  ( 47.37826908275614812, -4.356630359622855053, -1.481809601934080511 ) ) ;
#7142 = CARTESIAN_POINT ( 'NONE',  ( -59.59999999999998721, 2.022492213459062160, 1.712315755489264513 ) ) ;
#7141 = DIRECTION ( 'NONE',  ( 1.000000000000000000, -0.000000000000000000, -1.047444401652940007E-14 ) ) ;
#7143 = VERTEX_POINT ( 'NONE', #27467 ) ;
#7144 = CARTESIAN_POINT ( 'NONE',  ( 58.75000000000004263, -1.871971993774602661, 0.6020210199438860155 ) ) ;
#7145 = DIRECTION ( 'NONE',  ( -3.491481338843133355E-15, -3.491481338843133355E-15, 1.000000000000000000 ) ) ;
#7147 = CARTESIAN_POINT ( 'NONE',  ( -36.38139716712352367, 4.735424960531724459, 2.618558234549792196 ) ) ;
#7146 = CARTESIAN_POINT ( 'NONE',  ( -35.85663232820583346, -4.817150320980530864, 2.203324261490539282 ) ) ;
#7148 = CARTESIAN_POINT ( 'NONE',  ( 15.48609859788817822, -4.980680447166701441, 1.498595263773770281 ) ) ;
#7149 = ORIENTED_EDGE ( 'NONE', *, *, #29166, .F. ) ;
#7150 = VERTEX_POINT ( 'NONE', #27937 ) ;
#7151 = CIRCLE ( 'NONE', #11175, 0.2500000000000000000 ) ;
#7152 = DIRECTION ( 'NONE',  ( 0.000000000000000000, 0.6683962987614510132, -0.7438053426818022063 ) ) ;
#7153 = VERTEX_POINT ( 'NONE', #15757 ) ;
#7154 = CARTESIAN_POINT ( 'NONE',  ( 57.00791613703923844, 0.8068646677135199452, -2.471635681327667644 ) ) ;
#7155 = CARTESIAN_POINT ( 'NONE',  ( 51.80000000000002558, 3.954024819382278455, 2.040489646992247774 ) ) ;
#7156 = EDGE_LOOP ( 'NONE', ( #11793, #19924, #10896, #4507, #24627, #29866, #20367, #16383, #31311, #12556, #14506, #9907 ) ) ;
#7157 = ADVANCED_FACE ( 'NONE', ( #17978 ), #10692, .T. ) ;
#7158 = CARTESIAN_POINT ( 'NONE',  ( 58.65266784251152643, 1.873893454699072869, 0.06654060276385889705 ) ) ;
#7159 = ORIENTED_EDGE ( 'NONE', *, *, #19405, .T. ) ;
#7160 =( NAMED_UNIT ( * ) PLANE_ANGLE_UNIT ( ) SI_UNIT ( $, .RADIAN. ) );
#7161 = EDGE_CURVE ( 'NONE', #5085, #16145, #6091, .T. ) ;
#7162 = CARTESIAN_POINT ( 'NONE',  ( -60.08155989232412253, 3.925981830489463142, -1.989569613369437003E-13 ) ) ;
#7163 = ORIENTED_EDGE ( 'NONE', *, *, #19184, .T. ) ;
#7164 = SURFACE_STYLE_FILL_AREA ( #6834 ) ;
#7165 = EDGE_CURVE ( 'NONE', #6950, #6393, #6106, .T. ) ;
#7166 = ORIENTED_EDGE ( 'NONE', *, *, #6391, .F. ) ;
#7167 = ORIENTED_EDGE ( 'NONE', *, *, #10819, .F. ) ;
#7168 = CARTESIAN_POINT ( 'NONE',  ( -54.88452994616206126, 3.117691453623979481, 1.799999999999816858 ) ) ;
#7169 = CARTESIAN_POINT ( 'NONE',  ( 54.16322038507460235, 5.604326647956827223, -2.050000000000188116 ) ) ;
#7170 = DIRECTION ( 'NONE',  ( 0.000000000000000000, 0.000000000000000000, -1.000000000000000000 ) ) ;
#7171 = DIRECTION ( 'NONE',  ( 0.000000000000000000, -1.000000000000000000, -4.336808689942015369E-15 ) ) ;
#7172 = DIRECTION ( 'NONE',  ( 0.000000000000000000, 0.000000000000000000, 1.000000000000000000 ) ) ;
#7173 = VECTOR ( 'NONE', #113, 1000.000000000000000 ) ;
#7175 = CARTESIAN_POINT ( 'NONE',  ( 51.80000003860129709, 4.055787512326642918, -2.007379997706556285 ) ) ;
#7174 = LINE ( 'NONE', #46, #7434 ) ;
#7176 = CARTESIAN_POINT ( 'NONE',  ( 47.04702152735704601, -4.174452932061539556, 1.011256013762273698 ) ) ;
#7177 = CARTESIAN_POINT ( 'NONE',  ( 57.00000000000001421, 0.000000000000000000, 0.000000000000000000 ) ) ;
#7179 = CARTESIAN_POINT ( 'NONE',  ( -67.99999999999997158, -3.266925685480240183E-16, 2.202315069465531314E-15 ) ) ;
#7178 = DIRECTION ( 'NONE',  ( 0.000000000000000000, 0.000000000000000000, -1.000000000000000000 ) ) ;
#7180 = ORIENTED_EDGE ( 'NONE', *, *, #15305, .F. ) ;
#7181 = DIRECTION ( 'NONE',  ( 0.000000000000000000, 0.000000000000000000, -1.000000000000000000 ) ) ;
#7182 = CARTESIAN_POINT ( 'NONE',  ( 50.32622512580982033, 1.373801017329653762, -3.853344662332955473 ) ) ;
#7183 = DIRECTION ( 'NONE',  ( 1.000000000000000000, -0.000000000000000000, -0.000000000000000000 ) ) ;
#7184 = CARTESIAN_POINT ( 'NONE',  ( 54.24492254264022506, 6.702941018009704877, -2.050000000000186340 ) ) ;
#7185 = VERTEX_POINT ( 'NONE', #18450 ) ;
#7186 = CARTESIAN_POINT ( 'NONE',  ( 51.80000000000002558, 6.475000000000062705, 1.949999999999818767 ) ) ;
#7187 = CARTESIAN_POINT ( 'NONE',  ( -54.38452994616203995, 2.093608279459366986E-14, -3.600000000000193268 ) ) ;
#7188 = EDGE_LOOP ( 'NONE', ( #12875, #7583, #4218, #14700 ) ) ;
#7189 = VERTEX_POINT ( 'NONE', #11297 ) ;
#7190 = EDGE_CURVE ( 'NONE', #21138, #31077, #16193, .T. ) ;
#7191 = DIRECTION ( 'NONE',  ( 1.000000000000000000, 1.047444401652940007E-14, 0.000000000000000000 ) ) ;
#7192 = ORIENTED_EDGE ( 'NONE', *, *, #20116, .F. ) ;
#7193 = AXIS2_PLACEMENT_3D ( 'NONE', #2047, #21236, #25637 ) ;
#7194 = ADVANCED_FACE ( 'NONE', ( #13674 ), #3873, .F. ) ;
#7195 = CARTESIAN_POINT ( 'NONE',  ( 48.40000000000001990, -4.899999999999999467, -3.850000000000022737 ) ) ;
#7196 = AXIS2_PLACEMENT_3D ( 'NONE', #11642, #6884, #14314 ) ;
#7197 = CARTESIAN_POINT ( 'NONE',  ( -56.63452994616203284, 2.093608279459369510E-14, -3.600000000000201261 ) ) ;
#7198 = ORIENTED_EDGE ( 'NONE', *, *, #11207, .F. ) ;
#7199 = DIRECTION ( 'NONE',  ( -1.000000000000000000, 0.000000000000000000, 1.047444401652940007E-14 ) ) ;
#7200 = DIRECTION ( 'NONE',  ( 0.000000000000000000, 0.000000000000000000, -1.000000000000000000 ) ) ;
#7201 = CARTESIAN_POINT ( 'NONE',  ( 34.56269065792917417, 8.313757757582560970, 2.049999999999879030 ) ) ;
#7202 = ORIENTED_EDGE ( 'NONE', *, *, #967, .T. ) ;
#7203 = DIRECTION ( 'NONE',  ( 0.000000000000000000, -1.000000000000000000, -4.336808689942015369E-15 ) ) ;
#7204 = CARTESIAN_POINT ( 'NONE',  ( -62.09999999999997300, -2.687645153391445163, 0.1623166891292948111 ) ) ;
#7205 = CARTESIAN_POINT ( 'NONE',  ( 58.74160516400036158, -1.017053542743307171, -1.575205926126072908 ) ) ;
#7206 = ORIENTED_EDGE ( 'NONE', *, *, #18972, .T. ) ;
#7207 = DIRECTION ( 'NONE',  ( -1.000000000000000000, -3.054025858079668409E-16, 2.042474015755241579E-16 ) ) ;
#7208 = CARTESIAN_POINT ( 'NONE',  ( 57.05000000000001847, 0.7794871794871796045, 1.732743413496389939 ) ) ;
#7209 = EDGE_CURVE ( 'NONE', #31227, #21014, #22285, .T. ) ;
#7210 = FACE_OUTER_BOUND ( 'NONE', #22263, .T. ) ;
#7211 = CARTESIAN_POINT ( 'NONE',  ( 51.70000000000001705, -4.276948333784443612, 0.9210526315789470120 ) ) ;
#7212 = CARTESIAN_POINT ( 'NONE',  ( -44.49999999999997868, 1.400000000000009681, -1.540948453285710255E-13 ) ) ;
#7213 = CARTESIAN_POINT ( 'NONE',  ( 53.91678946233206915, 6.821600947619693933, 2.049999999999684963 ) ) ;
#7214 = PRODUCT_RELATED_PRODUCT_CATEGORY ( 'part', '', ( #22213 ) ) ;
#7215 = ORIENTED_EDGE ( 'NONE', *, *, #12507, .F. ) ;
#7216 = ORIENTED_EDGE ( 'NONE', *, *, #16363, .T. ) ;
#7217 = DIRECTION ( 'NONE',  ( 1.000000000000000000, 3.053848253006669023E-16, -2.042510438544995415E-16 ) ) ;
#7218 =( BOUNDED_SURFACE ( )  B_SPLINE_SURFACE ( 3, 2, ( 
 ( #11580, #6345, #25353 ),
 ( #16171, #3659, #22986 ),
 ( #8412, #28203, #3973 ),
 ( #15706, #16004, #1586 ),
 ( #25666, #13613, #13924 ),
 ( #8564, #18393, #23450 ),
 ( #11247, #11407, #23621 ),
 ( #1737, #27735, #15845 ),
 ( #8864, #9042, #23154 ),
 ( #30405, #25497, #18555 ) ),
 .UNSPECIFIED., .F., .F., .F. ) 
 B_SPLINE_SURFACE_WITH_KNOTS ( ( 4, 2, 2, 2, 4 ),
 ( 3, 3 ),
 ( 0.0001706658715692554269, 0.0002229276920778087870, 0.0002751895125863621470, 0.0003274513330949155613, 0.0003797131536034689214 ),
 ( 0.000000000000000000, 1.000000000000000000 ),
 .UNSPECIFIED. ) 
 GEOMETRIC_REPRESENTATION_ITEM ( )  RATIONAL_B_SPLINE_SURFACE ( (
 ( 1.000000000000000000, 0.7071067811865192621, 1.000000000000000000),
 ( 1.000000000000000000, 0.7375607040701905870, 1.000000000000000000),
 ( 1.000000000000000000, 0.7730431127427920268, 1.000000000000000000),
 ( 1.000000000000000000, 0.8321012486986795187, 1.000000000000000000),
 ( 1.000000000000000000, 0.8541932017409041844, 1.000000000000000000),
 ( 1.000000000000000000, 0.8545723906061826192, 1.000000000000000000),
 ( 1.000000000000000000, 0.8327032135051340989, 1.000000000000000000),
 ( 1.000000000000000000, 0.7734559727061557366, 1.000000000000000000),
 ( 1.000000000000000000, 0.7377766653997592794, 1.000000000000000000),
 ( 1.000000000000000000, 0.7071067811865198172, 1.000000000000000000) ) ) 
 REPRESENTATION_ITEM ( '' )  SURFACE ( )  );
#7219 = ORIENTED_EDGE ( 'NONE', *, *, #20376, .T. ) ;
#7220 = CARTESIAN_POINT ( 'NONE',  ( 52.10591853744708857, 8.701414215152928122, 2.049999999999818190 ) ) ;
#7221 = CARTESIAN_POINT ( 'NONE',  ( -59.53335481156722864, 0.8699069336946687603, -4.241846523238430144 ) ) ;
#7223 = DIRECTION ( 'NONE',  ( 0.000000000000000000, 0.000000000000000000, -1.000000000000000000 ) ) ;
#7222 = PLANE ( 'NONE',  #1901 ) ;
#7224 = ORIENTED_EDGE ( 'NONE', *, *, #6684, .F. ) ;
#7225 = ORIENTED_EDGE ( 'NONE', *, *, #25092, .F. ) ;
#7226 = FACE_OUTER_BOUND ( 'NONE', #5983, .T. ) ;
#7227 = VERTEX_POINT ( 'NONE', #4030 ) ;
#7228 = EDGE_CURVE ( 'NONE', #950, #9817, #9636, .T. ) ;
#7229 = CARTESIAN_POINT ( 'NONE',  ( 50.50000000000002842, -0.7374999999994747979, 1.362419564051435130E-16 ) ) ;
#7230 = ORIENTED_EDGE ( 'NONE', *, *, #1930, .T. ) ;
#7231 = CARTESIAN_POINT ( 'NONE',  ( -35.85663232820584767, 4.683225679163309785, 2.703237727951257607 ) ) ;
#7232 = EDGE_CURVE ( 'NONE', #4566, #6138, #20260, .T. ) ;
#7233 = ORIENTED_EDGE ( 'NONE', *, *, #1099, .T. ) ;
#7234 = DIRECTION ( 'NONE',  ( 1.000000000000000000, -0.000000000000000000, -0.000000000000000000 ) ) ;
#7235 = DIRECTION ( 'NONE',  ( 0.000000000000000000, -1.224646799147343593E-16, 1.000000000000000000 ) ) ;
#7236 = CARTESIAN_POINT ( 'NONE',  ( 57.00000000000001421, 0.6999999999999996225, -1.820027472320129736 ) ) ;
#7237 = CARTESIAN_POINT ( 'NONE',  ( -54.33155989232412253, -1.962990915244706924, -3.400000000000199751 ) ) ;
#7238 = DIRECTION ( 'NONE',  ( 1.000000000000000000, 0.000000000000000000, -1.047444401652940007E-14 ) ) ;
#7239 = DIRECTION ( 'NONE',  ( 0.000000000000000000, 0.000000000000000000, 1.000000000000000000 ) ) ;
#7240 = AXIS2_PLACEMENT_3D ( 'NONE', #27492, #5812, #2972 ) ;
#7241 = DIRECTION ( 'NONE',  ( 0.000000000000000000, 1.000000000000000000, 3.491481338843135722E-15 ) ) ;
#7242 = CARTESIAN_POINT ( 'NONE',  ( 58.75000000000002132, 6.153735859711025284E-13, 3.111507638930570854E-58 ) ) ;
#7243 = ORIENTED_EDGE ( 'NONE', *, *, #29449, .T. ) ;
#7244 = CARTESIAN_POINT ( 'NONE',  ( 64.95000000000001705, 1.401298464324817071E-42, -6.803151388735846952E-13 ) ) ;
#7245 = CARTESIAN_POINT ( 'NONE',  ( 58.65000000000000568, 1.372267738822026573, -1.278133834459896478 ) ) ;
#7246 = CARTESIAN_POINT ( 'NONE',  ( 53.81464057712626214, 5.799094425976102585, 1.402257142663977829 ) ) ;
#7247 = EDGE_LOOP ( 'NONE', ( #2201, #16881 ) ) ;
#7248 = CARTESIAN_POINT ( 'NONE',  ( -59.66183546925923764, -3.174920041538525251, -1.216504307364950854 ) ) ;
#7249 = ORIENTED_EDGE ( 'NONE', *, *, #28162, .T. ) ;
#7250 = CARTESIAN_POINT ( 'NONE',  ( 15.74504787372188730, 0.2143423494564743459, -5.404929114625646847 ) ) ;
#7252 = CARTESIAN_POINT ( 'NONE',  ( 47.10000000000000853, -3.550773357292059451, -2.049880134335985815 ) ) ;
#7251 = CARTESIAN_POINT ( 'NONE',  ( -57.65400635094607651, -3.399999999999988365, -0.9110272542660372563 ) ) ;
#7253 = EDGE_LOOP ( 'NONE', ( #2000, #3938, #27313, #18763 ) ) ;
#7254 = CARTESIAN_POINT ( 'NONE',  ( 50.50000000000002132, 2.428612866367529932E-14, 0.000000000000000000 ) ) ;
#7255 = EDGE_CURVE ( 'NONE', #16970, #21074, #9132, .T. ) ;
#7256 = CARTESIAN_POINT ( 'NONE',  ( 50.78793970012933556, 0.4223115601901949456, -0.9680023493207204899 ) ) ;
#7258 = CARTESIAN_POINT ( 'NONE',  ( 58.75000000000000711, 0.8495817349399600316, 1.671477153794648229 ) ) ;
#7257 = DIRECTION ( 'NONE',  ( 1.000000000000000000, 3.054025858079668409E-16, -2.042474015755241579E-16 ) ) ;
#7259 = VERTEX_POINT ( 'NONE', #22745 ) ;
#7260 = CARTESIAN_POINT ( 'NONE',  ( -56.68749999999997158, 3.238593381231846369, 2.874284765127021579 ) ) ;
#7261 = VECTOR ( 'NONE', #7286, 1000.000000000000000 ) ;
#7262 = DIRECTION ( 'NONE',  ( 0.000000000000000000, 0.000000000000000000, 1.000000000000000000 ) ) ;
#7263 = FACE_OUTER_BOUND ( 'NONE', #3363, .T. ) ;
#7264 = EDGE_CURVE ( 'NONE', #17419, #7270, #30860, .T. ) ;
#7265 = CIRCLE ( 'NONE', #29484, 3.524999999999996358 ) ;
#7266 = CARTESIAN_POINT ( 'NONE',  ( 16.00221665700883733, -3.629052419422202913, -4.014440194077229407 ) ) ;
#7267 = CARTESIAN_POINT ( 'NONE',  ( -61.34999999999997300, -2.588576612942594668, -0.5896429294185620007 ) ) ;
#7268 = CARTESIAN_POINT ( 'NONE',  ( -57.99999999999997868, 2.944486372867089141, 1.699999999999810774 ) ) ;
#7269 = DIRECTION ( 'NONE',  ( -1.000000000000000000, 0.000000000000000000, 1.047444401652940007E-14 ) ) ;
#7270 = VERTEX_POINT ( 'NONE', #18615 ) ;
#7271 = EDGE_CURVE ( 'NONE', #10898, #13515, #6878, .T. ) ;
#7272 = CARTESIAN_POINT ( 'NONE',  ( 47.54402780054770261, -3.873145847240279771, -1.345634385052774329 ) ) ;
#7273 = CARTESIAN_POINT ( 'NONE',  ( 15.49702763512084580, -3.012234853004051693, 4.239036759381619390 ) ) ;
#7274 =( BOUNDED_SURFACE ( )  B_SPLINE_SURFACE ( 3, 2, ( 
 ( #30870, #28177, #14079 ),
 ( #11564, #1898, #19007 ),
 ( #30714, #11862, #25953 ),
 ( #1570, #6492, #14234 ) ),
 .UNSPECIFIED., .F., .F., .F. ) 
 B_SPLINE_SURFACE_WITH_KNOTS ( ( 4, 4 ),
 ( 3, 3 ),
 ( 6.485788022086533158E-05, 0.0002376820751398764635 ),
 ( 0.000000000000000000, 1.000000000000000000 ),
 .UNSPECIFIED. ) 
 GEOMETRIC_REPRESENTATION_ITEM ( )  RATIONAL_B_SPLINE_SURFACE ( (
 ( 1.000000000000000000, 0.8191520442890480869, 1.000000000000000000),
 ( 1.000000000000000000, 0.8271241339490560396, 1.000000000000000000),
 ( 1.000000000000000000, 0.7737134445967045471, 1.000000000000000000),
 ( 1.000000000000000000, 0.7071067811865996422, 1.000000000000000000) ) ) 
 REPRESENTATION_ITEM ( '' )  SURFACE ( )  );
#7275 = DIRECTION ( 'NONE',  ( 0.000000000000000000, 0.000000000000000000, 1.000000000000000000 ) ) ;
#7276 = CARTESIAN_POINT ( 'NONE',  ( 27.27497440150130714, 5.311319583820425017, -1.950000000000095657 ) ) ;
#7277 = CARTESIAN_POINT ( 'NONE',  ( -62.05843735016853202, -2.684085269283162045, 0.2308628115494030242 ) ) ;
#7279 = CARTESIAN_POINT ( 'NONE',  ( 53.29837957427783124, 7.982236199023435397, -1.892846475469884604 ) ) ;
#7278 = LINE ( 'NONE', #24066, #18579 ) ;
#7280 = AXIS2_PLACEMENT_3D ( 'NONE', #16965, #14581, #7152 ) ;
#7281 = ADVANCED_FACE ( 'NONE', ( #28567 ), #16379, .T. ) ;
#7282 = DIRECTION ( 'NONE',  ( 3.491481338843133355E-15, 3.491481338843133355E-15, -1.000000000000000000 ) ) ;
#7284 = CARTESIAN_POINT ( 'NONE',  ( 31.59287277085072532, 7.495449159458786426, 1.424999999999890132 ) ) ;
#7283 = CARTESIAN_POINT ( 'NONE',  ( 68.00000000000002842, 1.401298464324817071E-42, -7.122621931239993559E-13 ) ) ;
#7285 = ORIENTED_EDGE ( 'NONE', *, *, #14514, .T. ) ;
#7286 = DIRECTION ( 'NONE',  ( 1.000000000000000000, -0.000000000000000000, -0.000000000000000000 ) ) ;
#7287 = UNCERTAINTY_MEASURE_WITH_UNIT (LENGTH_MEASURE( 1.000000000000000082E-05 ), #16339, 'distance_accuracy_value', 'NONE');
#7288 = CARTESIAN_POINT ( 'NONE',  ( 51.85262340636813860, -0.6891204047484754680, -1.750401715244590539 ) ) ;
#7290 = CARTESIAN_POINT ( 'NONE',  ( -44.49999999999996447, 1.514093959731561467, -3.183260039818548215 ) ) ;
#7289 = CARTESIAN_POINT ( 'NONE',  ( -44.49999999999999289, -6.938893903907228378E-14, 0.000000000000000000 ) ) ;
#7291 = CARTESIAN_POINT ( 'NONE',  ( 15.03925126672132961, -1.123735532908297863, -5.289358697221544503 ) ) ;
#7292 = ORIENTED_EDGE ( 'NONE', *, *, #17751, .T. ) ;
#7293 = CIRCLE ( 'NONE', #24974, 0.1500000000000001887 ) ;
#7294 = ORIENTED_EDGE ( 'NONE', *, *, #26442, .F. ) ;
#7295 = CARTESIAN_POINT ( 'NONE',  ( -57.40835481156722864, -3.238593381231842816, -2.874284765127022023 ) ) ;
#7296 = ADVANCED_FACE ( 'NONE', ( #23832 ), #4657, .F. ) ;
#7297 = ORIENTED_EDGE ( 'NONE', *, *, #5716, .T. ) ;
#7298 = DIRECTION ( 'NONE',  ( 0.000000000000000000, 0.000000000000000000, -1.000000000000000000 ) ) ;
#7299 = ADVANCED_FACE ( 'NONE', ( #19250 ), #27304, .T. ) ;
#7300 = CARTESIAN_POINT ( 'NONE',  ( -56.18749999999997868, 0.7533615035078125022, -3.673546848079176641 ) ) ;
#7301 = ORIENTED_EDGE ( 'NONE', *, *, #3707, .T. ) ;
#7302 = ADVANCED_FACE ( 'NONE', ( #14159 ), #30946, .T. ) ;
#7303 = CARTESIAN_POINT ( 'NONE',  ( -59.60130753818947369, -2.158066088952245387, 1.537948259120531125 ) ) ;
#7304 = ORIENTED_EDGE ( 'NONE', *, *, #4570, .T. ) ;
#7305 =( NAMED_UNIT ( * ) SI_UNIT ( $, .STERADIAN. ) SOLID_ANGLE_UNIT ( ) );
#7306 = DIRECTION ( 'NONE',  ( 0.000000000000000000, 0.000000000000000000, 1.000000000000000000 ) ) ;
#7307 = EDGE_LOOP ( 'NONE', ( #14058, #17165, #8718, #20081, #907, #2778, #29188, #21372, #16617, #26481, #6149, #26206, #1408, #24960, #3268, #15644, #13782 ) ) ;
#7308 =( NAMED_UNIT ( * ) SI_UNIT ( $, .STERADIAN. ) SOLID_ANGLE_UNIT ( ) );
#7309 = ORIENTED_EDGE ( 'NONE', *, *, #30775, .T. ) ;
#7310 = VECTOR ( 'NONE', #5694, 1000.000000000000000 ) ;
#7311 = ORIENTED_EDGE ( 'NONE', *, *, #19157, .F. ) ;
#7312 = CARTESIAN_POINT ( 'NONE',  ( -56.82202994616205416, -4.156921938165296204, -2.167734102480683039E-13 ) ) ;
#7313 = CARTESIAN_POINT ( 'NONE',  ( 51.38880644991419189, 3.878826100321112413, -2.050000000000178790 ) ) ;
#7314 = CARTESIAN_POINT ( 'NONE',  ( 49.00000000000004263, 0.7500000000000000000, 1.988246715072845561 ) ) ;
#7315 = DIRECTION ( 'NONE',  ( 0.000000000000000000, 0.000000000000000000, -1.000000000000000000 ) ) ;
#7316 = DIRECTION ( 'NONE',  ( 3.016910393003118404E-15, 0.000000000000000000, 1.000000000000000000 ) ) ;
#7318 = CARTESIAN_POINT ( 'NONE',  ( -36.26369610968609436, 0.2166734227622153230, -5.199999998324989825 ) ) ;
#7317 = DIRECTION ( 'NONE',  ( 0.000000000000000000, 0.5454670984320038052, 0.8381322357051842475 ) ) ;
#7319 = VECTOR ( 'NONE', #10994, 1000.000000000000000 ) ;
#7320 = EDGE_CURVE ( 'NONE', #11082, #4097, #1027, .T. ) ;
#7321 = CIRCLE ( 'NONE', #4282, 0.04999999999999988481 ) ;
#7322 = CARTESIAN_POINT ( 'NONE',  ( 48.45862863613067617, 1.344608935533184946, -3.858631320448700386 ) ) ;
#7324 = CARTESIAN_POINT ( 'NONE',  ( 51.23644008536121675, 1.080112125196981410, -1.214076932077873039 ) ) ;
#7323 = CARTESIAN_POINT ( 'NONE',  ( 51.25000000000001421, 1.163569835200988601E-28, -1.375000000000180300 ) ) ;
#7325 = EDGE_LOOP ( 'NONE', ( #18337, #30496, #30400, #25685 ) ) ;
#7326 = CARTESIAN_POINT ( 'NONE',  ( -44.49999999999997868, 2.624185894800584062, 0.06537116741875480252 ) ) ;
#7327 = ADVANCED_FACE ( 'NONE', ( #26354 ), #30355, .F. ) ;
#7328 = CIRCLE ( 'NONE', #8816, 0.04999999999999988481 ) ;
#7329 = CARTESIAN_POINT ( 'NONE',  ( -36.52757395963739384, -5.349060760730933062, -0.7993770229878666145 ) ) ;
#7331 = CARTESIAN_POINT ( 'NONE',  ( 50.30000000000001847, -1.426739617975179675, 3.843750000000022649 ) ) ;
#7330 = CARTESIAN_POINT ( 'NONE',  ( 48.41280093284956365, -1.295960864328790541, 3.889961360030774973 ) ) ;
#7332 = CARTESIAN_POINT ( 'NONE',  ( 47.11820097507338545, -4.249104741286833686, 1.767319601065233892 ) ) ;
#7333 = ORIENTED_EDGE ( 'NONE', *, *, #13390, .F. ) ;
#7334 = DIRECTION ( 'NONE',  ( 9.912705577010325352E-15, 0.000000000000000000, 1.000000000000000000 ) ) ;
#7335 = ORIENTED_EDGE ( 'NONE', *, *, #15635, .T. ) ;
#7336 = AXIS2_PLACEMENT_3D ( 'NONE', #30565, #23310, #18103 ) ;
#7337 = CARTESIAN_POINT ( 'NONE',  ( 50.93264768164066680, -4.319730106884873244, 1.256953381662059055 ) ) ;
#7338 = CARTESIAN_POINT ( 'NONE',  ( -58.13452994616202574, 2.093608279459371404E-14, -3.600000000000206146 ) ) ;
#7339 = EDGE_LOOP ( 'NONE', ( #10725, #26159, #29671, #22346, #25362, #19851 ) ) ;
#7340 = EDGE_LOOP ( 'NONE', ( #30787, #319, #5465, #11322 ) ) ;
#7341 = CARTESIAN_POINT ( 'NONE',  ( 15.45522337368514343, 4.885888067249533506, 1.790336215468755654 ) ) ;
#7342 = ORIENTED_EDGE ( 'NONE', *, *, #17433, .F. ) ;
#7343 = CARTESIAN_POINT ( 'NONE',  ( 50.78793970012933556, 0.4223115601901947791, 0.9680023493207204899 ) ) ;
#7344 = CARTESIAN_POINT ( 'NONE',  ( -56.75952994616203995, -3.117691453623963938, -1.800000000000212763 ) ) ;
#7345 = VERTEX_POINT ( 'NONE', #24142 ) ;
#7346 = FACE_OUTER_BOUND ( 'NONE', #14535, .T. ) ;
#7347 = CARTESIAN_POINT ( 'NONE',  ( -44.49999999999997868, -1.399999999999992806, -1.638709930773317737E-13 ) ) ;
#7348 = AXIS2_PLACEMENT_3D ( 'NONE', #21289, #21129, #16836 ) ;
#7349 = CARTESIAN_POINT ( 'NONE',  ( 29.24156347412778700, 6.028130183534497810, 1.949999999999896261 ) ) ;
#7350 = ORIENTED_EDGE ( 'NONE', *, *, #10583, .T. ) ;
#7351 = DIRECTION ( 'NONE',  ( 0.000000000000000000, 1.000000000000000000, 4.336808689942015369E-15 ) ) ;
#7352 = CARTESIAN_POINT ( 'NONE',  ( 53.31748909063354347, 8.199041228893841904, -2.050000000000185452 ) ) ;
#7354 = LINE ( 'NONE', #24443, #25862 ) ;
#7353 = CIRCLE ( 'NONE', #14903, 0.1000000000000000472 ) ;
#7355 = DIRECTION ( 'NONE',  ( 0.9992009587217894895, -0.008029435056736644594, 0.03915318968010782219 ) ) ;
#7356 = DIRECTION ( 'NONE',  ( 0.000000000000000000, 0.3099561728523109738, -0.9507508458638090909 ) ) ;
#7358 = DIRECTION ( 'NONE',  ( 0.000000000000000000, 0.000000000000000000, -1.000000000000000000 ) ) ;
#7357 = DIRECTION ( 'NONE',  ( 1.000000000000000000, -0.000000000000000000, -0.000000000000000000 ) ) ;
#7359 = EDGE_CURVE ( 'NONE', #16552, #11068, #30080, .T. ) ;
#7360 = CARTESIAN_POINT ( 'NONE',  ( -67.99999999999997158, -3.266925685480240183E-16, 2.202315069465531314E-15 ) ) ;
#7361 = ADVANCED_FACE ( 'NONE', ( #9101 ), #23680, .T. ) ;
#7362 = DIRECTION ( 'NONE',  ( 0.000000000000000000, 0.3529411764705882026, 0.9356455129756979794 ) ) ;
#7363 = CARTESIAN_POINT ( 'NONE',  ( 51.87416143049284756, 8.598705507415683513, 1.949999999999818767 ) ) ;
#7364 = ADVANCED_FACE ( 'NONE', ( #16864 ), #13637, .T. ) ;
#7365 = ORIENTED_EDGE ( 'NONE', *, *, #13003, .F. ) ;
#7366 = AXIS2_PLACEMENT_3D ( 'NONE', #24727, #3041, #22690 ) ;
#7367 = ORIENTED_EDGE ( 'NONE', *, *, #3362, .T. ) ;
#7368 = CARTESIAN_POINT ( 'NONE',  ( 51.87895135909221267, 0.03408243259258914720, -4.372659797885439126 ) ) ;
#7369 = ORIENTED_EDGE ( 'NONE', *, *, #23352, .F. ) ;
#7370 = CARTESIAN_POINT ( 'NONE',  ( 52.80968221184929234, 4.034333029853865327, 2.049999999999815969 ) ) ;
#7371 = CARTESIAN_POINT ( 'NONE',  ( -56.42292740578360366, 1.073804522883522239, 3.225979517392336238 ) ) ;
#7373 = CARTESIAN_POINT ( 'NONE',  ( 51.80000000000001847, -3.726179070414207928, -1.100000000000000089 ) ) ;
#7372 = DIRECTION ( 'NONE',  ( 0.000000000000000000, 0.000000000000000000, 1.000000000000000000 ) ) ;
#7374 = ORIENTED_EDGE ( 'NONE', *, *, #10472, .F. ) ;
#7375 = CIRCLE ( 'NONE', #22053, 4.800000000000000711 ) ;
#7376 = ORIENTED_EDGE ( 'NONE', *, *, #21836, .F. ) ;
#7377 = CYLINDRICAL_SURFACE ( 'NONE', #1748, 0.05000000000000143219 ) ;
#7378 = ORIENTED_EDGE ( 'NONE', *, *, #7735, .T. ) ;
#7379 = AXIS2_PLACEMENT_3D ( 'NONE', #14315, #23985, #2284 ) ;
#7380 = EDGE_CURVE ( 'NONE', #29298, #29220, #16469, .T. ) ;
#7381 = CARTESIAN_POINT ( 'NONE',  ( 47.10000000000002274, -4.179189514726506793, -1.000000000000000000 ) ) ;
#7382 = ORIENTED_EDGE ( 'NONE', *, *, #9759, .F. ) ;
#7383 = CARTESIAN_POINT ( 'NONE',  ( 58.65000000000003411, -1.571497941946429444, 1.022750809560281970 ) ) ;
#7384 = AXIS2_PLACEMENT_3D ( 'NONE', #22164, #7879, #17388 ) ;
#7385 =( REPRESENTATION_RELATIONSHIP ('NONE','NONE', #7047, #30888 ) REPRESENTATION_RELATIONSHIP_WITH_TRANSFORMATION ( #18370 )SHAPE_REPRESENTATION_RELATIONSHIP( ) );
#7386 = DIRECTION ( 'NONE',  ( 1.000000000000000000, -0.000000000000000000, -1.047444401652940007E-14 ) ) ;
#7387 = CARTESIAN_POINT ( 'NONE',  ( -69.22071067811863543, 0.4218824419643703583, -2.057186234924337054 ) ) ;
#7388 = DIRECTION ( 'NONE',  ( -8.673617379883787770E-15, 0.000000000000000000, -1.000000000000000000 ) ) ;
#7389 = CARTESIAN_POINT ( 'NONE',  ( -61.13452994616202574, 2.093608279459375190E-14, -3.600000000000216804 ) ) ;
#7390 = CARTESIAN_POINT ( 'NONE',  ( 52.16611735465125577, 8.588510181879298599, -2.050000000000181011 ) ) ;
#7391 = AXIS2_PLACEMENT_3D ( 'NONE', #2172, #14357, #24028 ) ;
#7392 = AXIS2_PLACEMENT_3D ( 'NONE', #3178, #801, #10468 ) ;
#7393 = AXIS2_PLACEMENT_3D ( 'NONE', #13325, #30127, #10525 ) ;
#7394 = CARTESIAN_POINT ( 'NONE',  ( 31.30720621464603326, 7.411182539856417506, 1.549999999999890798 ) ) ;
#7395 = DIRECTION ( 'NONE',  ( 1.000000000000000000, -0.000000000000000000, -1.047444401652940007E-14 ) ) ;
#7396 = STYLED_ITEM ( 'NONE', ( #18274 ), #15704 ) ;
#7397 = AXIS2_PLACEMENT_3D ( 'NONE', #30281, #8591, #27910 ) ;
#7398 = LINE ( 'NONE', #9480, #27087 ) ;
#7399 = EDGE_CURVE ( 'NONE', #21138, #3014, #4178, .T. ) ;
#7400 = AXIS2_PLACEMENT_3D ( 'NONE', #14753, #24414, #17293 ) ;
#7401 =( BOUNDED_CURVE ( )  B_SPLINE_CURVE ( 3, ( #14499, #16580, #16737, #4531 ),
 .UNSPECIFIED., .F., .T. ) 
 B_SPLINE_CURVE_WITH_KNOTS ( ( 4, 4 ),
 ( 3.141592653589793560, 4.712388980384687898 ),
 .UNSPECIFIED. ) 
 CURVE ( )  GEOMETRIC_REPRESENTATION_ITEM ( )  RATIONAL_B_SPLINE_CURVE ( ( 1.000000000000000000, 0.8047378541243654926, 0.8047378541243654926, 1.000000000000000000 ) ) 
 REPRESENTATION_ITEM ( '' )  );
#7402 = STYLED_ITEM ( 'NONE', ( #9744 ), #25849 ) ;
#7403 = DIRECTION ( 'NONE',  ( -1.000000000000000000, -3.054025858079668409E-16, 2.042474015755241579E-16 ) ) ;
#7404 = VERTEX_POINT ( 'NONE', #21156 ) ;
#7405 = CARTESIAN_POINT ( 'NONE',  ( -71.44999999999998863, -1.380331489585512972E-15, 2.906968604901091669E-15 ) ) ;
#7407 = CARTESIAN_POINT ( 'NONE',  ( -54.48167032960165557, 1.510995100284905579, 3.307167554963766243 ) ) ;
#7406 = LINE ( 'NONE', #7706, #13038 ) ;
#7408 = DIRECTION ( 'NONE',  ( 0.000000000000000000, -1.224646799147353207E-16, 1.000000000000000000 ) ) ;
#7409 = ORIENTED_EDGE ( 'NONE', *, *, #20691, .T. ) ;
#7410 = CARTESIAN_POINT ( 'NONE',  ( -36.92405921417686443, -5.098435263432280706, 1.807398698456160302 ) ) ;
#7411 = ORIENTED_EDGE ( 'NONE', *, *, #10551, .T. ) ;
#7412 = CONICAL_SURFACE ( 'NONE', #22667, 2.250000000000000444, 0.7853981633974536081 ) ;
#7413 = CARTESIAN_POINT ( 'NONE',  ( 15.03925126672127810, 0.4576450603547064233, -5.200000000000000178 ) ) ;
#7414 = CARTESIAN_POINT ( 'NONE',  ( -36.92362342067168868, -5.092377074781566648, 1.825725187625063972 ) ) ;
#7416 = DIRECTION ( 'NONE',  ( 0.000000000000000000, 0.000000000000000000, -1.000000000000000000 ) ) ;
#7415 = CARTESIAN_POINT ( 'NONE',  ( 58.66118217212531505, 0.9228675180758563190, -1.632243256842949464 ) ) ;
#7417 = VERTEX_POINT ( 'NONE', #10184 ) ;
#7418 = VECTOR ( 'NONE', #28676, 1000.000000000000000 ) ;
#7419 = DIRECTION ( 'NONE',  ( 0.000000000000000000, -1.000000000000000000, 0.000000000000000000 ) ) ;
#7420 = AXIS2_PLACEMENT_3D ( 'NONE', #3442, #28243, #13082 ) ;
#7421 = ADVANCED_FACE ( 'NONE', ( #2909 ), #7115, .T. ) ;
#7422 = CARTESIAN_POINT ( 'NONE',  ( 50.30000000000001847, -1.409787217987148233, -3.850000000000022737 ) ) ;
#7424 = CARTESIAN_POINT ( 'NONE',  ( -54.49131719536980967, -1.521332553059528081, -4.044684194243342468 ) ) ;
#7423 = LINE ( 'NONE', #12306, #29713 ) ;
#7425 = ORIENTED_EDGE ( 'NONE', *, *, #16880, .T. ) ;
#7426 = CARTESIAN_POINT ( 'NONE',  ( -60.24999999999996447, -2.489203624310586171, 2.804704140674917578 ) ) ;
#7427 = DIRECTION ( 'NONE',  ( 0.000000000000000000, -0.2008964009354146929, 0.9796124928211140670 ) ) ;
#7428 = DIRECTION ( 'NONE',  ( 3.002035892788117459E-16, -0.9996898646859344595, -0.02490330187381124133 ) ) ;
#7429 = VECTOR ( 'NONE', #9164, 1000.000000000000114 ) ;
#7430 = CARTESIAN_POINT ( 'NONE',  ( 15.97944027357902463, -2.710596767400041518, -4.680923748383032823 ) ) ;
#7431 = AXIS2_PLACEMENT_3D ( 'NONE', #25923, #14040, #1686 ) ;
#7432 = CARTESIAN_POINT ( 'NONE',  ( -54.93749999999997158, -4.108500314926507357, 1.367561758111405901 ) ) ;
#7433 = DIRECTION ( 'NONE',  ( -1.000000000000000000, 0.000000000000000000, 3.491481338843133355E-15 ) ) ;
#7434 = VECTOR ( 'NONE', #24410, 1000.000000000000000 ) ;
#7435 = VECTOR ( 'NONE', #10518, 1000.000000000000000 ) ;
#7436 = CARTESIAN_POINT ( 'NONE',  ( -54.49999999999997868, 4.900000000000003020, 0.000000000000000000 ) ) ;
#7437 = EDGE_LOOP ( 'NONE', ( #3781, #27068, #1601, #28594 ) ) ;
#7438 = DIRECTION ( 'NONE',  ( 0.000000000000000000, 0.000000000000000000, 1.000000000000000000 ) ) ;
#7439 = AXIS2_PLACEMENT_3D ( 'NONE', #13270, #18064, #25633 ) ;
#7440 = CARTESIAN_POINT ( 'NONE',  ( 33.97008042022903851, 8.187964135517418640, -1.950000000000118527 ) ) ;
#7441 = TOROIDAL_SURFACE ( 'NONE', #25128, 4.199999999999993072, 0.1000000000000000056 ) ;
#7442 = CARTESIAN_POINT ( 'NONE',  ( -59.69999999999997442, 8.366749974758454467E-15, -2.120534355533670266E-13 ) ) ;
#7443 = ADVANCED_FACE ( 'NONE', ( #7512 ), #7656, .T. ) ;
#7444 = AXIS2_PLACEMENT_3D ( 'NONE', #21979, #2658, #9488 ) ;
#7445 = CARTESIAN_POINT ( 'NONE',  ( 52.10570363851881837, 8.590619875341600320, -1.949999390396187637 ) ) ;
#7446 = CARTESIAN_POINT ( 'NONE',  ( 61.23837541685315244, -0.8927489269147697026, 1.767200183694116244 ) ) ;
#7448 = DIRECTION ( 'NONE',  ( 9.188255586753834161E-15, -0.8381322357045576377, -0.5454670984329669237 ) ) ;
#7447 = CARTESIAN_POINT ( 'NONE',  ( 56.95000000000001705, 0.7137254901960785602, -2.500119182087999548 ) ) ;
#7449 = EDGE_LOOP ( 'NONE', ( #4839, #25390, #9499, #27267 ) ) ;
#7450 = CIRCLE ( 'NONE', #29195, 0.05000000000000143219 ) ;
#7451 = CARTESIAN_POINT ( 'NONE',  ( 58.66118217212473240, -1.806736155626957663, 0.5016043952914784887 ) ) ;
#7452 = AXIS2_PLACEMENT_3D ( 'NONE', #24503, #25137, #2814 ) ;
#7453 = CARTESIAN_POINT ( 'NONE',  ( 50.25000000000003553, -1.666164585742576421, -1.106298139390194724 ) ) ;
#7454 = B_SPLINE_CURVE_WITH_KNOTS ( 'NONE', 3,
 ( #14629, #20007, #5601, #24295 ),
 .UNSPECIFIED., .F., .F.,
 ( 4, 4 ),
 ( 0.5073942967076801036, 0.8047316756486366796 ),
 .UNSPECIFIED. ) ;
#7456 = CARTESIAN_POINT ( 'NONE',  ( 58.64999999999999858, 1.932246131437592052, 0.4087173687853762338 ) ) ;
#7455 = CARTESIAN_POINT ( 'NONE',  ( 15.94709373951305764, -2.670851142931433664, -4.702170608191262424 ) ) ;
#7457 = DIRECTION ( 'NONE',  ( 0.000000000000000000, 0.000000000000000000, -1.000000000000000000 ) ) ;
#7458 = ORIENTED_EDGE ( 'NONE', *, *, #10557, .T. ) ;
#7459 = ORIENTED_EDGE ( 'NONE', *, *, #26901, .T. ) ;
#7460 = DIRECTION ( 'NONE',  ( 0.000000000000000000, 0.000000000000000000, 1.000000000000000000 ) ) ;
#7461 = VERTEX_POINT ( 'NONE', #26821 ) ;
#7462 = CARTESIAN_POINT ( 'NONE',  ( 51.76980060221182356, -4.166995010554928491, 1.027517533905028868 ) ) ;
#7463 = CARTESIAN_POINT ( 'NONE',  ( -54.36042740578361077, 3.725040285533371076, -1.239922660687676537 ) ) ;
#7464 = AXIS2_PLACEMENT_3D ( 'NONE', #25913, #16593, #14028 ) ;
#7465 = ORIENTED_EDGE ( 'NONE', *, *, #26186, .F. ) ;
#7466 = CARTESIAN_POINT ( 'NONE',  ( -36.50489844130356687, -5.244794032782665205, -1.329291831544206381 ) ) ;
#7467 = ORIENTED_EDGE ( 'NONE', *, *, #18154, .F. ) ;
#7468 =( LENGTH_UNIT ( ) NAMED_UNIT ( * ) SI_UNIT ( .MILLI., .METRE. ) );
#7469 = AXIS2_PLACEMENT_3D ( 'NONE', #17097, #26105, #31171 ) ;
#7470 = CARTESIAN_POINT ( 'NONE',  ( -60.89405989232410121, 2.944486372867106461, -1.700000000000203348 ) ) ;
#7471 = TOROIDAL_SURFACE ( 'NONE', #2428, 2.549999999999999822, 0.05000000000000000278 ) ;
#7472 = ORIENTED_EDGE ( 'NONE', *, *, #8113, .F. ) ;
#7473 = EDGE_CURVE ( 'NONE', #2793, #29835, #29834, .T. ) ;
#7474 = ORIENTED_EDGE ( 'NONE', *, *, #20115, .F. ) ;
#7475 = AXIS2_PLACEMENT_3D ( 'NONE', #14024, #23714, #1674 ) ;
#7476 = CARTESIAN_POINT ( 'NONE',  ( -58.63452994616204705, 3.117691453623979481, 1.799999999999803757 ) ) ;
#7477 = AXIS2_PLACEMENT_3D ( 'NONE', #14487, #9606, #18943 ) ;
#7478 = CARTESIAN_POINT ( 'NONE',  ( 53.13232117966330037, 4.211086031869615276, -2.050000000000185008 ) ) ;
#7479 = CARTESIAN_POINT ( 'NONE',  ( 60.88100035777595309, -0.5130564158037707045, -1.858165151418244010 ) ) ;
#7480 = CARTESIAN_POINT ( 'NONE',  ( 51.76237124553680502, -4.256129153948959853, -1.015733033895005688 ) ) ;
#7481 = ADVANCED_FACE ( 'NONE', ( #5270 ), #7623, .T. ) ;
#7483 = CARTESIAN_POINT ( 'NONE',  ( -61.36385676688671253, -2.559112712334371764, -0.8120304950550095713 ) ) ;
#7482 = CARTESIAN_POINT ( 'NONE',  ( 47.00000000000002132, 2.428612866367529932E-14, -1.640996229256273308E-13 ) ) ;
#7484 = EDGE_CURVE ( 'NONE', #4931, #29991, #28876, .T. ) ;
#7485 = VECTOR ( 'NONE', #9844, 999.9999999999998863 ) ;
#7486 = EDGE_CURVE ( 'NONE', #22071, #22328, #12553, .T. ) ;
#7487 = AXIS2_PLACEMENT_3D ( 'NONE', #30027, #8343, #5993 ) ;
#7488 = DIRECTION ( 'NONE',  ( 1.000000000000000000, 3.053848253006669023E-16, -2.042510438544995415E-16 ) ) ;
#7489 = CARTESIAN_POINT ( 'NONE',  ( -57.83155989232412253, 3.400000000000007905, -1.837192174579415629E-13 ) ) ;
#7491 = DIRECTION ( 'NONE',  ( -3.491481338843133355E-15, -3.491481338843133355E-15, 1.000000000000000000 ) ) ;
#7490 = CARTESIAN_POINT ( 'NONE',  ( 54.43308742068420969, -0.0001827659102894963578, -4.369367483123359541 ) ) ;
#7492 = ORIENTED_EDGE ( 'NONE', *, *, #4482, .F. ) ;
#7494 = CARTESIAN_POINT ( 'NONE',  ( 58.75000000000003553, -1.469015551795666452, 1.320082690054176666 ) ) ;
#7493 = TOROIDAL_SURFACE ( 'NONE', #25100, 4.199999999999993072, 0.1000000000000000056 ) ;
#7495 = CARTESIAN_POINT ( 'NONE',  ( 58.75000000000002132, 6.153735859711025284E-13, 3.111507638930570854E-58 ) ) ;
#7497 = DIRECTION ( 'NONE',  ( 1.000000000000000000, 0.000000000000000000, -1.047444401652940007E-14 ) ) ;
#7496 = CARTESIAN_POINT ( 'NONE',  ( 48.38568300895507690, -1.130504494894903456, 3.941663789486468339 ) ) ;
#7498 = CARTESIAN_POINT ( 'NONE',  ( 57.00000000000000711, 0.7137254901960808917, 2.500119182088006209 ) ) ;
#7499 = EDGE_LOOP ( 'NONE', ( #27625, #26782, #20400, #2770 ) ) ;
#7500 = CARTESIAN_POINT ( 'NONE',  ( 51.45655683570189609, 0.9591657938401613182, 1.611094652690528317 ) ) ;
#7501 = EDGE_CURVE ( 'NONE', #20905, #9490, #30366, .T. ) ;
#7502 = VERTEX_POINT ( 'NONE', #24588 ) ;
#7503 = CARTESIAN_POINT ( 'NONE',  ( 60.98985426489756634, 0.5466942006297351719, -1.538695758318366691 ) ) ;
#7504 = B_SPLINE_CURVE_WITH_KNOTS ( 'NONE', 3,
 ( #10997, #13054, #22737, #1033, #14265, #16967, #26615, #30302, #8611, #13514 ),
 .UNSPECIFIED., .F., .F.,
 ( 4, 2, 2, 2, 4 ),
 ( 0.000000000000000000, 0.0003923015305839671263, 0.0007846030611679342525, 0.001176904591751901270, 0.001569206122335868505 ),
 .UNSPECIFIED. ) ;
#7505 = EDGE_LOOP ( 'NONE', ( #5249, #30293, #6634, #968 ) ) ;
#7506 = VERTEX_POINT ( 'NONE', #29201 ) ;
#7507 = DIRECTION ( 'NONE',  ( 0.000000000000000000, -0.9996898646859343485, -0.02490330187381124133 ) ) ;
#7508 = ORIENTED_EDGE ( 'NONE', *, *, #6290, .T. ) ;
#7509 = DIRECTION ( 'NONE',  ( 0.000000000000000000, 0.6683962987610957418, 0.7438053426821212843 ) ) ;
#7510 = CARTESIAN_POINT ( 'NONE',  ( -57.25952994616203995, 3.117691453623994580, -1.800000000000189671 ) ) ;
#7511 = ORIENTED_EDGE ( 'NONE', *, *, #29422, .F. ) ;
#7512 = FACE_OUTER_BOUND ( 'NONE', #12613, .T. ) ;
#7513 = EDGE_CURVE ( 'NONE', #20962, #21492, #2748, .T. ) ;
#7514 = AXIS2_PLACEMENT_3D ( 'NONE', #23925, #11406, #3972 ) ;
#7515 = CARTESIAN_POINT ( 'NONE',  ( 32.57869118518240015, 7.908463454149416982, 2.049999999999884803 ) ) ;
#7516 = ORIENTED_EDGE ( 'NONE', *, *, #24684, .T. ) ;
#7517 = AXIS2_PLACEMENT_3D ( 'NONE', #29647, #673, #5600 ) ;
#7518 = CARTESIAN_POINT ( 'NONE',  ( 63.50000000000000000, 3.214697847761892795E-16, -2.625000000000663913 ) ) ;
#7519 = EDGE_CURVE ( 'NONE', #7079, #7997, #12394, .T. ) ;
#7520 = DIRECTION ( 'NONE',  ( 2.614375865348241018E-16, -0.2008964009354148039, 0.9796124928211140670 ) ) ;
#7521 = CARTESIAN_POINT ( 'NONE',  ( 58.65844932252345245, -0.9087029769943339996, -1.640171707772822396 ) ) ;
#7522 = DIRECTION ( 'NONE',  ( 0.000000000000000000, -1.000000000000000000, 0.000000000000000000 ) ) ;
#7523 = FACE_OUTER_BOUND ( 'NONE', #14740, .T. ) ;
#7524 = APPLICATION_CONTEXT ( 'automotive_design' ) ;
#7526 = DIRECTION ( 'NONE',  ( -0.000000000000000000, -2.168404344971007882E-16, -1.000000000000000000 ) ) ;
#7525 = CARTESIAN_POINT ( 'NONE',  ( -36.04581030752770943, -3.779372845003824644, 3.883777290285136186 ) ) ;
#7527 = EDGE_CURVE ( 'NONE', #29305, #7081, #20791, .T. ) ;
#7528 = EDGE_CURVE ( 'NONE', #13195, #13128, #7454, .T. ) ;
#7529 = FACE_OUTER_BOUND ( 'NONE', #16183, .T. ) ;
#7530 = FACE_OUTER_BOUND ( 'NONE', #7570, .T. ) ;
#7531 = DIRECTION ( 'NONE',  ( 0.000000000000000000, -0.3099561728522105541, -0.9507508458638417315 ) ) ;
#7532 = ORIENTED_EDGE ( 'NONE', *, *, #28171, .F. ) ;
#7533 = MECHANICAL_DESIGN_GEOMETRIC_PRESENTATION_REPRESENTATION (  '', ( #28252 ), #15110 ) ;
#7534 = ORIENTED_EDGE ( 'NONE', *, *, #6125, .T. ) ;
#7535 = AXIS2_PLACEMENT_3D ( 'NONE', #6860, #16526, #26183 ) ;
#7536 = ORIENTED_EDGE ( 'NONE', *, *, #18504, .T. ) ;
#7537 = CARTESIAN_POINT ( 'NONE',  ( 47.00000000000002132, 1.391941090707534023, -3.750000000000022649 ) ) ;
#7538 = CARTESIAN_POINT ( 'NONE',  ( -54.36042740578361077, 3.725040285533371076, -1.239922660687676537 ) ) ;
#7540 = DIRECTION ( 'NONE',  ( 0.000000000000000000, 0.000000000000000000, 1.000000000000000000 ) ) ;
#7539 = PLANE ( 'NONE',  #27686 ) ;
#7541 = ORIENTED_EDGE ( 'NONE', *, *, #25840, .F. ) ;
#7542 = VERTEX_POINT ( 'NONE', #4974 ) ;
#7543 = CARTESIAN_POINT ( 'NONE',  ( -55.90835481156722864, -3.238593381231841928, -2.874284765127022467 ) ) ;
#7544 = VERTEX_POINT ( 'NONE', #29649 ) ;
#7545 = CARTESIAN_POINT ( 'NONE',  ( 34.56702326949726256, 8.213851659285209550, 1.949999999999879163 ) ) ;
#7546 = ORIENTED_EDGE ( 'NONE', *, *, #2490, .F. ) ;
#7547 = CARTESIAN_POINT ( 'NONE',  ( 29.24156346101471016, 6.028130203021968114, -2.050000000000362199 ) ) ;
#7548 = VERTEX_POINT ( 'NONE', #21935 ) ;
#7549 = DIRECTION ( 'NONE',  ( 0.9992009587217894895, 0.008029435056737250012, -0.03915318968010823159 ) ) ;
#7550 = ADVANCED_FACE ( 'NONE', ( #29346 ), #9735, .F. ) ;
#7551 = DIRECTION ( 'NONE',  ( 0.000000000000000000, 1.000000000000000000, 3.491481338843137694E-15 ) ) ;
#7552 = EDGE_CURVE ( 'NONE', #17419, #25469, #15249, .T. ) ;
#7553 = CARTESIAN_POINT ( 'NONE',  ( 15.49676243306307732, -4.927920137446233362, -1.660974799722084061 ) ) ;
#7554 = ADVANCED_FACE ( 'NONE', ( #19397 ), #3074, .F. ) ;
#7555 = CARTESIAN_POINT ( 'NONE',  ( -56.33155989232412253, 3.925981830489463142, -1.858639063162819723E-13 ) ) ;
#7556 = CARTESIAN_POINT ( 'NONE',  ( 51.87765138016307986, 8.698644590117595499, -2.050000000000180123 ) ) ;
#7557 =( GEOMETRIC_REPRESENTATION_CONTEXT ( 3 ) GLOBAL_UNCERTAINTY_ASSIGNED_CONTEXT ( ( #25318 ) ) GLOBAL_UNIT_ASSIGNED_CONTEXT ( ( #9836, #7160, #4928 ) ) REPRESENTATION_CONTEXT ( 'NONE', 'WORKASPACE' ) );
#7558 = TOROIDAL_SURFACE ( 'NONE', #28276, 2.729289321881338548, 0.05000000000000000278 ) ;
#7559 = DIRECTION ( 'NONE',  ( -0.8262273428075421755, -0.5633368246415177971, 0.000000000000000000 ) ) ;
#7560 = CARTESIAN_POINT ( 'NONE',  ( 58.75000000000002132, 6.153735859711025284E-13, 3.111507638930570854E-58 ) ) ;
#7561 = CARTESIAN_POINT ( 'NONE',  ( -71.49999999999998579, -1.395601618875910821E-15, 2.917180974979867506E-15 ) ) ;
#7562 = DIRECTION ( 'NONE',  ( 0.000000000000000000, -0.1576190026614809614, 0.9875000000000001554 ) ) ;
#7563 = ORIENTED_EDGE ( 'NONE', *, *, #2544, .F. ) ;
#7564 = CARTESIAN_POINT ( 'NONE',  ( 61.25000000000000711, 1.470078920827461166, 1.470078920828533420 ) ) ;
#7565 = CARTESIAN_POINT ( 'NONE',  ( 51.40674769956039114, -0.9873535814794003329, -1.422142864483648461 ) ) ;
#7566 = CARTESIAN_POINT ( 'NONE',  ( 54.07864988756197988, 6.687439357893800285, 2.033314590869161442 ) ) ;
#7567 = ORIENTED_EDGE ( 'NONE', *, *, #16202, .T. ) ;
#7568 = DIRECTION ( 'NONE',  ( 0.000000000000000000, -0.4102564102564100201, 0.9119702176296790030 ) ) ;
#7569 = AXIS2_PLACEMENT_3D ( 'NONE', #16700, #23969, #17587 ) ;
#7570 = EDGE_LOOP ( 'NONE', ( #30227, #5651 ) ) ;
#7571 = FILL_AREA_STYLE ('',( #12300 ) ) ;
#7572 = DIRECTION ( 'NONE',  ( 0.000000000000000000, 0.000000000000000000, -1.000000000000000000 ) ) ;
#7574 = CARTESIAN_POINT ( 'NONE',  ( 58.65000000000004121, -1.782657835994225781, -0.5811678240974800236 ) ) ;
#7573 = CARTESIAN_POINT ( 'NONE',  ( 58.66107449606953139, 0.9081280691414966855, 1.640741681270895036 ) ) ;
#7575 = ORIENTED_EDGE ( 'NONE', *, *, #11711, .F. ) ;
#7576 = LINE ( 'NONE', #2520, #27514 ) ;
#7577 = AXIS2_PLACEMENT_3D ( 'NONE', #18021, #3606, #4071 ) ;
#7578 = CIRCLE ( 'NONE', #16697, 0.1000000000000001443 ) ;
#7579 = DIRECTION ( 'NONE',  ( 0.000000000000000000, 0.000000000000000000, -1.000000000000000000 ) ) ;
#7580 = AXIS2_PLACEMENT_3D ( 'NONE', #11905, #16507, #7170 ) ;
#7582 = DIRECTION ( 'NONE',  ( 0.000000000000000000, -1.000000000000000000, 0.000000000000000000 ) ) ;
#7581 = CARTESIAN_POINT ( 'NONE',  ( -57.89405989232411542, 2.944486372867110902, -1.700000000000184697 ) ) ;
#7583 = ORIENTED_EDGE ( 'NONE', *, *, #23686, .T. ) ;
#7584 = CARTESIAN_POINT ( 'NONE',  ( -58.12499999999997158, 1.184343223768590248, 3.558065644182725418 ) ) ;
#7585 = DIRECTION ( 'NONE',  ( -1.040834085586084257E-14, 0.000000000000000000, -1.000000000000000000 ) ) ;
#7586 = DIRECTION ( 'NONE',  ( -1.000000000000000000, -1.047444401652940007E-14, -0.000000000000000000 ) ) ;
#7587 = CIRCLE ( 'NONE', #5052, 0.2499999999999997780 ) ;
#7588 = EDGE_CURVE ( 'NONE', #17883, #30573, #17176, .T. ) ;
#7589 = CARTESIAN_POINT ( 'NONE',  ( 58.64999999999992752, -1.972190280207374968, 0.1053114364786527507 ) ) ;
#7590 = CARTESIAN_POINT ( 'NONE',  ( 58.50000000000001421, 0.000000000000000000, 0.000000000000000000 ) ) ;
#7591 = EDGE_LOOP ( 'NONE', ( #14875, #8237, #15722, #18107 ) ) ;
#7592 =( BOUNDED_SURFACE ( )  B_SPLINE_SURFACE ( 2, 3, ( 
 ( #17475, #19401, #10340, #29656, #27129, #5448, #24756, #3066, #29043, #20013, #12712, #17645, #4812, #7352, #21940, #9885, #29205, #17182 ),
 ( #26827, #27602, #5637, #2494, #19756, #24475, #2786, #12149, #570, #20061, #22130, #3099, #26858, #24792, #2952, #29242, #7841, #19604 ),
 ( #29385, #22426, #17516, #15288, #12597, #2644, #19897, #718, #29526, #21828, #22282, #29697, #10228, #27171, #5483, #27002, #116, #7556 ),
 ( #17216, #5165, #10080, #15135, #12750, #8017, #14814, #14970, #10378, #12437, #17682, #7697, #27325, #9771, #19436, #29082, #7390, #17068 ),
 ( #26724, #17355, #5308, #422, #5014, #24638, #14675, #24335, #12284, #21971, #260, #9924, #30466, #3880, #27943, #5964, #13530, #15904 ) ),
 .UNSPECIFIED., .F., .F., .F. ) 
 B_SPLINE_SURFACE_WITH_KNOTS ( ( 3, 2, 3 ),
 ( 4, 2, 2, 2, 2, 2, 2, 2, 4 ),
 ( -0.01000000000000000021, 0.000000000000000000, 1.000000000000000000 ),
 ( 1.413716694115406902, 1.826050729899067360, 2.238384765682727817, 2.650718801466387831, 3.063052837250048288, 3.475386873033708746, 3.887720908817368759, 4.300054944601029661, 4.712388980384689674 ),
 .UNSPECIFIED. ) 
 GEOMETRIC_REPRESENTATION_ITEM ( )  RATIONAL_B_SPLINE_SURFACE ( (
 ( 1.000000000000000000, 1.000000000000000000, 1.000000000000000000, 1.000000000000000000, 1.000000000000000000, 1.000000000000000000, 1.000000000000000000, 1.000000000000000000, 1.000000000000000000, 1.000000000000000000, 1.000000000000000000, 1.000000000000000000, 1.000000000000000000, 1.000000000000000000, 1.000000000000000000, 1.000000000000000000, 1.000000000000000000, 1.000000000000000000),
 ( 1.000000000000000000, 1.000000000000000000, 1.000000000000000000, 1.000000000000000000, 1.000000000000000000, 1.000000000000000000, 1.000000000000000000, 1.000000000000000000, 1.000000000000000000, 1.000000000000000000, 1.000000000000000000, 1.000000000000000000, 1.000000000000000000, 1.000000000000000000, 1.000000000000000000, 1.000000000000000000, 1.000000000000000000, 1.000000000000000000),
 ( 1.000000000000000000, 1.000000000000000000, 1.000000000000000000, 1.000000000000000000, 1.000000000000000000, 1.000000000000000000, 1.000000000000000000, 1.000000000000000000, 1.000000000000000000, 1.000000000000000000, 1.000000000000000000, 1.000000000000000000, 1.000000000000000000, 1.000000000000000000, 1.000000000000000000, 1.000000000000000000, 1.000000000000000000, 1.000000000000000000),
 ( 0.7071067811865476838, 0.7071067811865476838, 0.7071067811865475727, 0.7071067811865475727, 0.7071067811865476838, 0.7071067811865476838, 0.7071067811865475727, 0.7071067811865475727, 0.7071067811865473507, 0.7071067811865473507, 0.7071067811865479058, 0.7071067811865479058, 0.7071067811865475727, 0.7071067811865475727, 0.7071067811865463515, 0.7071067811865463515, 0.7071067811865475727, 0.7071067811865475727),
 ( 1.000000000000000000, 1.000000000000000000, 1.000000000000000000, 1.000000000000000000, 1.000000000000000000, 1.000000000000000000, 1.000000000000000000, 1.000000000000000000, 1.000000000000000000, 1.000000000000000000, 1.000000000000000000, 1.000000000000000000, 1.000000000000000000, 1.000000000000000000, 1.000000000000000000, 1.000000000000000000, 1.000000000000000000, 1.000000000000000000) ) ) 
 REPRESENTATION_ITEM ( '' )  SURFACE ( )  );
#7593 = CARTESIAN_POINT ( 'NONE',  ( 15.41080140630215922, -3.722599991951294207, 3.938370952810156478 ) ) ;
#7594 = B_SPLINE_CURVE_WITH_KNOTS ( 'NONE', 3,
 ( #21550, #15138, #19330, #14085, #30875, #28966, #4589, #11569, #9344, #19899, #4, #12600 ),
 .UNSPECIFIED., .F., .F.,
 ( 4, 2, 2, 2, 2, 4 ),
 ( 0.000000000000000000, 5.522938194211708289E-05, 0.0001104587638842341658, 0.0002209175277684793091, 0.0004418350555369705986, 0.0008836701110739516056 ),
 .UNSPECIFIED. ) ;
#7595 = CARTESIAN_POINT ( 'NONE',  ( 22.00209989016466494, 7.765045920621504116, -1.950000000000076561 ) ) ;
#7596 = DIRECTION ( 'NONE',  ( -7.790947421114572685E-15, 0.7438053426816656488, -0.6683962987616028917 ) ) ;
#7597 = ADVANCED_FACE ( 'NONE', ( #218 ), #4591, .F. ) ;
#7598 = CARTESIAN_POINT ( 'NONE',  ( -59.43190135328987367, 3.335228286247303053, -1.083751783614652409 ) ) ;
#7600 = VECTOR ( 'NONE', #7549, 999.9999999999998863 ) ;
#7599 = CARTESIAN_POINT ( 'NONE',  ( -44.59999999999998010, 8.366749974758271452E-15, -1.593320673368357319E-13 ) ) ;
#7602 = CARTESIAN_POINT ( 'NONE',  ( 25.48092967892656446, 5.262749364038179500, 1.424999999999912337 ) ) ;
#7601 = CARTESIAN_POINT ( 'NONE',  ( 58.73309930451056005, 0.5681566835776329372, 1.786899855580384555 ) ) ;
#7603 = ORIENTED_EDGE ( 'NONE', *, *, #4082, .F. ) ;
#7604 = CARTESIAN_POINT ( 'NONE',  ( 58.65844932252318245, -1.819473848873478516, 0.4532319986951370838 ) ) ;
#7605 = ORIENTED_EDGE ( 'NONE', *, *, #16812, .T. ) ;
#7606 = UNCERTAINTY_MEASURE_WITH_UNIT (LENGTH_MEASURE( 1.000000000000000082E-05 ), #4410, 'distance_accuracy_value', 'NONE');
#7607 = FACE_OUTER_BOUND ( 'NONE', #23453, .T. ) ;
#7609 = DIRECTION ( 'NONE',  ( 0.000000000000000000, -2.168404344971008868E-16, -1.000000000000000000 ) ) ;
#7608 = CARTESIAN_POINT ( 'NONE',  ( 57.01173390802158991, 0.7326096616897963543, -2.432492958759772783 ) ) ;
#7610 = CARTESIAN_POINT ( 'NONE',  ( 47.05963571244990362, 8.266527678078146479, -1.550000000000163469 ) ) ;
#7611 = VERTEX_POINT ( 'NONE', #21070 ) ;
#7612 = EDGE_LOOP ( 'NONE', ( #3665, #27999, #18323, #19364 ) ) ;
#7613 = DIRECTION ( 'NONE',  ( 0.000000000000000000, -1.000000000000000000, -3.491481338843133355E-15 ) ) ;
#7614 = DIRECTION ( 'NONE',  ( 0.000000000000000000, 0.000000000000000000, -1.000000000000000000 ) ) ;
#7615 = VERTEX_POINT ( 'NONE', #3953 ) ;
#7616 = DIRECTION ( 'NONE',  ( 1.000000000000000000, 0.000000000000000000, -1.047444401652940007E-14 ) ) ;
#7617 = CARTESIAN_POINT ( 'NONE',  ( 50.40000000000003411, 0.7618928438397208902, 3.939512004971702730 ) ) ;
#7618 = CARTESIAN_POINT ( 'NONE',  ( 47.09453520915242564, 9.265918505097243241, -1.950000000000163380 ) ) ;
#7619 = EDGE_LOOP ( 'NONE', ( #31215, #13313, #15842, #28334 ) ) ;
#7620 = EDGE_CURVE ( 'NONE', #23640, #28800, #20181, .T. ) ;
#7621 = CARTESIAN_POINT ( 'NONE',  ( -59.29999999999996163, -3.145551863026063266, -1.948307423342382938 ) ) ;
#7622 = ORIENTED_EDGE ( 'NONE', *, *, #11765, .F. ) ;
#7623 = TOROIDAL_SURFACE ( 'NONE', #25809, 0.2000000000000000111, 0.1000000000000000056 ) ;
#7624 = CARTESIAN_POINT ( 'NONE',  ( -57.82202994616206126, 2.078460969082646770, 3.599999999999802025 ) ) ;
#7625 = DIRECTION ( 'NONE',  ( -1.000000000000000000, -3.053848253006669023E-16, 2.042510438544995415E-16 ) ) ;
#7626 = CARTESIAN_POINT ( 'NONE',  ( 48.37884656342667711, -0.9200365198983474491, -3.998286360709680576 ) ) ;
#7627 = CARTESIAN_POINT ( 'NONE',  ( -54.44999999999997442, -1.500000000000000000, 3.300094695611020867 ) ) ;
#7628 = CARTESIAN_POINT ( 'NONE',  ( 54.40000000000001990, -1.084202172485504434E-16, 4.374999999999999112 ) ) ;
#7629 = CARTESIAN_POINT ( 'NONE',  ( -56.70655989232412253, -3.399999999999991029, -2.112596694108398482E-13 ) ) ;
#7630 = ADVANCED_FACE ( 'NONE', ( #8839 ), #8629, .T. ) ;
#7632 = CARTESIAN_POINT ( 'NONE',  ( -61.37141394935931515, -2.563724941572514737, -0.8190313348002082883 ) ) ;
#7631 = CARTESIAN_POINT ( 'NONE',  ( 50.56951033778286586, -0.1019484954143860672, -1.190698274346102092 ) ) ;
#7633 = CARTESIAN_POINT ( 'NONE',  ( 50.25000000000000000, 1.666164585742626159, 1.106298139391201030 ) ) ;
#7634 = CARTESIAN_POINT ( 'NONE',  ( 48.43359507746255588, 1.250162886418204389, -3.874884102585954171 ) ) ;
#7636 = CARTESIAN_POINT ( 'NONE',  ( -62.09999999999997300, -2.673664601801277296, -0.2941788001767337013 ) ) ;
#7635 = CARTESIAN_POINT ( 'NONE',  ( -69.19999999999998863, -6.931756715175872842E-16, 2.447411951356162049E-15 ) ) ;
#7637 = VERTEX_POINT ( 'NONE', #28339 ) ;
#7638 = DIRECTION ( 'NONE',  ( 0.000000000000000000, 0.9996898646859339044, 0.02490330187382721813 ) ) ;
#7639 = CARTESIAN_POINT ( 'NONE',  ( -36.79682133506354091, -5.289443499204832477, -1.131445731060801707 ) ) ;
#7641 = CARTESIAN_POINT ( 'NONE',  ( 54.19386703870443966, 5.671865141453449333, 1.949999999999810329 ) ) ;
#7640 = CARTESIAN_POINT ( 'NONE',  ( 51.39880218607839168, -0.9985439640369458969, -1.587650844584835852 ) ) ;
#7642 = DIRECTION ( 'NONE',  ( -1.000000000000000000, 0.000000000000000000, 1.047444401652940007E-14 ) ) ;
#7643 = EDGE_LOOP ( 'NONE', ( #23859, #11767, #3359, #13508 ) ) ;
#7644 = CARTESIAN_POINT ( 'NONE',  ( 51.80000000000001847, 2.428612866367529932E-14, -1.808587333520743709E-13 ) ) ;
#7645 = VERTEX_POINT ( 'NONE', #6491 ) ;
#7646 = CARTESIAN_POINT ( 'NONE',  ( -37.18272003341174070, -1.653865106024005477E-14, 0.000000000000000000 ) ) ;
#7647 = VERTEX_POINT ( 'NONE', #20336 ) ;
#7648 = ORIENTED_EDGE ( 'NONE', *, *, #3216, .T. ) ;
#7649 = CARTESIAN_POINT ( 'NONE',  ( 67.99999999999997158, 4.990435706524438473E-16, -4.050000000000713030 ) ) ;
#7650 = ORIENTED_EDGE ( 'NONE', *, *, #11832, .T. ) ;
#7651 = CARTESIAN_POINT ( 'NONE',  ( 48.43359507746254877, -1.250162886418155761, 3.874884102585953727 ) ) ;
#7652 = ADVANCED_FACE ( 'NONE', ( #26114 ), #10659, .F. ) ;
#7653 = CARTESIAN_POINT ( 'NONE',  ( -54.58155989232414385, -1.962990915244731571, 3.399999999999797851 ) ) ;
#7654 = ORIENTED_EDGE ( 'NONE', *, *, #27488, .T. ) ;
#7655 = CYLINDRICAL_SURFACE ( 'NONE', #16122, 0.7500000000000002220 ) ;
#7656 = CYLINDRICAL_SURFACE ( 'NONE', #25313, 1.000000000000000000 ) ;
#7657 = ADVANCED_FACE ( 'NONE', ( #15572, #21238 ), #5746, .F. ) ;
#7658 = CARTESIAN_POINT ( 'NONE',  ( -61.39999999999998437, -2.565822298769830478, -0.8405688140393350327 ) ) ;
#7659 = ORIENTED_EDGE ( 'NONE', *, *, #15805, .F. ) ;
#7660 = VECTOR ( 'NONE', #17371, 1000.000000000000000 ) ;
#7661 = TOROIDAL_SURFACE ( 'NONE', #30401, 2.973495046502706796, 1.679509022399086948 ) ;
#7662 = FACE_OUTER_BOUND ( 'NONE', #31089, .T. ) ;
#7663 = DIRECTION ( 'NONE',  ( 0.000000000000000000, 0.000000000000000000, 1.000000000000000000 ) ) ;
#7664 = CARTESIAN_POINT ( 'NONE',  ( 52.06628335902944826, 0.5434431642986584654, 1.794517909405660250 ) ) ;
#7665 = CARTESIAN_POINT ( 'NONE',  ( 57.00875904852982501, -0.7282698412063691729, 2.435189460583063514 ) ) ;
#7666 = EDGE_CURVE ( 'NONE', #15285, #21568, #19684, .T. ) ;
#7668 = CARTESIAN_POINT ( 'NONE',  ( 58.75000000000003553, -1.022750809560422525, 1.571497941946552901 ) ) ;
#7667 = CARTESIAN_POINT ( 'NONE',  ( -36.92362342067078629, -3.046685255238732459, 4.470266847515959263 ) ) ;
#7669 = DIRECTION ( 'NONE',  ( 1.189524669241239263E-14, 0.000000000000000000, 1.000000000000000000 ) ) ;
#7670 = DIRECTION ( 'NONE',  ( -1.000000000000000000, -3.054027077731387480E-16, 2.042479963029832083E-16 ) ) ;
#7671 = VECTOR ( 'NONE', #12713, 1000.000000000000000 ) ;
#7672 = CARTESIAN_POINT ( 'NONE',  ( -56.67499999999996874, 0.9643027244899941008, -4.702139965541347166 ) ) ;
#7673 = VERTEX_POINT ( 'NONE', #29965 ) ;
#7674 = EDGE_CURVE ( 'NONE', #26805, #7259, #27327, .T. ) ;
#7675 = EDGE_LOOP ( 'NONE', ( #13633, #2807, #15571, #31226 ) ) ;
#7676 = CIRCLE ( 'NONE', #18312, 0.05000000000000017625 ) ;
#7677 = ORIENTED_EDGE ( 'NONE', *, *, #3780, .T. ) ;
#7678 = CARTESIAN_POINT ( 'NONE',  ( -59.18789508915042319, 2.395752775956333291, 1.250136525132548915 ) ) ;
#7679 = CARTESIAN_POINT ( 'NONE',  ( -60.11042740578358945, -0.7887156198831607457, 3.845940847736174728 ) ) ;
#7681 = CYLINDRICAL_SURFACE ( 'NONE', #5062, 0.1500000000000000777 ) ;
#7680 = DIRECTION ( 'NONE',  ( 1.000000000000000000, 1.047444401652940007E-14, 0.000000000000000000 ) ) ;
#7682 = ORIENTED_EDGE ( 'NONE', *, *, #20337, .T. ) ;
#7683 = VERTEX_POINT ( 'NONE', #16149 ) ;
#7684 = CARTESIAN_POINT ( 'NONE',  ( 50.93175545242106494, -4.417905783403957898, -1.285520530455074528 ) ) ;
#7685 = VERTEX_POINT ( 'NONE', #4256 ) ;
#7686 = CARTESIAN_POINT ( 'NONE',  ( 49.05000000000002558, 1.401298464324817071E-42, -5.137714790107672405E-13 ) ) ;
#7687 = EDGE_CURVE ( 'NONE', #7227, #11190, #9187, .T. ) ;
#7688 = ORIENTED_EDGE ( 'NONE', *, *, #23564, .T. ) ;
#7689 = CARTESIAN_POINT ( 'NONE',  ( 32.30803788188134718, 7.816246126569818209, -1.950000000000048361 ) ) ;
#7690 = EDGE_CURVE ( 'NONE', #7270, #8110, #39, .T. ) ;
#7691 = EDGE_LOOP ( 'NONE', ( #4869, #17930 ) ) ;
#7692 = DIRECTION ( 'NONE',  ( 1.000000000000000000, -0.000000000000000000, -0.000000000000000000 ) ) ;
#7693 = EDGE_CURVE ( 'NONE', #23272, #25117, #30879, .T. ) ;
#7694 = CARTESIAN_POINT ( 'NONE',  ( 57.02474788916244108, 0.7434350531339385393, 1.784201504348416067 ) ) ;
#7695 = CARTESIAN_POINT ( 'NONE',  ( 15.30042582489636160, -5.377732434016963659, -0.5657657146875257892 ) ) ;
#7696 = CARTESIAN_POINT ( 'NONE',  ( -54.89405989232412963, 2.944486372867106461, -1.700000000000182254 ) ) ;
#7697 = CARTESIAN_POINT ( 'NONE',  ( 53.74478519188836856, 7.379842749953419379, -2.050000000000249401 ) ) ;
#7698 = DIRECTION ( 'NONE',  ( -0.000000000000000000, 0.9875000000000001554, 0.1576190026614806561 ) ) ;
#7699 = CARTESIAN_POINT ( 'NONE',  ( 50.46953806735880477, 1.143620537822834349, -3.937943076466140724 ) ) ;
#7700 = DIRECTION ( 'NONE',  ( 1.000000000000000000, -1.219044193948983948E-29, 3.491481338843133355E-15 ) ) ;
#7701 = DIRECTION ( 'NONE',  ( -1.000000000000000000, 0.000000000000000000, 1.047444401652940007E-14 ) ) ;
#7702 = CIRCLE ( 'NONE', #16310, 0.05000000000000012768 ) ;
#7703 = ORIENTED_EDGE ( 'NONE', *, *, #25651, .F. ) ;
#7704 = ADVANCED_FACE ( 'NONE', ( #25799 ), #841, .F. ) ;
#7705 = CARTESIAN_POINT ( 'NONE',  ( -62.14999999999998437, 1.152747360993128871E-15, 2.207939306294521009E-15 ) ) ;
#7706 = CARTESIAN_POINT ( 'NONE',  ( 57.05000000000001847, 0.7500000000000000000, 1.745709025009609228 ) ) ;
#7707 = DIRECTION ( 'NONE',  ( 1.000000000000000000, 1.047444401652940007E-14, 0.000000000000000000 ) ) ;
#7708 = ORIENTED_EDGE ( 'NONE', *, *, #16245, .F. ) ;
#7709 = CARTESIAN_POINT ( 'NONE',  ( 50.36673905152862574, 1.398826622412688403, -3.854114288381606190 ) ) ;
#7710 = ORIENTED_EDGE ( 'NONE', *, *, #30988, .T. ) ;
#7711 = ADVANCED_FACE ( 'NONE', ( #6645 ), #22710, .T. ) ;
#7712 = CARTESIAN_POINT ( 'NONE',  ( -35.98994760229852830, -5.086913989684993531, 1.171642050077752462 ) ) ;
#7713 = B_SPLINE_CURVE_WITH_KNOTS ( 'NONE', 3,
 ( #13321, #1465, #23473, #30117, #15730, #10973 ),
 .UNSPECIFIED., .F., .F.,
 ( 4, 2, 4 ),
 ( 0.000000000000000000, 0.001045838473297321580, 0.002091676946594643160 ),
 .UNSPECIFIED. ) ;
#7715 = DIRECTION ( 'NONE',  ( 0.000000000000000000, 0.2008964009354147484, -0.9796124928211139560 ) ) ;
#7714 = CARTESIAN_POINT ( 'NONE',  ( 58.75000000000002842, -0.8897917884444737080, 1.791164585743103999 ) ) ;
#7716 = ORIENTED_EDGE ( 'NONE', *, *, #18779, .T. ) ;
#7717 = CARTESIAN_POINT ( 'NONE',  ( 61.02723049001807709, -0.5636288612503438378, -1.705074539937696976 ) ) ;
#7718 = FACE_OUTER_BOUND ( 'NONE', #31084, .T. ) ;
#7720 = FACE_OUTER_BOUND ( 'NONE', #287, .T. ) ;
#7719 = CARTESIAN_POINT ( 'NONE',  ( 52.41501436764352206, 3.996684283499680745, 2.045735246708100696 ) ) ;
#7721 = DIRECTION ( 'NONE',  ( 0.000000000000000000, 1.532429380227445212E-15, -1.000000000000000000 ) ) ;
#7722 = CARTESIAN_POINT ( 'NONE',  ( -57.99999999999997158, -2.489203624310585727, 2.804704140674917134 ) ) ;
#7723 = CARTESIAN_POINT ( 'NONE',  ( -55.93749999999995737, 1.962990915244752888, -3.400000000000188205 ) ) ;
#7724 = EDGE_CURVE ( 'NONE', #9570, #26216, #24308, .T. ) ;
#7725 = DIRECTION ( 'NONE',  ( 0.000000000000000000, -1.000000000000000000, 0.000000000000000000 ) ) ;
#7726 = CARTESIAN_POINT ( 'NONE',  ( -54.39999999999999147, 1.499999999999998002, 3.363870538531247067 ) ) ;
#7727 =( BOUNDED_CURVE ( )  B_SPLINE_CURVE ( 2, ( #21390, #14233, #11861, #29564, #27208 ),
 .UNSPECIFIED., .F., .T. ) 
 B_SPLINE_CURVE_WITH_KNOTS ( ( 3, 2, 3 ),
 ( 0.6944444444444445308, 0.7037037037037037202, 0.7112308204265433975 ),
 .UNSPECIFIED. ) 
 CURVE ( )  GEOMETRIC_REPRESENTATION_ITEM ( )  RATIONAL_B_SPLINE_CURVE ( ( 0.9330127018922194093, 0.9330127018922197424, 1.000000000000000000, 0.9455441091250682550, 0.9353569697112142922 ) ) 
 REPRESENTATION_ITEM ( '' )  );
#7729 = DIRECTION ( 'NONE',  ( -1.000000000000000000, -2.586136946169074517E-16, 0.000000000000000000 ) ) ;
#7728 = CIRCLE ( 'NONE', #26449, 1.875000000000000222 ) ;
#7730 = CARTESIAN_POINT ( 'NONE',  ( 51.70000000000003126, -3.550773357292059007, 2.049880134335640758 ) ) ;
#7731 = VERTEX_POINT ( 'NONE', #17797 ) ;
#7732 = CARTESIAN_POINT ( 'NONE',  ( 15.03925126672127810, -3.426725943139564912, 3.937891353488730317 ) ) ;
#7733 = CARTESIAN_POINT ( 'NONE',  ( -62.06720320256510348, -2.648373711098206851, 0.1969833506954761504 ) ) ;
#7734 = DIRECTION ( 'NONE',  ( 0.8023336663629262455, -0.5470456816110725873, 0.2387503090077610912 ) ) ;
#7735 = EDGE_CURVE ( 'NONE', #4844, #8781, #11677, .T. ) ;
#7736 = CARTESIAN_POINT ( 'NONE',  ( 61.23787131559264907, -0.8905369330980658082, 1.779178344870881556 ) ) ;
#7738 = CARTESIAN_POINT ( 'NONE',  ( 50.40000000000001990, -0.7618928438396727065, -3.939512004971702730 ) ) ;
#7737 = CARTESIAN_POINT ( 'NONE',  ( 61.25000000000002132, 6.415596960124259844E-13, 3.111507638930570854E-58 ) ) ;
#7739 = ADVANCED_FACE ( 'NONE', ( #14077 ), #19006, .F. ) ;
#7740 = ORIENTED_EDGE ( 'NONE', *, *, #7850, .T. ) ;
#7741 = ORIENTED_EDGE ( 'NONE', *, *, #28819, .T. ) ;
#7742 = EDGE_CURVE ( 'NONE', #3419, #20255, #9673, .T. ) ;
#7743 = DIRECTION ( 'NONE',  ( 0.000000000000000000, 0.5333333333333335480, 0.8459051693633012903 ) ) ;
#7744 = AXIS2_PLACEMENT_3D ( 'NONE', #4565, #21520, #26411 ) ;
#7746 = CARTESIAN_POINT ( 'NONE',  ( 65.00000000000001421, -1.025519176787267142E-28, -6.808388610744108654E-13 ) ) ;
#7745 = CARTESIAN_POINT ( 'NONE',  ( 15.56401610563845672, -3.953723660658770900, -3.694477770903854541 ) ) ;
#7747 = LINE ( 'NONE', #14868, #29719 ) ;
#7748 = AXIS2_PLACEMENT_3D ( 'NONE', #13923, #23302, #4126 ) ;
#7749 = EDGE_LOOP ( 'NONE', ( #22078, #7192, #3484, #18607, #31156 ) ) ;
#7750 = ORIENTED_EDGE ( 'NONE', *, *, #24316, .T. ) ;
#7751 = DIRECTION ( 'NONE',  ( 0.000000000000000000, 0.000000000000000000, 1.000000000000000000 ) ) ;
#7752 = CARTESIAN_POINT ( 'NONE',  ( 51.89360908398765559, 0.6611756245550114430, 1.497563819581031241 ) ) ;
#7753 = ORIENTED_EDGE ( 'NONE', *, *, #29471, .T. ) ;
#7754 = DIRECTION ( 'NONE',  ( -1.000000000000000000, -1.047444401652940007E-14, 0.000000000000000000 ) ) ;
#7755 = LINE ( 'NONE', #17421, #1239 ) ;
#7756 = CARTESIAN_POINT ( 'NONE',  ( -59.60065375968532209, -2.157866302380323731, 1.538217518236592474 ) ) ;
#7757 = ORIENTED_EDGE ( 'NONE', *, *, #30680, .F. ) ;
#7758 = CARTESIAN_POINT ( 'NONE',  ( 0.000000000000000000, 0.000000000000000000, 0.000000000000000000 ) ) ;
#7759 = ADVANCED_FACE ( 'NONE', ( #6 ), #17237, .T. ) ;
#7760 = CARTESIAN_POINT ( 'NONE',  ( 50.30000000000001847, -4.899999999999999467, -3.950000000000022826 ) ) ;
#7761 =( BOUNDED_CURVE ( )  B_SPLINE_CURVE ( 2, ( #5242, #23843, #10016, #27084, #24717, #14748, #26210, #28582, #23695 ),
 .UNSPECIFIED., .F., .T. ) 
 B_SPLINE_CURVE_WITH_KNOTS ( ( 3, 2, 2, 2, 3 ),
 ( 0.6388888888888889506, 0.6481481481481481399, 0.6666666666666666297, 0.6851851851851852304, 0.6944444444444445308 ),
 .UNSPECIFIED. ) 
 CURVE ( )  GEOMETRIC_REPRESENTATION_ITEM ( )  RATIONAL_B_SPLINE_CURVE ( ( 0.9330127018922194093, 0.9330127018922197424, 1.000000000000000000, 0.8660254037844387076, 1.000000000000000000, 0.8660254037844387076, 1.000000000000000000, 0.9330127018922189652, 0.9330127018922194093 ) ) 
 REPRESENTATION_ITEM ( '' )  );
#7762 = ORIENTED_EDGE ( 'NONE', *, *, #4741, .T. ) ;
#7763 = CARTESIAN_POINT ( 'NONE',  ( -59.82202994616204705, -4.156921938165296204, -2.272478542645976661E-13 ) ) ;
#7764 = CARTESIAN_POINT ( 'NONE',  ( 54.16553928697275921, 6.951169537962178069, -2.050000000000189448 ) ) ;
#7765 = DIRECTION ( 'NONE',  ( 0.000000000000000000, -0.9996898646859344595, -0.02490330187381124133 ) ) ;
#7766 = CIRCLE ( 'NONE', #13805, 4.000000000000000000 ) ;
#7767 = B_SPLINE_CURVE_WITH_KNOTS ( 'NONE', 3,
 ( #22316, #24971, #10263, #27034, #3297, #5345, #12943, #15010 ),
 .UNSPECIFIED., .F., .F.,
 ( 4, 2, 2, 4 ),
 ( 1.494941423529140449E-17, 0.001707980657444188501, 0.002561970986166275163, 0.003415961314888361824 ),
 .UNSPECIFIED. ) ;
#7768 = FACE_OUTER_BOUND ( 'NONE', #26461, .T. ) ;
#7769 = CARTESIAN_POINT ( 'NONE',  ( 51.70000000000001705, -4.259946800035232073, -1.000000000000000222 ) ) ;
#7770 = DIRECTION ( 'NONE',  ( 0.000000000000000000, 0.000000000000000000, -1.000000000000000000 ) ) ;
#7772 = CARTESIAN_POINT ( 'NONE',  ( -36.76447480099743359, -0.6031025731806715084, -5.374022845360705958 ) ) ;
#7771 = CARTESIAN_POINT ( 'NONE',  ( 61.23770293222991512, 0.8897917884447287262, -1.791164585742097914 ) ) ;
#7773 = PRODUCT ( 'Pocket Clip', 'Pocket Clip', '', ( #18228 ) ) ;
#7774 = CARTESIAN_POINT ( 'NONE',  ( -62.09772439161942259, -2.519395624556878488, 0.1682286568119469583 ) ) ;
#7775 = LINE ( 'NONE', #5102, #31181 ) ;
#7777 = DIRECTION ( 'NONE',  ( 3.491481338843133355E-15, 0.000000000000000000, 1.000000000000000000 ) ) ;
#7776 = CARTESIAN_POINT ( 'NONE',  ( 16.10624235918716352, 5.192953935288670664, -1.516181439821520538 ) ) ;
#7778 = EDGE_CURVE ( 'NONE', #22413, #9758, #26579, .T. ) ;
#7779 = ORIENTED_EDGE ( 'NONE', *, *, #21581, .T. ) ;
#7780 = CARTESIAN_POINT ( 'NONE',  ( 50.41431699104521158, -1.130504494894903900, -3.941663789486498093 ) ) ;
#7781 = CARTESIAN_POINT ( 'NONE',  ( 47.73554962785864575, -4.311893144378706744, -1.282556980650735978 ) ) ;
#7782 = CARTESIAN_POINT ( 'NONE',  ( 48.00000000000003553, -4.417905791132258564, 1.285520503972574557 ) ) ;
#7783 = ORIENTED_EDGE ( 'NONE', *, *, #28785, .T. ) ;
#7784 = CARTESIAN_POINT ( 'NONE',  ( -61.39793805872155730, -2.653040316467372151, 0.5011856904451539307 ) ) ;
#7785 = ORIENTED_EDGE ( 'NONE', *, *, #5984, .F. ) ;
#7786 = VECTOR ( 'NONE', #21851, 1000.000000000000000 ) ;
#7787 = DIRECTION ( 'NONE',  ( 1.000000000000000000, 1.047444401652940007E-14, 0.000000000000000000 ) ) ;
#7788 = ORIENTED_EDGE ( 'NONE', *, *, #12789, .F. ) ;
#7789 = ORIENTED_EDGE ( 'NONE', *, *, #2651, .F. ) ;
#7790 = CARTESIAN_POINT ( 'NONE',  ( 15.18459684427939749, 4.683225679163376398, -2.703237727951164793 ) ) ;
#7791 = EDGE_LOOP ( 'NONE', ( #15775, #12960, #15240, #6246 ) ) ;
#7792 =( NAMED_UNIT ( * ) SI_UNIT ( $, .STERADIAN. ) SOLID_ANGLE_UNIT ( ) );
#7793 = CARTESIAN_POINT ( 'NONE',  ( 32.53491908475320571, 7.895085025454613437, 1.949999999999886713 ) ) ;
#7794 = EDGE_CURVE ( 'NONE', #4056, #17666, #22002, .T. ) ;
#7795 = CARTESIAN_POINT ( 'NONE',  ( -61.00952994616203284, 3.117691453623994580, -1.800000000000202993 ) ) ;
#7796 = ORIENTED_EDGE ( 'NONE', *, *, #27040, .F. ) ;
#7797 = CARTESIAN_POINT ( 'NONE',  ( -56.24999999999997868, -2.944486372867090918, 1.699999999999786349 ) ) ;
#7798 = ORIENTED_EDGE ( 'NONE', *, *, #3847, .F. ) ;
#7799 = CIRCLE ( 'NONE', #20455, 0.1500000000000003830 ) ;
#7800 = CARTESIAN_POINT ( 'NONE',  ( 51.70000000000002416, 2.428612866367529932E-14, -1.805095852181900386E-13 ) ) ;
#7801 = CARTESIAN_POINT ( 'NONE',  ( 26.61920844897847260, 5.219578739559102232, 2.049999999999775113 ) ) ;
#7802 = VERTEX_POINT ( 'NONE', #9339 ) ;
#7803 = CARTESIAN_POINT ( 'NONE',  ( -59.22282295291818599, -3.176879556488940270, 1.263313363143568013 ) ) ;
#7804 = CARTESIAN_POINT ( 'NONE',  ( -59.09999999999997300, 2.750000000000007994, -2.003569730682425015E-13 ) ) ;
#7805 = DIRECTION ( 'NONE',  ( 1.000000000000000000, 3.054025858079668409E-16, -2.042474015755241579E-16 ) ) ;
#7806 = LINE ( 'NONE', #17184, #19526 ) ;
#7807 = CIRCLE ( 'NONE', #6818, 2.750000000000000000 ) ;
#7808 = CARTESIAN_POINT ( 'NONE',  ( 57.00797408584070070, 0.7277374606022131154, 2.435538690626270597 ) ) ;
#7810 = CARTESIAN_POINT ( 'NONE',  ( -59.60604010435355349, 3.187076279294280390, -1.184290838417780600 ) ) ;
#7809 = CARTESIAN_POINT ( 'NONE',  ( -36.11187263677871329, -3.378578820314678488, 3.972872285093159483 ) ) ;
#7811 = AXIS2_PLACEMENT_3D ( 'NONE', #442, #27024, #18803 ) ;
#7812 = CARTESIAN_POINT ( 'NONE',  ( -54.39999999999999147, 1.599999999999998090, 3.363870538531247512 ) ) ;
#7813 = CARTESIAN_POINT ( 'NONE',  ( 52.20711756518983293, 0.5000000000005468959, -1.807104036850122109 ) ) ;
#7814 = ADVANCED_FACE ( 'NONE', ( #21541 ), #24368, .F. ) ;
#7815 = CARTESIAN_POINT ( 'NONE',  ( -54.49999999999997868, 1.549999999999999600, -3.332135201338624952 ) ) ;
#7816 = CARTESIAN_POINT ( 'NONE',  ( 51.68129744679068693, 4.333300462216209681, 2.050000000000262279 ) ) ;
#7817 = CIRCLE ( 'NONE', #9868, 4.100000000000022737 ) ;
#7818 = VERTEX_POINT ( 'NONE', #31017 ) ;
#7819 = ORIENTED_EDGE ( 'NONE', *, *, #10733, .F. ) ;
#7820 = EDGE_LOOP ( 'NONE', ( #26464, #482, #28128, #29593, #16891 ) ) ;
#7821 = CARTESIAN_POINT ( 'NONE',  ( -62.09529625801577168, -2.507189385900795653, -0.2994239205180544983 ) ) ;
#7822 = CARTESIAN_POINT ( 'NONE',  ( -60.73542740578358945, -3.725040285533365747, 1.239922660687676093 ) ) ;
#7824 = CARTESIAN_POINT ( 'NONE',  ( -61.37035765953427102, -2.600782770733796934, 0.6894593850982138061 ) ) ;
#7823 = FACE_BOUND ( 'NONE', #27826, .T. ) ;
#7825 = VERTEX_POINT ( 'NONE', #23905 ) ;
#7826 = ORIENTED_EDGE ( 'NONE', *, *, #851, .T. ) ;
#7827 = AXIS2_PLACEMENT_3D ( 'NONE', #25890, #26367, #16874 ) ;
#7828 = CARTESIAN_POINT ( 'NONE',  ( 51.03681636671011290, -4.380055612571975843, -1.406160842577909964 ) ) ;
#7829 = VERTEX_POINT ( 'NONE', #28657 ) ;
#7830 = DIRECTION ( 'NONE',  ( 0.000000000000000000, 0.9996898646859344595, 0.02490330187381124133 ) ) ;
#7831 = EDGE_CURVE ( 'NONE', #24006, #15457, #14696, .T. ) ;
#7832 = ORIENTED_EDGE ( 'NONE', *, *, #28716, .F. ) ;
#7833 = CARTESIAN_POINT ( 'NONE',  ( 31.73163254175006287, 7.673342708999780548, -2.050000000000110401 ) ) ;
#7834 = ORIENTED_EDGE ( 'NONE', *, *, #228, .F. ) ;
#7835 = CARTESIAN_POINT ( 'NONE',  ( -58.37499999999997158, 2.489203624310597274, -2.804704140674911361 ) ) ;
#7836 = CARTESIAN_POINT ( 'NONE',  ( 50.80000000000001847, -4.003661535119149129, -1.269131321892095654 ) ) ;
#7837 = CARTESIAN_POINT ( 'NONE',  ( 15.94709373951294573, -4.924630501335173882, -2.234249019593651742 ) ) ;
#7838 = CIRCLE ( 'NONE', #26560, 0.2500000000000002776 ) ;
#7839 = CARTESIAN_POINT ( 'NONE',  ( -59.89405989232412963, -3.920666489018293080E-15, 3.399999999999786304 ) ) ;
#7840 = EDGE_CURVE ( 'NONE', #7345, #10060, #429, .T. ) ;
#7841 = CARTESIAN_POINT ( 'NONE',  ( 52.18331218360314949, 8.688678219032366812, -2.050000000000181455 ) ) ;
#7842 = CARTESIAN_POINT ( 'NONE',  ( 58.65000000000000568, 1.827356000910769440, 0.4213753797520914390 ) ) ;
#7843 = CARTESIAN_POINT ( 'NONE',  ( 50.22478246037407246, 8.164214000976986796, 2.049999999999824851 ) ) ;
#7844 = DIRECTION ( 'NONE',  ( 1.000000000000000000, 1.047444401652940007E-14, 0.000000000000000000 ) ) ;
#7845 = DIRECTION ( 'NONE',  ( 1.000000000000000000, 0.000000000000000000, -3.491481338843133355E-15 ) ) ;
#7846 = TOROIDAL_SURFACE ( 'NONE', #11403, 4.600000000000000533, 0.5000000000000013323 ) ;
#7847 = CARTESIAN_POINT ( 'NONE',  ( -59.69457535546589355, 2.411387898321005530, -1.235406689480260001 ) ) ;
#7848 = ADVANCED_FACE ( 'NONE', ( #23757 ), #6972, .T. ) ;
#7849 = DIRECTION ( 'NONE',  ( 0.000000000000000000, -1.224646799147353207E-16, 1.000000000000000000 ) ) ;
#7850 = EDGE_CURVE ( 'NONE', #5429, #25588, #22306, .T. ) ;
#7851 = ORIENTED_EDGE ( 'NONE', *, *, #19116, .T. ) ;
#7852 = EDGE_CURVE ( 'NONE', #3598, #4273, #16088, .T. ) ;
#7853 = VECTOR ( 'NONE', #6805, 1000.000000000000000 ) ;
#7854 = CARTESIAN_POINT ( 'NONE',  ( 58.75000000000000711, 1.039502773796331159, 1.800471618825331355 ) ) ;
#7855 = CARTESIAN_POINT ( 'NONE',  ( 51.43355796162965987, -0.9748468443428969232, -1.443681521171313653 ) ) ;
#7856 = CARTESIAN_POINT ( 'NONE',  ( 54.38834410771541172, 6.716312262692355262, 2.020140340243033350 ) ) ;
#7857 = AXIS2_PLACEMENT_3D ( 'NONE', #11160, #15176, #20834 ) ;
#7858 = ORIENTED_EDGE ( 'NONE', *, *, #12665, .F. ) ;
#7859 = CARTESIAN_POINT ( 'NONE',  ( 50.40746642207052730, 1.341874354110782486, -3.874311046529112623 ) ) ;
#7860 = ORIENTED_EDGE ( 'NONE', *, *, #11047, .T. ) ;
#7861 = VECTOR ( 'NONE', #22461, 1000.000000000000000 ) ;
#7862 = CARTESIAN_POINT ( 'NONE',  ( 47.10000000000003695, 6.982261990806648555E-14, 4.599999999999874412 ) ) ;
#7863 = DIRECTION ( 'NONE',  ( 0.000000000000000000, 0.000000000000000000, 1.000000000000000000 ) ) ;
#7865 = DIRECTION ( 'NONE',  ( -0.03489949670250097613, -0.9993908270190957621, 0.000000000000000000 ) ) ;
#7864 = DIRECTION ( 'NONE',  ( 1.189524669241238948E-14, 0.000000000000000000, 1.000000000000000000 ) ) ;
#7866 = ORIENTED_EDGE ( 'NONE', *, *, #6050, .T. ) ;
#7867 = ORIENTED_EDGE ( 'NONE', *, *, #15803, .F. ) ;
#7868 = CARTESIAN_POINT ( 'NONE',  ( -53.99999999999997868, 0.000000000000000000, 4.700000000000000178 ) ) ;
#7869 = CARTESIAN_POINT ( 'NONE',  ( -59.69999999999997442, 3.400000000000007905, -2.001823990013003858E-13 ) ) ;
#7870 = EDGE_CURVE ( 'NONE', #30422, #26099, #20274, .T. ) ;
#7871 = VERTEX_POINT ( 'NONE', #295 ) ;
#7873 = FACE_OUTER_BOUND ( 'NONE', #19412, .T. ) ;
#7872 = CARTESIAN_POINT ( 'NONE',  ( 52.35001713925458944, 3.980960944483503017, 2.045629575386918919 ) ) ;
#7874 = CARTESIAN_POINT ( 'NONE',  ( -44.49999999999997868, 2.650000000000008349, -1.494059622532430298E-13 ) ) ;
#7875 = CARTESIAN_POINT ( 'NONE',  ( -57.24999999999996447, -2.489203624310585283, 2.804704140674917134 ) ) ;
#7876 = CARTESIAN_POINT ( 'NONE',  ( -64.29999999999996874, 2.249302195543353200, 0.05603242921607794191 ) ) ;
#7877 = CIRCLE ( 'NONE', #29609, 3.299999999999999822 ) ;
#7878 = CARTESIAN_POINT ( 'NONE',  ( 58.66122797211882300, 1.632010475559142915, -0.9232791089886424052 ) ) ;
#7879 = DIRECTION ( 'NONE',  ( 1.000000000000000000, 1.047444401652940007E-14, 0.000000000000000000 ) ) ;
#7880 = DIRECTION ( 'NONE',  ( 0.000000000000000000, 0.000000000000000000, 1.000000000000000000 ) ) ;
#7881 = CYLINDRICAL_SURFACE ( 'NONE', #29055, 0.9999999999999997780 ) ;
#7882 = CARTESIAN_POINT ( 'NONE',  ( -62.09999999999997300, -2.737158043526071172, 0.2654540351181889912 ) ) ;
#7884 = EDGE_CURVE ( 'NONE', #26613, #27565, #19637, .T. ) ;
#7883 = TOROIDAL_SURFACE ( 'NONE', #19027, 2.750000000000000000, 0.05000000000000000278 ) ;
#7885 = ORIENTED_EDGE ( 'NONE', *, *, #20587, .T. ) ;
#7886 = AXIS2_PLACEMENT_3D ( 'NONE', #2755, #10050, #7522 ) ;
#7887 = AXIS2_PLACEMENT_3D ( 'NONE', #20156, #29785, #25491 ) ;
#7888 = CONICAL_SURFACE ( 'NONE', #23596, 4.375000000000000000, 0.06758856876739828545 ) ;
#7889 = EDGE_CURVE ( 'NONE', #7150, #9227, #7727, .T. ) ;
#7890 = CARTESIAN_POINT ( 'NONE',  ( 16.10624235918716707, 3.046685255238750667, 4.470266847515931730 ) ) ;
#7891 = CARTESIAN_POINT ( 'NONE',  ( -60.61073679674431958, -2.503406555032712699, 0.9604922998729967798 ) ) ;
#7892 = AXIS2_PLACEMENT_3D ( 'NONE', #4289, #13938, #28218 ) ;
#7893 = CARTESIAN_POINT ( 'NONE',  ( -58.51905989232412253, 2.944486372867082924, 1.699999999999820099 ) ) ;
#7894 = EDGE_CURVE ( 'NONE', #27829, #18852, #28347, .T. ) ;
#7895 = ADVANCED_FACE ( 'NONE', ( #1079 ), #22635, .T. ) ;
#7896 = CIRCLE ( 'NONE', #11960, 4.700000000000000178 ) ;
#7897 = CARTESIAN_POINT ( 'NONE',  ( -58.32202994616203995, -4.156921938165296204, -2.492539235493512031E-13 ) ) ;
#7898 = DIRECTION ( 'NONE',  ( 1.344447539785323523E-44, -1.000000000000000000, -3.491481338843137300E-15 ) ) ;
#7899 = CARTESIAN_POINT ( 'NONE',  ( 22.79065618564551343, 6.593681752169803012, 2.049999999999919442 ) ) ;
#7900 = ORIENTED_EDGE ( 'NONE', *, *, #30437, .F. ) ;
#7901 = FACE_OUTER_BOUND ( 'NONE', #29581, .T. ) ;
#7902 = AXIS2_PLACEMENT_3D ( 'NONE', #4780, #10022, #26479 ) ;
#7903 = ORIENTED_EDGE ( 'NONE', *, *, #17400, .F. ) ;
#7904 = UNCERTAINTY_MEASURE_WITH_UNIT (LENGTH_MEASURE( 1.000000000000000082E-05 ), #13777, 'distance_accuracy_value', 'NONE');
#7905 = CARTESIAN_POINT ( 'NONE',  ( 68.00000000000007105, 1.401298464324817071E-42, 3.949999999999288303 ) ) ;
#7907 = CARTESIAN_POINT ( 'NONE',  ( 58.74840439586703411, -0.4999999999993848254, -1.859896009349159884 ) ) ;
#7906 = CARTESIAN_POINT ( 'NONE',  ( 69.25000000000004263, -0.8558823529411765385, 2.268940368965340237 ) ) ;
#7908 = STYLED_ITEM ( 'NONE', ( #13793 ), #15609 ) ;
#7909 = EDGE_LOOP ( 'NONE', ( #16096, #6216, #13480, #27106 ) ) ;
#7910 = EDGE_LOOP ( 'NONE', ( #27271, #19846, #10796, #18255 ) ) ;
#7911 = CARTESIAN_POINT ( 'NONE',  ( 51.80000000000001847, -0.1421112804877788793, -7.888760782825513275E-16 ) ) ;
#7912 = AXIS2_PLACEMENT_3D ( 'NONE', #14523, #14202, #21829 ) ;
#7913 = TOROIDAL_SURFACE ( 'NONE', #29653, 4.199999999999954881, 0.1000000000000000056 ) ;
#7914 = CARTESIAN_POINT ( 'NONE',  ( 47.38204862782191640, -3.967700393345040766, 1.365904513876657456 ) ) ;
#7915 = VERTEX_POINT ( 'NONE', #12782 ) ;
#7916 = AXIS2_PLACEMENT_3D ( 'NONE', #20802, #28385, #21432 ) ;
#7918 = CARTESIAN_POINT ( 'NONE',  ( -59.18789508915042319, 2.395752775956333291, 1.250136525132548915 ) ) ;
#7917 = CARTESIAN_POINT ( 'NONE',  ( -59.50952994616202574, 3.117691453623994580, -1.800000000000197664 ) ) ;
#7919 =( BOUNDED_SURFACE ( )  B_SPLINE_SURFACE ( 3, 2, ( 
 ( #24595, #5604, #29350 ),
 ( #5447, #383, #10339 ),
 ( #14927, #22246, #24898 ),
 ( #8129, #15097, #5130 ) ),
 .UNSPECIFIED., .F., .F., .F. ) 
 B_SPLINE_SURFACE_WITH_KNOTS ( ( 4, 4 ),
 ( 3, 3 ),
 ( 1.982313172862385287, 2.241731514487932841 ),
 ( 0.000000000000000000, 1.000000000000000000 ),
 .UNSPECIFIED. ) 
 GEOMETRIC_REPRESENTATION_ITEM ( )  RATIONAL_B_SPLINE_SURFACE ( (
 ( 1.000000000000000000, 0.8156258140602938855, 1.000000000000000000),
 ( 1.000000000000000000, 0.8356979842195433328, 1.000000000000000000),
 ( 1.000000000000000000, 0.8538860448759271193, 1.000000000000000000),
 ( 1.000000000000000000, 0.8699658093904928391, 1.000000000000000000) ) ) 
 REPRESENTATION_ITEM ( '' )  SURFACE ( )  );
#7920 = CARTESIAN_POINT ( 'NONE',  ( 50.38701762163459819, 1.088467210617599656, 3.899823238510140122 ) ) ;
#7921 = CARTESIAN_POINT ( 'NONE',  ( -36.77443515226921278, -4.926689578693618898, -2.233438676318209470 ) ) ;
#7922 = APPLICATION_PROTOCOL_DEFINITION ( 'draft international standard', 'automotive_design', 1998, #2661 ) ;
#7923 = CARTESIAN_POINT ( 'NONE',  ( 58.72419296898084440, -1.293880926823457900, -1.357170035999710089 ) ) ;
#7924 = SHAPE_REPRESENTATION_RELATIONSHIP ( 'NONE' , 'NONE' ,  #16755, #27821 ) ;
#7925 = AXIS2_PLACEMENT_3D ( 'NONE', #24997, #479, #5385 ) ;
#7926 = EDGE_CURVE ( 'NONE', #1734, #30371, #604, .T. ) ;
#7927 = CIRCLE ( 'NONE', #25613, 1.000000000000000000 ) ;
#7928 = VERTEX_POINT ( 'NONE', #15174 ) ;
#7929 = CIRCLE ( 'NONE', #21083, 1.000000000000000000 ) ;
#7930 = EDGE_CURVE ( 'NONE', #6393, #1641, #12345, .T. ) ;
#7931 = CARTESIAN_POINT ( 'NONE',  ( -57.38452994616203284, 2.093608279459370457E-14, -3.600000000000203926 ) ) ;
#7932 = TOROIDAL_SURFACE ( 'NONE', #16025, 4.800000000000000711, 0.05000000000000000278 ) ;
#7933 = EDGE_CURVE ( 'NONE', #30886, #29305, #5673, .T. ) ;
#7934 = CARTESIAN_POINT ( 'NONE',  ( 53.94136487687683967, 6.599443998687462454, -1.761196874214848052 ) ) ;
#7935 = CARTESIAN_POINT ( 'NONE',  ( -56.64405989232412253, -2.944486372867073154, -1.700000000000216893 ) ) ;
#7936 = DIRECTION ( 'NONE',  ( 1.000000000000000000, 3.053848253006669023E-16, -2.042510438544995415E-16 ) ) ;
#7937 =( GEOMETRIC_REPRESENTATION_CONTEXT ( 3 ) GLOBAL_UNCERTAINTY_ASSIGNED_CONTEXT ( ( #24385 ) ) GLOBAL_UNIT_ASSIGNED_CONTEXT ( ( #13495, #48, #4948 ) ) REPRESENTATION_CONTEXT ( 'NONE', 'WORKASPACE' ) );
#7938 = FACE_OUTER_BOUND ( 'NONE', #24670, .T. ) ;
#7939 = TOROIDAL_SURFACE ( 'NONE', #10471, 2.549999999999999822, 0.05000000000000000278 ) ;
#7940 = DIRECTION ( 'NONE',  ( 1.000000000000000000, 0.000000000000000000, -1.047444401652940007E-14 ) ) ;
#7941 = AXIS2_PLACEMENT_3D ( 'NONE', #15627, #5800, #23061 ) ;
#7943 = CARTESIAN_POINT ( 'NONE',  ( -36.39645873810206211, -0.5233326973448176878, -5.388419908789483515 ) ) ;
#7942 = CARTESIAN_POINT ( 'NONE',  ( 52.06628335902944826, 0.5434431642986584654, 1.794517909405660250 ) ) ;
#7944 = AXIS2_PLACEMENT_3D ( 'NONE', #20531, #11163, #18462 ) ;
#7945 = DIRECTION ( 'NONE',  ( 0.000000000000000000, 0.8740818021021506956, 0.4857787595540346559 ) ) ;
#7946 = CARTESIAN_POINT ( 'NONE',  ( 15.90468948301723628, -3.705258523861264752, 3.939862169952856874 ) ) ;
#7948 = CARTESIAN_POINT ( 'NONE',  ( -35.85663232820584057, -3.426725943139567576, 3.937891353488737423 ) ) ;
#7947 = FACE_OUTER_BOUND ( 'NONE', #13889, .T. ) ;
#7949 = EDGE_LOOP ( 'NONE', ( #519, #17011, #24384, #10045 ) ) ;
#7950 = CARTESIAN_POINT ( 'NONE',  ( 54.50000000000002132, 4.041334437186265510E-16, 3.299999999999999822 ) ) ;
#7951 = CARTESIAN_POINT ( 'NONE',  ( -67.99999999999997158, -3.266925685480267300E-16, 2.202315069465532498E-15 ) ) ;
#7952 = VECTOR ( 'NONE', #20562, 1000.000000000000000 ) ;
#7954 = CARTESIAN_POINT ( 'NONE',  ( -54.39999999999999147, -1.500000000000004663, 3.363870538531238186 ) ) ;
#7953 = CARTESIAN_POINT ( 'NONE',  ( 16.10624235918717062, 3.309998894527902635, -4.278958290368501949 ) ) ;
#7955 = CARTESIAN_POINT ( 'NONE',  ( 47.19248715958271845, -4.291463206566032085, 1.660299764304369319 ) ) ;
#7956 = ORIENTED_EDGE ( 'NONE', *, *, #31253, .F. ) ;
#7957 = DIRECTION ( 'NONE',  ( 0.000000000000000000, -1.000000000000000000, 0.000000000000000000 ) ) ;
#7958 = CARTESIAN_POINT ( 'NONE',  ( 47.01640678142056373, -4.158733306197476942, 1.045116725612200037 ) ) ;
#7959 = AXIS2_PLACEMENT_3D ( 'NONE', #28477, #18988, #28943 ) ;
#7960 =( BOUNDED_CURVE ( )  B_SPLINE_CURVE ( 3, ( #28665, #9028, #6981, #25486 ),
 .UNSPECIFIED., .F., .T. ) 
 B_SPLINE_CURVE_WITH_KNOTS ( ( 4, 4 ),
 ( 5.087525389280254551, 5.203235046317044699 ),
 .UNSPECIFIED. ) 
 CURVE ( )  GEOMETRIC_REPRESENTATION_ITEM ( )  RATIONAL_B_SPLINE_CURVE ( ( 1.000000000000000000, 0.9988845841160336469, 0.9988845841160336469, 1.000000000000000000 ) ) 
 REPRESENTATION_ITEM ( '' )  );
#7961 = VECTOR ( 'NONE', #25617, 1000.000000000000000 ) ;
#7962 = ORIENTED_EDGE ( 'NONE', *, *, #6748, .T. ) ;
#7963 = CARTESIAN_POINT ( 'NONE',  ( 58.75000000000002132, 6.153735859711025284E-13, 3.111507638930570854E-58 ) ) ;
#7964 = VERTEX_POINT ( 'NONE', #8205 ) ;
#7965 = ORIENTED_EDGE ( 'NONE', *, *, #7, .F. ) ;
#7966 = CARTESIAN_POINT ( 'NONE',  ( 15.70940947763170570, 4.797009389500183296, -2.498041539401762101 ) ) ;
#7967 = VERTEX_POINT ( 'NONE', #17389 ) ;
#7968 =( NAMED_UNIT ( * ) SI_UNIT ( $, .STERADIAN. ) SOLID_ANGLE_UNIT ( ) );
#7969 = CARTESIAN_POINT ( 'NONE',  ( 27.74852811682016096, 5.417024961191244437, 1.949999999999903810 ) ) ;
#7970 = CIRCLE ( 'NONE', #15029, 0.09999999999999986677 ) ;
#7971 = CARTESIAN_POINT ( 'NONE',  ( -60.13452994616204705, 3.117691453623979481, 1.799999999999798428 ) ) ;
#7972 = ORIENTED_EDGE ( 'NONE', *, *, #28613, .T. ) ;
#7973 = CARTESIAN_POINT ( 'NONE',  ( 54.49754940158101846, -0.002530889200285349212, 4.297001851131137862 ) ) ;
#7974 = CIRCLE ( 'NONE', #22132, 2.985355339059319046 ) ;
#7975 = AXIS2_PLACEMENT_3D ( 'NONE', #28651, #29111, #7428 ) ;
#7976 = DIRECTION ( 'NONE',  ( 0.9993908270190956511, -0.03489949670250096919, -3.491481338843132961E-15 ) ) ;
#7977 = CARTESIAN_POINT ( 'NONE',  ( 23.07431837909872741, 6.199584074734312722, 1.949999999999919575 ) ) ;
#7978 = VERTEX_POINT ( 'NONE', #933 ) ;
#7979 = EDGE_CURVE ( 'NONE', #23889, #10218, #16240, .T. ) ;
#7980 = DIRECTION ( 'NONE',  ( 0.000000000000000000, 0.000000000000000000, -1.000000000000000000 ) ) ;
#7981 = CARTESIAN_POINT ( 'NONE',  ( 49.00000000000004263, -0.7500000000000000000, 1.988246715072845117 ) ) ;
#7982 = DIRECTION ( 'NONE',  ( 0.000000000000000000, 0.4102564102564100201, 0.9119702176296790030 ) ) ;
#7983 = AXIS2_PLACEMENT_3D ( 'NONE', #30288, #18588, #22871 ) ;
#7984 = CARTESIAN_POINT ( 'NONE',  ( 56.96274124341056222, -0.7308628367038140228, -1.753832840855930719 ) ) ;
#7985 = CYLINDRICAL_SURFACE ( 'NONE', #8436, 0.1500000000000001887 ) ;
#7986 = CIRCLE ( 'NONE', #25674, 5.100000000000000533 ) ;
#7987 = AXIS2_PLACEMENT_3D ( 'NONE', #4748, #19347, #26910 ) ;
#7989 = CARTESIAN_POINT ( 'NONE',  ( 59.00000000000002132, 1.401298464324817071E-42, -6.179921969752347932E-13 ) ) ;
#7988 = CARTESIAN_POINT ( 'NONE',  ( -57.09585481156723574, 3.673546848079182414, 0.7533615035078063960 ) ) ;
#7990 = CARTESIAN_POINT ( 'NONE',  ( -54.49999999999997868, 8.366749974758391359E-15, -1.938977325913827332E-13 ) ) ;
#7991 = CARTESIAN_POINT ( 'NONE',  ( 15.03925126672132784, 4.804073783693472599, -2.042134687550301919 ) ) ;
#7992 = EDGE_CURVE ( 'NONE', #19238, #3444, #12189, .T. ) ;
#7993 = DIRECTION ( 'NONE',  ( 0.000000000000000000, 0.000000000000000000, 1.000000000000000000 ) ) ;
#7994 = LINE ( 'NONE', #5765, #23529 ) ;
#7995 = VERTEX_POINT ( 'NONE', #25143 ) ;
#7996 = DIRECTION ( 'NONE',  ( 1.000000000000000000, -1.219044193948983948E-29, 3.491481338843133355E-15 ) ) ;
#7997 = VERTEX_POINT ( 'NONE', #10730 ) ;
#7998 = VERTEX_POINT ( 'NONE', #30035 ) ;
#7999 = CARTESIAN_POINT ( 'NONE',  ( 50.40000000000001990, 0.6304760106459513791, 3.950000000000022826 ) ) ;
#8000 = CARTESIAN_POINT ( 'NONE',  ( -59.86042740578359656, -2.936324665650201116, -2.606018187048497303 ) ) ;
#8002 = CARTESIAN_POINT ( 'NONE',  ( -61.09509470490392147, -2.525749930366390394, 0.7571355657749674339 ) ) ;
#8001 = CARTESIAN_POINT ( 'NONE',  ( 15.90468948301722385, 4.892019442464165202, 2.306425897666068980 ) ) ;
#8003 = ORIENTED_EDGE ( 'NONE', *, *, #21296, .F. ) ;
#8004 = VERTEX_POINT ( 'NONE', #3141 ) ;
#8005 = CARTESIAN_POINT ( 'NONE',  ( 54.22146708689643191, 6.361260388417356637, -2.050000000000189004 ) ) ;
#8006 = CIRCLE ( 'NONE', #20154, 4.384222560975607585 ) ;
#8007 = VERTEX_POINT ( 'NONE', #10116 ) ;
#8008 = CARTESIAN_POINT ( 'NONE',  ( 51.47729133425608694, 0.9526829978903045282, -1.321356857234299520 ) ) ;
#8009 = VERTEX_POINT ( 'NONE', #27506 ) ;
#8010 = CARTESIAN_POINT ( 'NONE',  ( 26.00343446089717148, 5.312306467083453221, -2.050000000000090417 ) ) ;
#8011 = ORIENTED_EDGE ( 'NONE', *, *, #944, .T. ) ;
#8012 = CARTESIAN_POINT ( 'NONE',  ( -57.20655989232411542, 1.962990915244760659, -3.400000000000188205 ) ) ;
#8013 = CARTESIAN_POINT ( 'NONE',  ( 15.03925126672132961, 2.199885893005915527, 4.939696249117695892 ) ) ;
#8014 = EDGE_CURVE ( 'NONE', #7978, #17227, #4087, .T. ) ;
#8015 = CARTESIAN_POINT ( 'NONE',  ( 15.17256654081426248, -5.086913989685139192, -1.171642050077601249 ) ) ;
#8016 = CARTESIAN_POINT ( 'NONE',  ( -60.76905989232411542, 2.944486372867092250, 1.699999999999795675 ) ) ;
#8017 = CARTESIAN_POINT ( 'NONE',  ( 53.29207122288455878, 4.934008984266823994, -2.050000000000185896 ) ) ;
#8018 = CARTESIAN_POINT ( 'NONE',  ( 51.75427322675442809, -4.276948333784438283, -0.9210526315789454577 ) ) ;
#8019 = CYLINDRICAL_SURFACE ( 'NONE', #9598, 2.600000000000000089 ) ;
#8020 = DIRECTION ( 'NONE',  ( -1.000000000000000000, -0.000000000000000000, 3.491481338843133355E-15 ) ) ;
#8021 = CARTESIAN_POINT ( 'NONE',  ( -36.11692583559977976, -4.018128194441230150, -3.618665885216601819 ) ) ;
#8022 = AXIS2_PLACEMENT_3D ( 'NONE', #15672, #13261, #6166 ) ;
#8023 = AXIS2_PLACEMENT_3D ( 'NONE', #23004, #28048, #17939 ) ;
#8024 = CARTESIAN_POINT ( 'NONE',  ( 65.05000000000005400, 5.021051876503140601E-16, 4.099999999999318412 ) ) ;
#8025 = DIRECTION ( 'NONE',  ( 0.000000000000000000, -0.9996898646859344595, -0.02490330187381124827 ) ) ;
#8026 = VECTOR ( 'NONE', #27608, 1000.000000000000000 ) ;
#8027 = ADVANCED_FACE ( 'NONE', ( #14847 ), #25833, .T. ) ;
#8028 = ORIENTED_EDGE ( 'NONE', *, *, #26516, .F. ) ;
#8029 = CARTESIAN_POINT ( 'NONE',  ( -35.98994760229851408, -2.686240678227972190, -4.475885392924968897 ) ) ;
#8030 = CARTESIAN_POINT ( 'NONE',  ( 54.41366571437519895, 6.718673005292168376, -1.963089969304977700 ) ) ;
#8031 = ORIENTED_EDGE ( 'NONE', *, *, #8875, .T. ) ;
#8032 = CARTESIAN_POINT ( 'NONE',  ( 50.25000000000002842, -0.5380862305904318132, -2.008165151418244143 ) ) ;
#8033 = EDGE_LOOP ( 'NONE', ( #4016, #22809, #130, #11595 ) ) ;
#8034 = CARTESIAN_POINT ( 'NONE',  ( -55.34585481156723574, -2.489203624310586616, 2.804704140674918023 ) ) ;
#8036 = CARTESIAN_POINT ( 'NONE',  ( 51.59759607754882182, -3.813771782910184260, -1.508835477669506098 ) ) ;
#8035 = CARTESIAN_POINT ( 'NONE',  ( 48.34316787720665332, -1.211455355144519297, -3.917539841352833285 ) ) ;
#8037 = ADVANCED_FACE ( 'NONE', ( #24507 ), #29418, .F. ) ;
#8038 = ORIENTED_EDGE ( 'NONE', *, *, #10025, .T. ) ;
#8039 = CARTESIAN_POINT ( 'NONE',  ( 54.50000000000002132, 0.000000000000000000, 0.000000000000000000 ) ) ;
#8040 = CARTESIAN_POINT ( 'NONE',  ( 57.00221072626734298, -0.7147032416868923654, -1.808443027029684291 ) ) ;
#8041 = ORIENTED_EDGE ( 'NONE', *, *, #2325, .F. ) ;
#8043 = CARTESIAN_POINT ( 'NONE',  ( 51.80000000000001847, 4.100000000000047606, 2.275957200481583214E-14 ) ) ;
#8042 = CARTESIAN_POINT ( 'NONE',  ( 68.95000000000007390, 4.898587196589412829E-16, 3.999999999999277467 ) ) ;
#8044 = CARTESIAN_POINT ( 'NONE',  ( 58.75000000000002132, 6.153735859711025284E-13, 3.111507638930570854E-58 ) ) ;
#8045 = ORIENTED_EDGE ( 'NONE', *, *, #22825, .T. ) ;
#8046 = CARTESIAN_POINT ( 'NONE',  ( -59.49999999999997158, -2.489203624310586171, 2.804704140674917578 ) ) ;
#8047 = LINE ( 'NONE', #7876, #16572 ) ;
#8048 = CARTESIAN_POINT ( 'NONE',  ( 58.75000000694005564, 1.682988785001006793, -0.9428687169902416620 ) ) ;
#8049 = CIRCLE ( 'NONE', #17660, 0.2999999999999999334 ) ;
#8050 = ADVANCED_FACE ( 'NONE', ( #12474 ), #12632, .F. ) ;
#8051 = CARTESIAN_POINT ( 'NONE',  ( -54.49999999999998579, 0.03583423507999000668, -3.425661966777131973 ) ) ;
#8052 = DIRECTION ( 'NONE',  ( 1.000000000000000000, 1.047444401652940007E-14, 0.000000000000000000 ) ) ;
#8053 = EDGE_CURVE ( 'NONE', #19715, #5500, #7767, .T. ) ;
#8054 = PRODUCT ( 'Tip', 'Tip', '', ( #13898 ) ) ;
#8055 = CARTESIAN_POINT ( 'NONE',  ( -55.63452994616205416, 3.117691453623979481, 1.799999999999814415 ) ) ;
#8056 = ADVANCED_FACE ( 'NONE', ( #13246 ), #26137, .T. ) ;
#8057 = DIRECTION ( 'NONE',  ( 0.000000000000000000, 0.000000000000000000, 1.000000000000000000 ) ) ;
#8058 = ORIENTED_EDGE ( 'NONE', *, *, #30999, .T. ) ;
#8059 = CARTESIAN_POINT ( 'NONE',  ( 15.03925126672132784, -2.525801270006312382, 4.794550352686321126 ) ) ;
#8060 = AXIS2_PLACEMENT_3D ( 'NONE', #31023, #16943, #26588 ) ;
#8061 = CARTESIAN_POINT ( 'NONE',  ( -60.60807700862574166, -2.500243950683068928, 0.9573076586908287888 ) ) ;
#8062 = EDGE_CURVE ( 'NONE', #9539, #2309, #13566, .T. ) ;
#8063 = DIRECTION ( 'NONE',  ( 0.000000000000000000, -0.9996898646859344595, -0.02490330187381124480 ) ) ;
#8064 = CARTESIAN_POINT ( 'NONE',  ( -58.75952994616203284, 3.117691453624006126, -1.800000000000174794 ) ) ;
#8065 = COLOUR_RGB ( '', 0.40784314, 0.44705882, 0.49803922) ;
#8066 = CARTESIAN_POINT ( 'NONE',  ( -36.04518387042617888, 0.7747498539026829167, 5.363501450340917742 ) ) ;
#8067 = CARTESIAN_POINT ( 'NONE',  ( 30.16244940506470229, 6.784331066303296964, 2.049999999999894129 ) ) ;
#8068 = ORIENTED_EDGE ( 'NONE', *, *, #7132, .T. ) ;
#8069 = AXIS2_PLACEMENT_3D ( 'NONE', #26945, #3193, #12835 ) ;
#8070 = FACE_OUTER_BOUND ( 'NONE', #30748, .T. ) ;
#8071 = ORIENTED_EDGE ( 'NONE', *, *, #20534, .T. ) ;
#8072 = LINE ( 'NONE', #22810, #21706 ) ;
#8074 = FACE_OUTER_BOUND ( 'NONE', #12878, .T. ) ;
#8073 = CARTESIAN_POINT ( 'NONE',  ( 57.01550456668461209, 0.7366124869942373143, -2.429953032873097829 ) ) ;
#8075 = EDGE_CURVE ( 'NONE', #15123, #7818, #5645, .T. ) ;
#8076 = VERTEX_POINT ( 'NONE', #21029 ) ;
#8077 = ORIENTED_EDGE ( 'NONE', *, *, #28892, .F. ) ;
#8078 = PLANE ( 'NONE',  #4242 ) ;
#8079 = AXIS2_PLACEMENT_3D ( 'NONE', #9767, #18810, #19285 ) ;
#8080 = CARTESIAN_POINT ( 'NONE',  ( 29.69543387591358652, 6.938696499881336521, -1.425000000000103517 ) ) ;
#8081 = ORIENTED_EDGE ( 'NONE', *, *, #19438, .F. ) ;
#8083 = DIRECTION ( 'NONE',  ( 1.000000000000000000, 1.047444401652940007E-14, 0.000000000000000000 ) ) ;
#8082 = CARTESIAN_POINT ( 'NONE',  ( -55.94702994616203995, -2.078460969082631227, -3.600000000000205258 ) ) ;
#8084 = CARTESIAN_POINT ( 'NONE',  ( 50.30848954602731027, 1.391941090707534689, 3.850000000000023181 ) ) ;
#8085 = CARTESIAN_POINT ( 'NONE',  ( 51.80000000000001137, 3.949999999998452971, -1.950000000000180256 ) ) ;
#8086 = EDGE_CURVE ( 'NONE', #9490, #19242, #20340, .T. ) ;
#8087 = DIRECTION ( 'NONE',  ( -1.000000000000000000, -3.054025858079668409E-16, 2.042474015755241579E-16 ) ) ;
#8088 = ADVANCED_FACE ( 'NONE', ( #18342 ), #8806, .T. ) ;
#8089 = EDGE_CURVE ( 'NONE', #8546, #20739, #6292, .T. ) ;
#8090 = ORIENTED_EDGE ( 'NONE', *, *, #29132, .T. ) ;
#8091 = DIRECTION ( 'NONE',  ( -1.047444401652940007E-14, 0.000000000000000000, -1.000000000000000000 ) ) ;
#8092 = AXIS2_PLACEMENT_3D ( 'NONE', #919, #18183, #1067 ) ;
#8093 = CARTESIAN_POINT ( 'NONE',  ( 47.08691981199204690, -4.178911716362186723, -1.000646358242008205 ) ) ;
#8094 = CARTESIAN_POINT ( 'NONE',  ( 52.61915120152464453, 4.492597126270361230, -1.565330858589896845 ) ) ;
#8095 = CARTESIAN_POINT ( 'NONE',  ( 15.86395258069112124, -0.7247683022689926924, 5.358970532132270925 ) ) ;
#8096 = CARTESIAN_POINT ( 'NONE',  ( -54.87499999999998579, -3.920666489018356189E-15, 3.399999999999804068 ) ) ;
#8098 = CARTESIAN_POINT ( 'NONE',  ( 58.74999999999981526, -1.834410884275056386, -0.3880228184668537694 ) ) ;
#8097 = CARTESIAN_POINT ( 'NONE',  ( 50.25000000000003553, -1.666164585743077131, 1.106298139390331947 ) ) ;
#8099 = CARTESIAN_POINT ( 'NONE',  ( -62.10000000000010090, -2.520192335802873274, 0.1557817865423931636 ) ) ;
#8100 = FACE_OUTER_BOUND ( 'NONE', #10395, .T. ) ;
#8102 = CARTESIAN_POINT ( 'NONE',  ( -59.69464122902330416, 2.086944863889884871, 1.740854861534822273 ) ) ;
#8101 = DIRECTION ( 'NONE',  ( 0.000000000000000000, 0.000000000000000000, -1.000000000000000000 ) ) ;
#8103 = ORIENTED_EDGE ( 'NONE', *, *, #1306, .F. ) ;
#8104 = CARTESIAN_POINT ( 'NONE',  ( -44.49999999999997868, 1.499999999999999556, 4.029888335921975262 ) ) ;
#8105 = DIRECTION ( 'NONE',  ( 0.000000000000000000, 0.9996898646859343485, 0.02490330187381124133 ) ) ;
#8107 = DIRECTION ( 'NONE',  ( 1.000000000000000000, -0.000000000000000000, -1.047444401652940007E-14 ) ) ;
#8106 = CARTESIAN_POINT ( 'NONE',  ( 15.87128154250932610, 2.562020839648826431, -4.763023844700913223 ) ) ;
#8108 = PLANE ( 'NONE',  #2407 ) ;
#8109 = EDGE_CURVE ( 'NONE', #2034, #507, #16119, .T. ) ;
#8110 = VERTEX_POINT ( 'NONE', #4077 ) ;
#8111 = CARTESIAN_POINT ( 'NONE',  ( -61.39919398045554289, -2.652907018884305135, 0.5020538984275566552 ) ) ;
#8112 = DIRECTION ( 'NONE',  ( 1.054009200593503061E-14, 0.000000000000000000, 1.000000000000000000 ) ) ;
#8113 = EDGE_CURVE ( 'NONE', #1709, #30274, #1103, .T. ) ;
#8114 = ORIENTED_EDGE ( 'NONE', *, *, #23479, .T. ) ;
#8115 = EDGE_CURVE ( 'NONE', #14916, #30026, #17800, .T. ) ;
#8116 = CARTESIAN_POINT ( 'NONE',  ( -55.40835481156723574, -0.7533615035078004007, 3.673546848079179306 ) ) ;
#8117 = ORIENTED_EDGE ( 'NONE', *, *, #3762, .F. ) ;
#8118 = ORIENTED_EDGE ( 'NONE', *, *, #29176, .F. ) ;
#8119 = DIRECTION ( 'NONE',  ( -1.000000000000000000, -0.000000000000000000, 0.000000000000000000 ) ) ;
#8120 = VERTEX_POINT ( 'NONE', #28306 ) ;
#8121 = VECTOR ( 'NONE', #26676, 1000.000000000000000 ) ;
#8122 = CARTESIAN_POINT ( 'NONE',  ( 52.06789853512057675, 4.366897080361537675, -1.445771047857228542 ) ) ;
#8123 = CARTESIAN_POINT ( 'NONE',  ( -59.13452994616204705, -3.117691453623976816, 1.799999999999778000 ) ) ;
#8124 = ORIENTED_EDGE ( 'NONE', *, *, #4153, .F. ) ;
#8125 = CARTESIAN_POINT ( 'NONE',  ( 68.00000000000000000, -0.8382352941176474115, -2.222158093317993632 ) ) ;
#8126 = CARTESIAN_POINT ( 'NONE',  ( 48.40000000000001990, -4.899999999999999467, 4.100000000000022737 ) ) ;
#8127 = CARTESIAN_POINT ( 'NONE',  ( 26.00343446089713240, 5.312306467083714345, 2.049999999999908784 ) ) ;
#8128 = ORIENTED_EDGE ( 'NONE', *, *, #2418, .T. ) ;
#8129 = CARTESIAN_POINT ( 'NONE',  ( 51.59739104186226655, 1.010292945603183501, -1.272765950230259735 ) ) ;
#8130 = DIRECTION ( 'NONE',  ( 1.000000000000000000, 3.053848253006669023E-16, -2.042510438544995415E-16 ) ) ;
#8131 = CARTESIAN_POINT ( 'NONE',  ( 58.75000000000001421, 0.5380862305915540267, -1.858165151417984218 ) ) ;
#8132 = DIRECTION ( 'NONE',  ( 0.000000000000000000, 0.000000000000000000, -1.000000000000000000 ) ) ;
#8133 = CARTESIAN_POINT ( 'NONE',  ( 69.20000000000005969, -0.7500000000000000000, 1.988246715072633508 ) ) ;
#8135 = CARTESIAN_POINT ( 'NONE',  ( -44.59999999999995879, 1.433333333333357329, -4.054078878803043295 ) ) ;
#8134 = DIRECTION ( 'NONE',  ( 1.000000000000000000, 0.000000000000000000, 0.000000000000000000 ) ) ;
#8136 = VECTOR ( 'NONE', #2563, 1000.000000000000000 ) ;
#8137 = AXIS2_PLACEMENT_3D ( 'NONE', #8350, #15324, #17558 ) ;
#8138 = CARTESIAN_POINT ( 'NONE',  ( -60.84461143194912580, -2.378894296791489449, 0.8519906293918184659 ) ) ;
#8139 = DIRECTION ( 'NONE',  ( 3.083952846180964840E-15, 8.881784197001241477E-16, 1.000000000000000000 ) ) ;
#8140 = CARTESIAN_POINT ( 'NONE',  ( 58.65263613458535019, 1.277852321299496552, -1.372222488449735378 ) ) ;
#8141 = CARTESIAN_POINT ( 'NONE',  ( 53.97819099888265271, 5.744223774131685722, 2.011101020406490747 ) ) ;
#8142 = ORIENTED_EDGE ( 'NONE', *, *, #18936, .T. ) ;
#8143 = CARTESIAN_POINT ( 'NONE',  ( -54.49998431799114940, 1.548747819918198987, 3.331336553795240185 ) ) ;
#8144 = EDGE_CURVE ( 'NONE', #29040, #23306, #2623, .T. ) ;
#8145 = EDGE_CURVE ( 'NONE', #23567, #7041, #15252, .T. ) ;
#8146 = VERTEX_POINT ( 'NONE', #16273 ) ;
#8147 = ORIENTED_EDGE ( 'NONE', *, *, #30619, .F. ) ;
#8148 = EDGE_CURVE ( 'NONE', #13311, #3612, #577, .T. ) ;
#8149 = CARTESIAN_POINT ( 'NONE',  ( -59.12165399575386004, 2.320602887402581249, 1.283384167747377846 ) ) ;
#8150 = CARTESIAN_POINT ( 'NONE',  ( -58.17292740578360366, 2.256877952708268964, -2.542931754211925188 ) ) ;
#8152 = CARTESIAN_POINT ( 'NONE',  ( -59.69620733439754190, 2.084614077930948550, 1.743567435612995986 ) ) ;
#8151 = CARTESIAN_POINT ( 'NONE',  ( -55.93749999999996447, 1.962990915244749557, -3.400000000000189981 ) ) ;
#8153 = ORIENTED_EDGE ( 'NONE', *, *, #22798, .T. ) ;
#8154 = ORIENTED_EDGE ( 'NONE', *, *, #4524, .T. ) ;
#8155 = CARTESIAN_POINT ( 'NONE',  ( 53.81464057712624793, 5.799094425976102585, -1.689602626210267466 ) ) ;
#8156 = AXIS2_PLACEMENT_3D ( 'NONE', #21953, #4529, #4833 ) ;
#8157 = ORIENTED_EDGE ( 'NONE', *, *, #9126, .F. ) ;
#8158 = LINE ( 'NONE', #5780, #2018 ) ;
#8159 = ORIENTED_EDGE ( 'NONE', *, *, #4200, .T. ) ;
#8160 = CARTESIAN_POINT ( 'NONE',  ( 31.33102771648032459, 7.478136438692663646, -2.050000000000108180 ) ) ;
#8161 = VERTEX_POINT ( 'NONE', #11526 ) ;
#8162 = DIRECTION ( 'NONE',  ( 0.000000000000000000, 0.4295302013422852561, -0.9030524935654935526 ) ) ;
#8163 = CARTESIAN_POINT ( 'NONE',  ( -61.34999999999997300, -2.560800045841856942, 0.6641068371778564572 ) ) ;
#8164 = ORIENTED_EDGE ( 'NONE', *, *, #19725, .F. ) ;
#8165 = EDGE_CURVE ( 'NONE', #29519, #27339, #21861, .T. ) ;
#8166 = CARTESIAN_POINT ( 'NONE',  ( 15.76675455518220303, -5.174628573245093399, -1.572974725650858385 ) ) ;
#8167 = CARTESIAN_POINT ( 'NONE',  ( -57.33155989232411542, -1.962990915244706924, -3.400000000000209521 ) ) ;
#8168 = CARTESIAN_POINT ( 'NONE',  ( 47.44326941947779375, -3.851351755029098101, 1.408485093544704192 ) ) ;
#8169 = CARTESIAN_POINT ( 'NONE',  ( 47.00000000000000711, -3.700421601131886007, -1.984561589293904582 ) ) ;
#8170 = AXIS2_PLACEMENT_3D ( 'NONE', #12358, #2415, #19367 ) ;
#8171 = CARTESIAN_POINT ( 'NONE',  ( 50.56951033778286586, 0.1019484954154457890, 1.190698274346101648 ) ) ;
#8172 = CYLINDRICAL_SURFACE ( 'NONE', #28140, 0.1500000000000001887 ) ;
#8174 = CARTESIAN_POINT ( 'NONE',  ( 51.80288952865482344, -4.086537470739417088, 2.116255473933748910 ) ) ;
#8173 = CARTESIAN_POINT ( 'NONE',  ( -59.42430006944807275, 3.327103312532478263, 1.272610237773433184 ) ) ;
#8175 = B_SPLINE_CURVE_WITH_KNOTS ( 'NONE', 3,
 ( #5907, #13022, #17313, #5742, #15392, #25042 ),
 .UNSPECIFIED., .F., .F.,
 ( 4, 2, 4 ),
 ( 0.000000000000000000, 8.451199622854574779E-05, 0.0001690239924570914956 ),
 .UNSPECIFIED. ) ;
#8176 = CARTESIAN_POINT ( 'NONE',  ( -58.40835481156724285, -0.7533615035077920741, 3.673546848079180638 ) ) ;
#8177 = DIRECTION ( 'NONE',  ( 0.9993908270190957621, -0.03489949670250100389, -3.492120980335537899E-15 ) ) ;
#8178 = CIRCLE ( 'NONE', #27881, 1.000000000000000000 ) ;
#8179 = CARTESIAN_POINT ( 'NONE',  ( 51.47729133425627168, -0.9526829978892129569, 1.321356857233838777 ) ) ;
#8180 = ORIENTED_EDGE ( 'NONE', *, *, #2379, .F. ) ;
#8181 = DIRECTION ( 'NONE',  ( 1.027984282060330001E-14, 0.000000000000000000, 1.000000000000000000 ) ) ;
#8182 = CARTESIAN_POINT ( 'NONE',  ( 54.28867365409853107, 5.640057820322910587, -0.9750000000001823874 ) ) ;
#8183 = ORIENTED_EDGE ( 'NONE', *, *, #26237, .F. ) ;
#8184 = EDGE_CURVE ( 'NONE', #18396, #14402, #8178, .T. ) ;
#8185 = CARTESIAN_POINT ( 'NONE',  ( 48.30000000000001847, 2.428612866367529932E-14, 0.000000000000000000 ) ) ;
#8186 = ORIENTED_EDGE ( 'NONE', *, *, #26897, .T. ) ;
#8187 = CARTESIAN_POINT ( 'NONE',  ( 15.03925126672132961, -1.123735532908281431, -5.289358697221548056 ) ) ;
#8188 = CARTESIAN_POINT ( 'NONE',  ( -36.11187263677951620, -5.068523420888918274, 1.228242390833657049 ) ) ;
#8190 = CARTESIAN_POINT ( 'NONE',  ( 50.50000000000002132, -0.6304760106459033064, -3.950000000000021938 ) ) ;
#8189 = DIRECTION ( 'NONE',  ( 1.000000000000000000, 3.054025858079668409E-16, -2.042474015755241579E-16 ) ) ;
#8191 = ORIENTED_EDGE ( 'NONE', *, *, #27718, .T. ) ;
#8192 = CARTESIAN_POINT ( 'NONE',  ( 61.00000000000003553, -0.8666666666660277629, -1.374595900215364708 ) ) ;
#8193 = CARTESIAN_POINT ( 'NONE',  ( 57.01635142493560693, -0.7373792903891465134, -1.789496335369930025 ) ) ;
#8194 = ORIENTED_EDGE ( 'NONE', *, *, #17120, .F. ) ;
#8196 = CYLINDRICAL_SURFACE ( 'NONE', #386, 1.000000000000000000 ) ;
#8195 = DIRECTION ( 'NONE',  ( 0.000000000000000000, 0.7438053426816615410, -0.6683962987616075546 ) ) ;
#8197 = CARTESIAN_POINT ( 'NONE',  ( -56.72499999999997300, -0.9643027244899884387, 4.702139965541347166 ) ) ;
#8198 = ORIENTED_EDGE ( 'NONE', *, *, #9738, .F. ) ;
#8199 = CARTESIAN_POINT ( 'NONE',  ( 58.75000000000003553, -1.323060376181803832, 1.499837071478349326 ) ) ;
#8200 = AXIS2_PLACEMENT_3D ( 'NONE', #17064, #7086, #19751 ) ;
#8201 = DIRECTION ( 'NONE',  ( -1.000000000000000000, -3.054025858079668409E-16, 2.042474015755241579E-16 ) ) ;
#8202 = CARTESIAN_POINT ( 'NONE',  ( 58.72419296898052465, 1.645806614395798340, -0.8985315506020565834 ) ) ;
#8203 = EDGE_CURVE ( 'NONE', #26062, #23038, #30918, .T. ) ;
#8204 = CARTESIAN_POINT ( 'NONE',  ( -36.89831264271880684, -2.941172302009062545, 4.539591111929643041 ) ) ;
#8205 = CARTESIAN_POINT ( 'NONE',  ( 34.56702326949724835, 8.213851659285209550, -1.550000000000119948 ) ) ;
#8206 = CARTESIAN_POINT ( 'NONE',  ( 69.00000000000001421, 1.401298464324817071E-42, -7.227366371405287181E-13 ) ) ;
#8207 = ORIENTED_EDGE ( 'NONE', *, *, #4693, .F. ) ;
#8208 = CARTESIAN_POINT ( 'NONE',  ( 15.03925126672122836, 2.199885893005901316, 4.939696249117701221 ) ) ;
#8209 = AXIS2_PLACEMENT_3D ( 'NONE', #1992, #16731, #28277 ) ;
#8210 = CARTESIAN_POINT ( 'NONE',  ( -60.64271989919365780, -2.512715456726746677, 0.9876222387486196519 ) ) ;
#8211 = DIRECTION ( 'NONE',  ( 1.047444401652940007E-14, 0.000000000000000000, 1.000000000000000000 ) ) ;
#8212 = CARTESIAN_POINT ( 'NONE',  ( -57.00952994616205416, -7.288692778928185739E-15, 3.599999999999796696 ) ) ;
#8213 = CARTESIAN_POINT ( 'NONE',  ( 58.73379417893116994, -1.873409305145653292, 0.08040888200709349343 ) ) ;
#8214 = CARTESIAN_POINT ( 'NONE',  ( 23.38432935081488395, 6.109573960516228475, 2.049999999999918554 ) ) ;
#8215 = ORIENTED_EDGE ( 'NONE', *, *, #28349, .F. ) ;
#8216 = EDGE_CURVE ( 'NONE', #13291, #17296, #15798, .T. ) ;
#8217 = DIRECTION ( 'NONE',  ( 0.000000000000000000, 0.000000000000000000, -1.000000000000000000 ) ) ;
#8218 = ORIENTED_EDGE ( 'NONE', *, *, #28589, .T. ) ;
#8219 = UNCERTAINTY_MEASURE_WITH_UNIT (LENGTH_MEASURE( 1.000000000000000082E-05 ), #19508, 'distance_accuracy_value', 'NONE');
#8220 = CARTESIAN_POINT ( 'NONE',  ( 51.85262340636813150, -0.6891204047484758011, 1.750401715244590539 ) ) ;
#8222 = CARTESIAN_POINT ( 'NONE',  ( 58.73379417893119836, -1.267842757871934012, 1.381558089341300422 ) ) ;
#8221 = CARTESIAN_POINT ( 'NONE',  ( 51.25000000000001421, 0.6500000000005367040, 1.489337100860647967 ) ) ;
#8223 = ORIENTED_EDGE ( 'NONE', *, *, #16848, .T. ) ;
#8224 = VERTEX_POINT ( 'NONE', #26240 ) ;
#8225 = DIRECTION ( 'NONE',  ( 1.000000000000000000, 0.000000000000000000, -3.491481338843133355E-15 ) ) ;
#8226 = CARTESIAN_POINT ( 'NONE',  ( -44.59999999999999432, -1.400000000000007017, 3.959797974644484242 ) ) ;
#8227 = VERTEX_POINT ( 'NONE', #24185 ) ;
#8229 = FACE_OUTER_BOUND ( 'NONE', #10103, .T. ) ;
#8228 = CARTESIAN_POINT ( 'NONE',  ( -59.25952994616205416, -4.643455692769875931E-15, 3.599999999999788702 ) ) ;
#8230 = CARTESIAN_POINT ( 'NONE',  ( -58.73542740578359656, 2.936324665650206889, 2.606018187048499080 ) ) ;
#8231 = AXIS2_PLACEMENT_3D ( 'NONE', #12767, #29875, #30019 ) ;
#8232 = FACE_OUTER_BOUND ( 'NONE', #14769, .T. ) ;
#8233 = APPLICATION_PROTOCOL_DEFINITION ( 'draft international standard', 'automotive_design', 1998, #9144 ) ;
#8234 = EDGE_CURVE ( 'NONE', #7417, #22240, #25873, .T. ) ;
#8235 = CARTESIAN_POINT ( 'NONE',  ( 58.73371041428924144, -1.267950628961127757, -1.381461519773210522 ) ) ;
#8236 = PRESENTATION_STYLE_ASSIGNMENT (( #5558 ) ) ;
#8237 = ORIENTED_EDGE ( 'NONE', *, *, #10400, .T. ) ;
#8238 = FACE_OUTER_BOUND ( 'NONE', #18648, .T. ) ;
#8239 = CARTESIAN_POINT ( 'NONE',  ( 52.11477178369203500, 3.843881278534198476, -2.050000000000181455 ) ) ;
#8240 = CARTESIAN_POINT ( 'NONE',  ( 48.47204894654066010, -1.409900792624738886, -3.850000304694921827 ) ) ;
#8241 = DIRECTION ( 'NONE',  ( 2.614375865348241018E-16, -0.2008964009354148039, 0.9796124928211140670 ) ) ;
#8242 = ADVANCED_FACE ( 'NONE', ( #14348 ), #23723, .F. ) ;
#8243 = CARTESIAN_POINT ( 'NONE',  ( 57.04413099161754985, -0.7497394063391640273, -2.421432380119032501 ) ) ;
#8245 = CARTESIAN_POINT ( 'NONE',  ( 58.75000018803721957, -1.857237022264228044, -0.5488434064257393663 ) ) ;
#8244 = CYLINDRICAL_SURFACE ( 'NONE', #5940, 0.1000000000000000472 ) ;
#8246 = AXIS2_PLACEMENT_3D ( 'NONE', #5029, #24202, #2510 ) ;
#8247 = CARTESIAN_POINT ( 'NONE',  ( -62.09999999999997300, -2.520404473256288469, 0.1522704540930145123 ) ) ;
#8249 = CARTESIAN_POINT ( 'NONE',  ( 51.80000000000001847, -3.726179070414207928, -1.100000000000000089 ) ) ;
#8248 = DIRECTION ( 'NONE',  ( 1.000000000000000000, 1.786976680021873984E-16, 2.459562394685737870E-16 ) ) ;
#8250 = ORIENTED_EDGE ( 'NONE', *, *, #11931, .F. ) ;
#8251 = EDGE_CURVE ( 'NONE', #20165, #29437, #17066, .T. ) ;
#8252 = CARTESIAN_POINT ( 'NONE',  ( 50.33814819168215138, -1.426738236278548566, -3.843750512866276559 ) ) ;
#8253 = EDGE_CURVE ( 'NONE', #11810, #2222, #29365, .T. ) ;
#8254 = DIRECTION ( 'NONE',  ( 1.000000000000000000, 1.047444401652940007E-14, 0.000000000000000000 ) ) ;
#8256 = CARTESIAN_POINT ( 'NONE',  ( -59.68687113065863059, -2.402179451507847396, -1.230958653213905851 ) ) ;
#8255 = CARTESIAN_POINT ( 'NONE',  ( 15.67083574136752411, 2.849134329833903578, -4.601168830303363322 ) ) ;
#8258 = EDGE_CURVE ( 'NONE', #16066, #30797, #21968, .T. ) ;
#8257 = CARTESIAN_POINT ( 'NONE',  ( 57.02185466405004632, 0.7499999999999981126, 2.421260014775926006 ) ) ;
#8259 = ORIENTED_EDGE ( 'NONE', *, *, #2046, .T. ) ;
#8260 = CARTESIAN_POINT ( 'NONE',  ( 54.23831472968567624, 6.535030234825929263, 2.049999999999810640 ) ) ;
#8261 = CARTESIAN_POINT ( 'NONE',  ( 47.03864569166055531, -4.169908074913990070, 1.021033875312352235 ) ) ;
#8262 = VERTEX_POINT ( 'NONE', #21825 ) ;
#8263 = DIRECTION ( 'NONE',  ( 0.000000000000000000, 0.000000000000000000, 1.000000000000000000 ) ) ;
#8264 = ORIENTED_EDGE ( 'NONE', *, *, #30713, .F. ) ;
#8265 = CARTESIAN_POINT ( 'NONE',  ( 15.71019289815287223, 3.857619034241809075, -3.790808625283980771 ) ) ;
#8266 = CARTESIAN_POINT ( 'NONE',  ( -44.49999999999999289, 0.000000000000000000, 4.299999999999998046 ) ) ;
#8267 = ORIENTED_EDGE ( 'NONE', *, *, #10520, .F. ) ;
#8268 = DIRECTION ( 'NONE',  ( 0.000000000000000000, -1.517883041479702421E-14, 1.000000000000000000 ) ) ;
#8269 = CARTESIAN_POINT ( 'NONE',  ( -54.89405989232412963, 2.944486372867106461, -1.700000000000182254 ) ) ;
#8270 = ORIENTED_EDGE ( 'NONE', *, *, #4217, .T. ) ;
#8271 = DIRECTION ( 'NONE',  ( 1.000000000000000000, 0.000000000000000000, 0.000000000000000000 ) ) ;
#8272 = AXIS2_PLACEMENT_3D ( 'NONE', #8032, #14829, #17697 ) ;
#8273 = CARTESIAN_POINT ( 'NONE',  ( -35.85663232820584057, -3.056483311920853208, -4.206888370749738648 ) ) ;
#8274 = CARTESIAN_POINT ( 'NONE',  ( 23.88937651017007369, 5.720041407194654148, 1.949999999999850075 ) ) ;
#8275 = VERTEX_POINT ( 'NONE', #9472 ) ;
#8276 = CARTESIAN_POINT ( 'NONE',  ( -55.93749999999996447, 1.962990915244749557, -3.400000000000189981 ) ) ;
#8277 = CARTESIAN_POINT ( 'NONE',  ( -57.31249999999996447, -0.7533615035078060629, 3.673546848079176197 ) ) ;
#8278 = CARTESIAN_POINT ( 'NONE',  ( -61.34999999999997300, -2.515554072771550853, -0.7899129066418597578 ) ) ;
#8279 = CARTESIAN_POINT ( 'NONE',  ( -74.38999999999998636, -2.585162900687033808E-15, 4.707972083073595634E-15 ) ) ;
#8280 = EDGE_CURVE ( 'NONE', #6307, #6992, #3614, .T. ) ;
#8281 = DIRECTION ( 'NONE',  ( 0.000000000000000000, -1.224646799147353207E-16, 1.000000000000000000 ) ) ;
#8282 = ADVANCED_FACE ( 'NONE', ( #31300 ), #28616, .T. ) ;
#8284 = CARTESIAN_POINT ( 'NONE',  ( -54.39999999999999147, 1.399999999999995914, 3.959797974644419849 ) ) ;
#8283 = CARTESIAN_POINT ( 'NONE',  ( 51.80000000000001137, -3.936726248589971444, -1.145507068360074765 ) ) ;
#8285 =( BOUNDED_SURFACE ( )  B_SPLINE_SURFACE ( 3, 2, ( 
 ( #7201, #9736, #14631 ),
 ( #9592, #28570, #26355 ),
 ( #4658, #22086, #12396 ),
 ( #21936, #7515, #26823 ),
 ( #16865, #381, #18925 ),
 ( #6879, #16550, #11787 ),
 ( #19251, #14312, #17177 ),
 ( #4808, #26200, #26678 ),
 ( #4505, #4976, #2280 ),
 ( #23982, #5126, #29039 ),
 ( #24296, #2606, #29202 ),
 ( #11943, #14470, #14779 ),
 ( #12252, #75, #31264 ),
 ( #19398, #2452, #7349 ),
 ( #24143, #21633, #14160 ),
 ( #23833, #21790, #31093 ),
 ( #220, #9881, #19556 ),
 ( #24439, #20009, #10336 ),
 ( #10511, #7801, #20338 ),
 ( #8127, #10044, #5272 ),
 ( #27123, #5445, #15980 ),
 ( #26963, #29650, #17798 ),
 ( #12707, #5749, #22539 ),
 ( #3214, #20183, #27285 ),
 ( #1006, #29966, #8274 ),
 ( #17318, #19714, #3063 ),
 ( #12857, #843, #7977 ),
 ( #14922, #17640, #5602 ),
 ( #25051, #13593, #29815 ),
 ( #27436, #530, #17471 ),
 ( #15398, #10660, #6326 ),
 ( #17942, #27585, #15250 ),
 ( #3380, #15095, #13030 ),
 ( #24753, #24896, #22711 ) ),
 .UNSPECIFIED., .F., .F., .F. ) 
 B_SPLINE_SURFACE_WITH_KNOTS ( ( 4, 2, 2, 2, 2, 2, 2, 2, 2, 2, 2, 2, 2, 2, 2, 2, 4 ),
 ( 3, 3 ),
 ( -1.734723475976807094E-18, 0.001741451497654487477, 0.002612177246481731975, 0.003047540120895354115, 0.003482902995308976690, 0.004353628744136221404, 0.005224354492963465685, 0.006965805990617955114, 0.007836531739445200262, 0.008707257488272444543, 0.009577983237099688824, 0.01044870898592693310, 0.01131943473475417739, 0.01219016048358142340, 0.01262552335799504641, 0.01306088623240866768, 0.01393161198123591196 ),
 ( 0.000000000000000000, 1.000000000000000000 ),
 .UNSPECIFIED. ) 
 GEOMETRIC_REPRESENTATION_ITEM ( )  RATIONAL_B_SPLINE_SURFACE ( (
 ( 1.000000000000000000, 0.7071067811865467956, 1.000000000000000000),
 ( 1.000000000000000000, 0.7071067811865467956, 1.000000000000000000),
 ( 1.000000000000000000, 0.7071067811865482389, 1.000000000000000000),
 ( 1.000000000000000000, 0.7071067811865482389, 1.000000000000000000),
 ( 1.000000000000000000, 0.7071067811865467956, 1.000000000000000000),
 ( 1.000000000000000000, 0.7071067811865467956, 1.000000000000000000),
 ( 1.000000000000000000, 0.7071067811865475727, 1.000000000000000000),
 ( 1.000000000000000000, 0.7071067811865475727, 1.000000000000000000),
 ( 1.000000000000000000, 0.7071067811865425767, 1.000000000000000000),
 ( 1.000000000000000000, 0.7071067811865425767, 1.000000000000000000),
 ( 1.000000000000000000, 0.7071067811865441310, 1.000000000000000000),
 ( 1.000000000000000000, 0.7071067811865441310, 1.000000000000000000),
 ( 1.000000000000000000, 0.7071067811865494601, 1.000000000000000000),
 ( 1.000000000000000000, 0.7071067811865494601, 1.000000000000000000),
 ( 1.000000000000000000, 0.7071067811865467956, 1.000000000000000000),
 ( 1.000000000000000000, 0.7071067811865467956, 1.000000000000000000),
 ( 1.000000000000000000, 0.7071067811865406894, 1.000000000000000000),
 ( 1.000000000000000000, 0.7071067811865406894, 1.000000000000000000),
 ( 1.000000000000000000, 0.7071067811865483499, 1.000000000000000000),
 ( 1.000000000000000000, 0.7071067811865483499, 1.000000000000000000),
 ( 1.000000000000000000, 0.7071067811865475727, 1.000000000000000000),
 ( 1.000000000000000000, 0.7071067811865475727, 1.000000000000000000),
 ( 1.000000000000000000, 0.7071067811865475727, 1.000000000000000000),
 ( 1.000000000000000000, 0.7071067811865475727, 1.000000000000000000),
 ( 1.000000000000000000, 0.7071067811865497932, 1.000000000000000000),
 ( 1.000000000000000000, 0.7071067811865497932, 1.000000000000000000),
 ( 1.000000000000000000, 0.7071067811865565655, 1.000000000000000000),
 ( 1.000000000000000000, 0.7071067811865565655, 1.000000000000000000),
 ( 1.000000000000000000, 0.7071067811865490160, 1.000000000000000000),
 ( 1.000000000000000000, 0.7071067811865490160, 1.000000000000000000),
 ( 1.000000000000000000, 0.7071067811865389130, 1.000000000000000000),
 ( 1.000000000000000000, 0.7071067811865389130, 1.000000000000000000),
 ( 1.000000000000000000, 0.7071067811865361374, 1.000000000000000000),
 ( 1.000000000000000000, 0.7071067811865361374, 1.000000000000000000) ) ) 
 REPRESENTATION_ITEM ( '' )  SURFACE ( )  );
#8286 = DIRECTION ( 'NONE',  ( -1.000000000000000000, -3.053848253006669023E-16, 2.042510438544995415E-16 ) ) ;
#8287 = DIRECTION ( 'NONE',  ( -3.491481338843133355E-15, 0.000000000000000000, -1.000000000000000000 ) ) ;
#8288 = LINE ( 'NONE', #4007, #26104 ) ;
#8289 = CARTESIAN_POINT ( 'NONE',  ( 58.75000018803716983, 1.403930843797543293, -1.333992738915948051 ) ) ;
#8290 = CARTESIAN_POINT ( 'NONE',  ( -57.72499999999997300, 2.811319000628834039E-15, 1.036730182770210180E-16 ) ) ;
#8291 = VECTOR ( 'NONE', #8680, 1000.000000000000000 ) ;
#8292 = ORIENTED_EDGE ( 'NONE', *, *, #12677, .F. ) ;
#8293 = DIRECTION ( 'NONE',  ( 0.000000000000000000, 0.000000000000000000, -1.000000000000000000 ) ) ;
#8294 = FACE_OUTER_BOUND ( 'NONE', #11412, .T. ) ;
#8295 = ORIENTED_EDGE ( 'NONE', *, *, #19916, .F. ) ;
#8296 = ORIENTED_EDGE ( 'NONE', *, *, #25943, .F. ) ;
#8297 = FACE_OUTER_BOUND ( 'NONE', #11888, .T. ) ;
#8298 = CARTESIAN_POINT ( 'NONE',  ( -57.48542740578361077, 0.7887156198831664078, -3.845940847736174284 ) ) ;
#8300 = DIRECTION ( 'NONE',  ( -4.636120533309209166E-15, 0.3099561728519886206, -0.9507508458639142290 ) ) ;
#8299 = CARTESIAN_POINT ( 'NONE',  ( -55.56249999999998579, -1.962990915244731793, 3.399999999999794742 ) ) ;
#8301 = ORIENTED_EDGE ( 'NONE', *, *, #8777, .F. ) ;
#8302 = ORIENTED_EDGE ( 'NONE', *, *, #22179, .F. ) ;
#8303 = AXIS2_PLACEMENT_3D ( 'NONE', #27184, #5494, #10091 ) ;
#8304 = DIRECTION ( 'NONE',  ( -4.439792124536519685E-15, 0.3099561728528805182, -0.9507508458636233506 ) ) ;
#8305 = ORIENTED_EDGE ( 'NONE', *, *, #22796, .T. ) ;
#8306 = FACE_OUTER_BOUND ( 'NONE', #19591, .T. ) ;
#8307 = ORIENTED_EDGE ( 'NONE', *, *, #31164, .F. ) ;
#8308 = DIRECTION ( 'NONE',  ( 0.000000000000000000, -1.000000000000000000, -3.491481338843133355E-15 ) ) ;
#8309 = B_SPLINE_CURVE_WITH_KNOTS ( 'NONE', 3,
 ( #22366, #21768, #12374, #5580, #509, #26650, #12090, #7781, #17157, #24120 ),
 .UNSPECIFIED., .F., .F.,
 ( 4, 2, 2, 2, 4 ),
 ( 4.336808689942017255E-19, 0.0003923434276460365509, 0.0007846868552920726681, 0.001177030282938108839, 0.001569373710584144902 ),
 .UNSPECIFIED. ) ;
#8310 = CARTESIAN_POINT ( 'NONE',  ( 54.41366571437522026, 6.718673005292167488, 1.976179938779723422 ) ) ;
#8311 = DIRECTION ( 'NONE',  ( -1.000000000000000000, 0.000000000000000000, 3.491481338843133355E-15 ) ) ;
#8313 = CARTESIAN_POINT ( 'NONE',  ( -58.95655989232412253, -3.925981830489445379, -2.234056176427713674E-13 ) ) ;
#8312 = CIRCLE ( 'NONE', #24014, 0.04999999999999988481 ) ;
#8314 = CARTESIAN_POINT ( 'NONE',  ( -57.65835481156722864, -0.7533615035078039535, 3.673546848079178861 ) ) ;
#8315 = EDGE_CURVE ( 'NONE', #7461, #21159, #18338, .T. ) ;
#8316 = CARTESIAN_POINT ( 'NONE',  ( 47.73776917354344818, -3.930699233196665254, -1.170919866331572079 ) ) ;
#8317 = ADVANCED_FACE ( 'NONE', ( #21358 ), #14203, .T. ) ;
#8318 = CARTESIAN_POINT ( 'NONE',  ( 48.50000000000002132, 1.391941090707534023, 3.850000000000022737 ) ) ;
#8319 = EDGE_CURVE ( 'NONE', #13545, #29070, #27386, .T. ) ;
#8320 = CARTESIAN_POINT ( 'NONE',  ( 58.75000002382375897, -0.5510104498256471750, 1.849358057802746425 ) ) ;
#8322 = CARTESIAN_POINT ( 'NONE',  ( 51.30632327778202040, -4.280384112422016329, 1.378579207634347936 ) ) ;
#8321 = DIRECTION ( 'NONE',  ( 1.000000000000000000, 1.047444401652940007E-14, 0.000000000000000000 ) ) ;
#8323 = DIRECTION ( 'NONE',  ( 0.000000000000000000, 0.2745098039215673746, 0.9615843008030769967 ) ) ;
#8324 = CARTESIAN_POINT ( 'NONE',  ( 51.50435016707359637, -0.9265794315402090531, 1.339215852266876672 ) ) ;
#8325 = EDGE_LOOP ( 'NONE', ( #16996, #8305, #8342, #13316 ) ) ;
#8326 = VECTOR ( 'NONE', #15423, 1000.000000000000000 ) ;
#8327 = AXIS2_PLACEMENT_3D ( 'NONE', #18128, #20803, #30433 ) ;
#8328 = CARTESIAN_POINT ( 'NONE',  ( 50.59602332238209499, 0.1408342061609073048, 0.8215393206232031176 ) ) ;
#8329 = CARTESIAN_POINT ( 'NONE',  ( 54.44213313387141540, 6.358439080500951412, 1.988253682540942258 ) ) ;
#8330 = EDGE_LOOP ( 'NONE', ( #4294, #1028, #11886, #9103 ) ) ;
#8331 = ADVANCED_FACE ( 'NONE', ( #14672 ), #2640, .T. ) ;
#8332 = DIRECTION ( 'NONE',  ( 0.000000000000000000, 1.000000000000000000, 0.000000000000000000 ) ) ;
#8333 = ORIENTED_EDGE ( 'NONE', *, *, #6824, .T. ) ;
#8334 = CARTESIAN_POINT ( 'NONE',  ( 15.56401610563845850, -1.027070083875938566, -5.312835761376674348 ) ) ;
#8335 = AXIS2_PLACEMENT_3D ( 'NONE', #27276, #25038, #7507 ) ;
#8336 = FACE_OUTER_BOUND ( 'NONE', #26707, .T. ) ;
#8338 = CARTESIAN_POINT ( 'NONE',  ( -54.49999999999997868, 1.549999999999999600, -3.300094695611021312 ) ) ;
#8337 = FACE_OUTER_BOUND ( 'NONE', #30706, .T. ) ;
#8339 = ORIENTED_EDGE ( 'NONE', *, *, #10194, .F. ) ;
#8340 = DIRECTION ( 'NONE',  ( 1.000000000000000000, 3.053848253006669023E-16, -2.042510438544995415E-16 ) ) ;
#8341 = CARTESIAN_POINT ( 'NONE',  ( -59.69999999999998153, -3.031840806488110385, 1.538811659727342906 ) ) ;
#8342 = ORIENTED_EDGE ( 'NONE', *, *, #26310, .T. ) ;
#8344 = DIRECTION ( 'NONE',  ( -3.489354422748178582E-15, 1.218509414717996338E-16, -1.000000000000000000 ) ) ;
#8343 = DIRECTION ( 'NONE',  ( 1.000000000000000000, 0.000000000000000000, -1.047444401652940007E-14 ) ) ;
#8345 = VECTOR ( 'NONE', #26950, 1000.000000000000114 ) ;
#8346 = CARTESIAN_POINT ( 'NONE',  ( 47.05963571244991783, 8.266527678078146479, 1.549999999999835953 ) ) ;
#8347 = ORIENTED_EDGE ( 'NONE', *, *, #3822, .F. ) ;
#8348 = CARTESIAN_POINT ( 'NONE',  ( -77.28999999999996362, -3.470778894058966809E-15, 5.300300110251643219E-15 ) ) ;
#8349 = CARTESIAN_POINT ( 'NONE',  ( 58.75000018595668649, 1.651828233789292222, -1.011330950599448109 ) ) ;
#8350 = CARTESIAN_POINT ( 'NONE',  ( 48.30000000000001847, -0.6304760106459033064, -3.950000000000022826 ) ) ;
#8351 = CARTESIAN_POINT ( 'NONE',  ( -55.88452994616203995, 2.093608279459368564E-14, -3.600000000000198597 ) ) ;
#8353 = VERTEX_POINT ( 'NONE', #14036 ) ;
#8352 = AXIS2_PLACEMENT_3D ( 'NONE', #27725, #6190, #15837 ) ;
#8354 = ADVANCED_FACE ( 'NONE', ( #30984 ), #24112, .T. ) ;
#8355 = CIRCLE ( 'NONE', #26050, 2.824999999999998845 ) ;
#8356 = CARTESIAN_POINT ( 'NONE',  ( 15.41217651307625225, 2.840625797033981215, 4.363718033548180664 ) ) ;
#8357 = CIRCLE ( 'NONE', #8871, 2.625000000001610267 ) ;
#8358 = CARTESIAN_POINT ( 'NONE',  ( 51.80000000000001847, 2.428612866367529932E-14, 0.000000000000000000 ) ) ;
#8359 = CIRCLE ( 'NONE', #24546, 1.975000000000001865 ) ;
#8360 = CARTESIAN_POINT ( 'NONE',  ( -64.29999999999996874, -2.249302195543352312, -0.05603242921607237692 ) ) ;
#8361 = DIRECTION ( 'NONE',  ( -1.000000000000000000, -2.586136946169074517E-16, 0.000000000000000000 ) ) ;
#8362 = CARTESIAN_POINT ( 'NONE',  ( -57.44702994616203284, -2.078460969082625898, -3.600000000000213696 ) ) ;
#8363 = CARTESIAN_POINT ( 'NONE',  ( 58.65263613458533598, -1.873885868624304729, 0.06672978513340610540 ) ) ;
#8364 = CARTESIAN_POINT ( 'NONE',  ( 22.26232992071278005, 7.345532757394721557, 2.049999999999922551 ) ) ;
#8365 = ORIENTED_EDGE ( 'NONE', *, *, #8053, .F. ) ;
#8366 = EDGE_CURVE ( 'NONE', #10836, #23636, #21337, .T. ) ;
#8367 = DIRECTION ( 'NONE',  ( -1.000000000000000000, -3.053848253006669023E-16, 2.042510438544995415E-16 ) ) ;
#8368 = VERTEX_POINT ( 'NONE', #3427 ) ;
#8370 = DIRECTION ( 'NONE',  ( 0.000000000000000000, 0.000000000000000000, 1.000000000000000000 ) ) ;
#8369 = CARTESIAN_POINT ( 'NONE',  ( 48.43418025728714582, 1.399739523915438211, 3.853780793998481169 ) ) ;
#8371 = ORIENTED_EDGE ( 'NONE', *, *, #26125, .F. ) ;
#8372 = CIRCLE ( 'NONE', #22560, 0.09999999999999993616 ) ;
#8373 = ORIENTED_EDGE ( 'NONE', *, *, #7690, .F. ) ;
#8374 = CARTESIAN_POINT ( 'NONE',  ( -59.14405989232412963, -2.099645193746120606E-14, 3.399999999999788969 ) ) ;
#8375 = VECTOR ( 'NONE', #11719, 1000.000000000000000 ) ;
#8376 = CARTESIAN_POINT ( 'NONE',  ( 31.35411506066951404, 7.935106535555555674, 1.424999999999890354 ) ) ;
#8377 = ORIENTED_EDGE ( 'NONE', *, *, #10719, .T. ) ;
#8379 = CARTESIAN_POINT ( 'NONE',  ( 51.86020163181182596, 8.198949176608044453, -1.950000000000180256 ) ) ;
#8378 = CARTESIAN_POINT ( 'NONE',  ( -58.94702994616203284, -2.078460969082631227, -3.600000000000215472 ) ) ;
#8380 = CARTESIAN_POINT ( 'NONE',  ( -58.61042740578358945, -0.7887156198831605236, 3.845940847736174284 ) ) ;
#8381 = AXIS2_PLACEMENT_3D ( 'NONE', #9810, #14854, #5061 ) ;
#8382 = DIRECTION ( 'NONE',  ( 1.000000000000000000, -0.000000000000000000, -1.047444401652940007E-14 ) ) ;
#8383 = APPLICATION_PROTOCOL_DEFINITION ( 'draft international standard', 'automotive_design', 1998, #16079 ) ;
#8384 = AXIS2_PLACEMENT_3D ( 'NONE', #17030, #26509, #12714 ) ;
#8385 = CYLINDRICAL_SURFACE ( 'NONE', #17983, 1.000000000000000000 ) ;
#8386 = MECHANICAL_DESIGN_GEOMETRIC_PRESENTATION_REPRESENTATION (  '', ( #9426 ), #21043 ) ;
#8387 = ORIENTED_EDGE ( 'NONE', *, *, #9373, .F. ) ;
#8388 = EDGE_CURVE ( 'NONE', #23530, #24915, #9922, .T. ) ;
#8389 = AXIS2_PLACEMENT_3D ( 'NONE', #1986, #16084, #11307 ) ;
#8390 = CARTESIAN_POINT ( 'NONE',  ( 47.10000000000002274, -4.179189514726506793, -1.000000000000000000 ) ) ;
#8391 = CARTESIAN_POINT ( 'NONE',  ( 52.05393800078974209, 4.345106731198625560, -2.050000000000180567 ) ) ;
#8392 = CARTESIAN_POINT ( 'NONE',  ( 58.45000000000001705, 0.8000000000000000444, -1.778341924377873751 ) ) ;
#8393 = FACE_OUTER_BOUND ( 'NONE', #20097, .T. ) ;
#8394 = VECTOR ( 'NONE', #20312, 1000.000000000000000 ) ;
#8395 = CARTESIAN_POINT ( 'NONE',  ( -59.69376084107991431, -2.238561451677897551, 1.535209479645327946 ) ) ;
#8396 = VECTOR ( 'NONE', #193, 1000.000000000000227 ) ;
#8398 = CARTESIAN_POINT ( 'NONE',  ( 58.72204580543426289, -1.816949979608304178, -0.4634803957297197186 ) ) ;
#8397 = CARTESIAN_POINT ( 'NONE',  ( 51.45655683570189609, 0.9591657938401613182, 1.611094652690528317 ) ) ;
#8399 = PRESENTATION_LAYER_ASSIGNMENT (  '', '', ( #7908 ) ) ;
#8400 = CARTESIAN_POINT ( 'NONE',  ( -44.59999999999999432, -1.433333333333339343, 4.054078878802691577 ) ) ;
#8401 = CARTESIAN_POINT ( 'NONE',  ( 51.80000000000001137, 3.850000000000016520, -2.050000000000180123 ) ) ;
#8402 = AXIS2_PLACEMENT_3D ( 'NONE', #18660, #11204, #9310 ) ;
#8404 = LINE ( 'NONE', #30398, #8394 ) ;
#8403 = DIRECTION ( 'NONE',  ( 0.000000000000000000, 0.000000000000000000, 1.000000000000000000 ) ) ;
#8405 = EDGE_LOOP ( 'NONE', ( #29740, #28881, #18292, #20486 ) ) ;
#8406 = VECTOR ( 'NONE', #12367, 1000.000000000000000 ) ;
#8407 = ADVANCED_FACE ( 'NONE', ( #14967 ), #14749, .T. ) ;
#8408 =( BOUNDED_SURFACE ( )  B_SPLINE_SURFACE ( 3, 2, ( 
 ( #20561, #6139, #8508 ),
 ( #13384, #18188, #4377 ),
 ( #14027, #26535, #29073 ),
 ( #16894, #11519, #30978 ),
 ( #28772, #14507, #6923 ),
 ( #9296, #23716, #2007 ),
 ( #21196, #16745, #21495 ),
 ( #2158, #24180, #16592 ),
 ( #19283, #26233, #13855 ),
 ( #30826, #26388, #11821 ) ),
 .UNSPECIFIED., .F., .F., .F. ) 
 B_SPLINE_SURFACE_WITH_KNOTS ( ( 4, 2, 2, 2, 4 ),
 ( 3, 3 ),
 ( 0.0002526260074104870901, 0.0003606909493797115550, 0.0004687558913489360741, 0.0006848857752873850581, 0.001117145543164283026 ),
 ( 0.000000000000000000, 1.000000000000000000 ),
 .UNSPECIFIED. ) 
 GEOMETRIC_REPRESENTATION_ITEM ( )  RATIONAL_B_SPLINE_SURFACE ( (
 ( 1.000000000000000000, 0.9842509842511785179, 1.000000000000000000),
 ( 1.000000000000000000, 0.9838268088398964828, 1.000000000000000000),
 ( 1.000000000000000000, 0.9731519947952215199, 1.000000000000000000),
 ( 1.000000000000000000, 0.9499473078865533493, 1.000000000000000000),
 ( 1.000000000000000000, 0.9371632344323698183, 1.000000000000000000),
 ( 1.000000000000000000, 0.8981767195495007350, 1.000000000000000000),
 ( 1.000000000000000000, 0.8714317066438488357, 1.000000000000000000),
 ( 1.000000000000000000, 0.7945716934681560373, 1.000000000000000000),
 ( 1.000000000000000000, 0.7462340517456401701, 1.000000000000000000),
 ( 1.000000000000000000, 0.7071067811865505703, 1.000000000000000000) ) ) 
 REPRESENTATION_ITEM ( '' )  SURFACE ( )  );
#8409 = CARTESIAN_POINT ( 'NONE',  ( 50.36079629521400847, -1.278211010209444387, -3.870212229389975445 ) ) ;
#8410 = CIRCLE ( 'NONE', #14475, 1.625000000000000222 ) ;
#8411 = CARTESIAN_POINT ( 'NONE',  ( -36.79682133506351960, 2.710596767400097473, -4.680923748382986638 ) ) ;
#8413 = CARTESIAN_POINT ( 'NONE',  ( -59.62735476476905205, -2.346806195053343647, -1.237686616523553607 ) ) ;
#8412 = CARTESIAN_POINT ( 'NONE',  ( 58.74999981404330640, 1.909395380152493438, 0.4234853497079917872 ) ) ;
#8414 = CARTESIAN_POINT ( 'NONE',  ( 15.03925126672123369, -5.377732432866647372, 0.5657657256215353758 ) ) ;
#8415 = ORIENTED_EDGE ( 'NONE', *, *, #27305, .T. ) ;
#8416 = CARTESIAN_POINT ( 'NONE',  ( 52.45567523936519905, 8.517307475678896012, 2.049999999999817302 ) ) ;
#8417 = CARTESIAN_POINT ( 'NONE',  ( 47.00000000000002132, -4.131056160354152240, 1.099999999999999867 ) ) ;
#8418 = ORIENTED_EDGE ( 'NONE', *, *, #5617, .T. ) ;
#8419 = AXIS2_PLACEMENT_3D ( 'NONE', #29003, #26469, #17143 ) ;
#8420 = EDGE_CURVE ( 'NONE', #4028, #4358, #24846, .T. ) ;
#8421 = EDGE_LOOP ( 'NONE', ( #13172, #2160, #8919, #666 ) ) ;
#8422 = AXIS2_PLACEMENT_3D ( 'NONE', #26445, #30885, #19020 ) ;
#8423 = FACE_OUTER_BOUND ( 'NONE', #17024, .T. ) ;
#8424 = DIRECTION ( 'NONE',  ( -1.047444401652940007E-14, 0.000000000000000000, -1.000000000000000000 ) ) ;
#8425 = EDGE_LOOP ( 'NONE', ( #16953, #17108, #16825 ) ) ;
#8426 = VECTOR ( 'NONE', #19799, 1000.000000000000000 ) ;
#8427 = CARTESIAN_POINT ( 'NONE',  ( -55.75952994616203995, 3.117691453623995024, -1.800000000000183897 ) ) ;
#8428 = CARTESIAN_POINT ( 'NONE',  ( -59.01905989232412253, -2.944486372867088697, 1.699999999999779243 ) ) ;
#8429 = ORIENTED_EDGE ( 'NONE', *, *, #10188, .T. ) ;
#8430 = CARTESIAN_POINT ( 'NONE',  ( -35.85663232820584057, 4.945493884734801782, -1.606888370749687933 ) ) ;
#8431 = TOROIDAL_SURFACE ( 'NONE', #3379, 1.975000000000001865, 0.1000000000000000056 ) ;
#8432 = ORIENTED_EDGE ( 'NONE', *, *, #261, .F. ) ;
#8433 = CIRCLE ( 'NONE', #5915, 0.01000000000000001929 ) ;
#8434 = CARTESIAN_POINT ( 'NONE',  ( -58.93749999999995737, 1.962990915244749557, -3.400000000000200640 ) ) ;
#8435 = VECTOR ( 'NONE', #4155, 999.9999999999998863 ) ;
#8436 = AXIS2_PLACEMENT_3D ( 'NONE', #1014, #17648, #12865 ) ;
#8437 = ADVANCED_FACE ( 'NONE', ( #12435 ), #7661, .T. ) ;
#8438 = FACE_OUTER_BOUND ( 'NONE', #22028, .T. ) ;
#8439 = DIRECTION ( 'NONE',  ( -1.000000000000000000, 1.219044193948984088E-29, -3.491481338843133750E-15 ) ) ;
#8441 = EDGE_CURVE ( 'NONE', #3969, #6711, #5144, .T. ) ;
#8440 = DIRECTION ( 'NONE',  ( 1.000000000000000000, -0.000000000000000000, -0.000000000000000000 ) ) ;
#8442 = CARTESIAN_POINT ( 'NONE',  ( 47.00000000000002132, 2.428612866367529932E-14, 0.000000000000000000 ) ) ;
#8444 = DIRECTION ( 'NONE',  ( 0.000000000000000000, 0.9996898646859343485, 0.02490330187381130031 ) ) ;
#8443 = FACE_OUTER_BOUND ( 'NONE', #23452, .T. ) ;
#8445 = AXIS2_PLACEMENT_3D ( 'NONE', #20439, #30064, #25327 ) ;
#8446 = CIRCLE ( 'NONE', #6947, 2.000000000000000000 ) ;
#8447 = CYLINDRICAL_SURFACE ( 'NONE', #8893, 2.700000000000000178 ) ;
#8448 = FACE_OUTER_BOUND ( 'NONE', #30940, .T. ) ;
#8449 = FACE_OUTER_BOUND ( 'NONE', #2121, .T. ) ;
#8450 = CARTESIAN_POINT ( 'NONE',  ( -60.49999999999995737, 0.7328781032566589193, -3.573665542649862914 ) ) ;
#8451 = ADVANCED_FACE ( 'NONE', ( #30158 ), #15610, .T. ) ;
#8453 = CARTESIAN_POINT ( 'NONE',  ( 48.37784963381696457, -1.308847734660468332, 3.885629509820973659 ) ) ;
#8452 = VECTOR ( 'NONE', #4279, 1000.000000000000000 ) ;
#8454 = EDGE_LOOP ( 'NONE', ( #18990, #20551, #2866, #434 ) ) ;
#8455 = DIRECTION ( 'NONE',  ( 1.000000000000000000, -0.000000000000000000, 0.000000000000000000 ) ) ;
#8456 = CARTESIAN_POINT ( 'NONE',  ( 68.00000000000001421, 1.401298464324817071E-42, -7.122621931239992550E-13 ) ) ;
#8457 = ORIENTED_EDGE ( 'NONE', *, *, #31125, .T. ) ;
#8458 = AXIS2_PLACEMENT_3D ( 'NONE', #17378, #2523, #26744 ) ;
#8459 = ORIENTED_EDGE ( 'NONE', *, *, #20530, .F. ) ;
#8460 = AXIS2_PLACEMENT_3D ( 'NONE', #1910, #25811, #21086 ) ;
#8461 = TOROIDAL_SURFACE ( 'NONE', #26163, 2.750000000000000000, 0.05000000000000000278 ) ;
#8462 = DIRECTION ( 'NONE',  ( -1.000000000000000000, -3.054025858079668409E-16, 2.042474015755241579E-16 ) ) ;
#8463 = CARTESIAN_POINT ( 'NONE',  ( 61.00000000000001421, 0.8666666666673057406, -1.374595900215365152 ) ) ;
#8465 = CARTESIAN_POINT ( 'NONE',  ( -59.58735571801867792, 2.155141953262397436, 1.555030905555851106 ) ) ;
#8464 = CARTESIAN_POINT ( 'NONE',  ( -57.37499999999996447, 2.944486372867106905, -1.700000000000191136 ) ) ;
#8466 = ORIENTED_EDGE ( 'NONE', *, *, #27419, .T. ) ;
#8467 = ADVANCED_FACE ( 'NONE', ( #23362 ), #22863, .T. ) ;
#8468 = EDGE_LOOP ( 'NONE', ( #19733, #13047, #3038, #20329 ) ) ;
#8469 = CARTESIAN_POINT ( 'NONE',  ( 51.77443163147427896, -4.052038242240612043, -1.950335525115999502 ) ) ;
#8470 = ORIENTED_EDGE ( 'NONE', *, *, #6539, .T. ) ;
#8471 = DIRECTION ( 'NONE',  ( 0.000000000000000000, -1.000000000000000000, 0.000000000000000000 ) ) ;
#8472 = EDGE_LOOP ( 'NONE', ( #11284, #10964, #22415, #27231 ) ) ;
#8473 = CARTESIAN_POINT ( 'NONE',  ( 22.41225425283442618, 6.886225701513755126, -2.050000000000144595 ) ) ;
#8474 = EDGE_CURVE ( 'NONE', #8800, #20516, #16783, .T. ) ;
#8475 = FACE_OUTER_BOUND ( 'NONE', #2929, .T. ) ;
#8476 = CIRCLE ( 'NONE', #10486, 0.2999999999999999334 ) ;
#8477 = CARTESIAN_POINT ( 'NONE',  ( 47.12303005161511038, -3.663337715290890362, 1.844354128036148843 ) ) ;
#8478 = CIRCLE ( 'NONE', #20142, 0.2500000000000000000 ) ;
#8479 = EDGE_CURVE ( 'NONE', #26621, #20326, #14231, .T. ) ;
#8480 = CARTESIAN_POINT ( 'NONE',  ( -60.08155989232412253, 3.925981830489463142, -1.989569613369437003E-13 ) ) ;
#8482 = EDGE_CURVE ( 'NONE', #18265, #22989, #15754, .T. ) ;
#8481 = CARTESIAN_POINT ( 'NONE',  ( 48.00000000000002132, -3.908336260473454615, 1.238913909465752194 ) ) ;
#8483 = CARTESIAN_POINT ( 'NONE',  ( 58.65263613458532888, 1.372222488449602595, 1.277852321299682847 ) ) ;
#8484 = CIRCLE ( 'NONE', #21142, 2.424999999999998934 ) ;
#8485 = CARTESIAN_POINT ( 'NONE',  ( -71.49999999999998579, -1.395601618875910821E-15, 2.917180974979867506E-15 ) ) ;
#8486 = CARTESIAN_POINT ( 'NONE',  ( -35.85663232820584057, 5.086913985776128300, 1.171642053949150331 ) ) ;
#8488 = CYLINDRICAL_SURFACE ( 'NONE', #23012, 0.2500000000000000000 ) ;
#8487 = CARTESIAN_POINT ( 'NONE',  ( 51.12687253673781385, -0.9194130538815391551, 1.491219977510798600 ) ) ;
#8489 = DIRECTION ( 'NONE',  ( 0.000000000000000000, -0.2008964009354147762, 0.9796124928211140670 ) ) ;
#8490 = CARTESIAN_POINT ( 'NONE',  ( -59.03335481156722864, -4.108500314926510022, 1.367561758111408121 ) ) ;
#8491 = CARTESIAN_POINT ( 'NONE',  ( 60.75000000000001421, 0.6500000000006362910, -1.489337100860648189 ) ) ;
#8492 = ORIENTED_EDGE ( 'NONE', *, *, #11720, .T. ) ;
#8493 = AXIS2_PLACEMENT_3D ( 'NONE', #13559, #25593, #18649 ) ;
#8494 = CARTESIAN_POINT ( 'NONE',  ( 54.38981513202823947, 6.361385888908016817, -2.043118470513792140 ) ) ;
#8495 = ORIENTED_EDGE ( 'NONE', *, *, #20452, .T. ) ;
#8496 = CARTESIAN_POINT ( 'NONE',  ( 51.59708304119570954, -3.814011388176574702, 1.508225752246529883 ) ) ;
#8497 = EDGE_LOOP ( 'NONE', ( #19907, #4320, #607, #16893 ) ) ;
#8498 = DIRECTION ( 'NONE',  ( 0.000000000000000000, 0.000000000000000000, 1.000000000000000000 ) ) ;
#8499 = CARTESIAN_POINT ( 'NONE',  ( -57.28335481156723574, 0.8699069336946692044, -4.241846523238430144 ) ) ;
#8501 = CARTESIAN_POINT ( 'NONE',  ( 15.03925126672132784, 4.804073783693426414, 2.042134687550409833 ) ) ;
#8500 = CARTESIAN_POINT ( 'NONE',  ( -35.85663232820584057, 4.018128179617486140, 3.618665901676695995 ) ) ;
#8502 = ORIENTED_EDGE ( 'NONE', *, *, #31055, .T. ) ;
#8503 = EDGE_CURVE ( 'NONE', #26007, #26067, #6151, .T. ) ;
#8504 = CARTESIAN_POINT ( 'NONE',  ( -71.49999999999998579, -1.395601618875910821E-15, 2.917180974979867506E-15 ) ) ;
#8505 = EDGE_CURVE ( 'NONE', #1074, #8907, #10187, .T. ) ;
#8506 = CARTESIAN_POINT ( 'NONE',  ( 57.02075198358709684, -0.7405530952691583568, -1.786721332245943428 ) ) ;
#8507 = ORIENTED_EDGE ( 'NONE', *, *, #2508, .T. ) ;
#8509 = DIRECTION ( 'NONE',  ( -0.9993908270190958731, 0.03489949670250096919, 3.491595022110081325E-15 ) ) ;
#8508 = CARTESIAN_POINT ( 'NONE',  ( 50.29999999999649418, 1.426739617988885822, 3.843749999997122746 ) ) ;
#8510 = EDGE_CURVE ( 'NONE', #17741, #13619, #10842, .T. ) ;
#8511 = CARTESIAN_POINT ( 'NONE',  ( 51.45655683570189609, 0.9591657938401613182, -1.611094652690528317 ) ) ;
#8512 = ORIENTED_EDGE ( 'NONE', *, *, #10626, .T. ) ;
#8513 = CARTESIAN_POINT ( 'NONE',  ( -36.56390771145525775, 5.205077242910716606, -1.471673150993946244 ) ) ;
#8514 = CARTESIAN_POINT ( 'NONE',  ( 58.74999981196283727, 1.734557215429400001, -0.9033020670118147022 ) ) ;
#8515 = PLANE ( 'NONE',  #14960 ) ;
#8516 = DIRECTION ( 'NONE',  ( 0.000000000000000000, -0.9996898646859343485, -0.02490330187381123786 ) ) ;
#8517 = DIRECTION ( 'NONE',  ( 1.000000000000000000, -0.000000000000000000, -1.047444401652940007E-14 ) ) ;
#8518 = AXIS2_PLACEMENT_3D ( 'NONE', #12496, #16957, #24239 ) ;
#8519 = ORIENTED_EDGE ( 'NONE', *, *, #31318, .T. ) ;
#8520 = TOROIDAL_SURFACE ( 'NONE', #14582, 2.750000000000000000, 0.1000000000000000056 ) ;
#8521 = CARTESIAN_POINT ( 'NONE',  ( 15.17256654081426070, -2.686240678228060119, 4.475885392924785933 ) ) ;
#8522 = CARTESIAN_POINT ( 'NONE',  ( -54.67292740578360366, -3.330682475591782765, -0.6830477631804114935 ) ) ;
#8523 = DIRECTION ( 'NONE',  ( 1.000000000000000000, 0.000000000000000000, -0.000000000000000000 ) ) ;
#8524 = CARTESIAN_POINT ( 'NONE',  ( -59.13452994616204705, -3.117691453623983477, 1.799999999999766676 ) ) ;
#8525 = CARTESIAN_POINT ( 'NONE',  ( 58.65000000000004121, -1.872332544500606044, -0.09997921184723318477 ) ) ;
#8526 = CARTESIAN_POINT ( 'NONE',  ( 48.43389689255278796, 1.399562922973069057, -3.853849143137397792 ) ) ;
#8527 = VERTEX_POINT ( 'NONE', #13527 ) ;
#8528 = CARTESIAN_POINT ( 'NONE',  ( 58.74154451056412540, 1.575232816092658972, 1.017012227665773150 ) ) ;
#8529 = VERTEX_POINT ( 'NONE', #20833 ) ;
#8530 = CARTESIAN_POINT ( 'NONE',  ( -59.10189254050602869, 2.466111651538507310, -0.9699939413580190850 ) ) ;
#8532 = DIRECTION ( 'NONE',  ( 2.459562394685743786E-16, -0.9510565162951521989, -0.3090169943749515591 ) ) ;
#8531 = CARTESIAN_POINT ( 'NONE',  ( 58.75000000000000711, 0.8495817349404619634, -1.671477153794393322 ) ) ;
#8533 = VERTEX_POINT ( 'NONE', #3714 ) ;
#8534 = VERTEX_POINT ( 'NONE', #20377 ) ;
#8535 = DIRECTION ( 'NONE',  ( 1.000000000000000000, 2.586136946169074517E-16, -0.000000000000000000 ) ) ;
#8536 = EDGE_CURVE ( 'NONE', #16075, #26071, #4034, .T. ) ;
#8537 = CIRCLE ( 'NONE', #10560, 1.351996603031850208 ) ;
#8538 = CARTESIAN_POINT ( 'NONE',  ( 31.35411506066950693, 7.935106535555555674, -1.425000000000108846 ) ) ;
#8540 = CYLINDRICAL_SURFACE ( 'NONE', #17567, 160.1997717543138720 ) ;
#8539 = CARTESIAN_POINT ( 'NONE',  ( 51.06284382647740472, -4.312058781922653239, -1.282041952414082475 ) ) ;
#8541 = CARTESIAN_POINT ( 'NONE',  ( -56.04792740578360366, -1.073804522883516688, -3.225979517392335794 ) ) ;
#8542 = DIRECTION ( 'NONE',  ( 1.040834085586084257E-14, 0.000000000000000000, 1.000000000000000000 ) ) ;
#8543 = ITEM_DEFINED_TRANSFORMATION ( 'NONE', 'NONE', #16675,  #9018 ) ;
#8544 = CARTESIAN_POINT ( 'NONE',  ( -59.35433616094501730, 2.309227654852833211, 1.299999087803395792 ) ) ;
#8545 = CIRCLE ( 'NONE', #22222, 3.399999999999999911 ) ;
#8546 = VERTEX_POINT ( 'NONE', #6416 ) ;
#8547 = EDGE_CURVE ( 'NONE', #125, #10074, #16078, .T. ) ;
#8548 = DIRECTION ( 'NONE',  ( -1.000000000000000000, 1.219044193948983948E-29, -3.491481338843133355E-15 ) ) ;
#8549 = DIRECTION ( 'NONE',  ( 1.000000000000000000, 2.586136946169074517E-16, -0.000000000000000000 ) ) ;
#8550 = CYLINDRICAL_SURFACE ( 'NONE', #18705, 0.1500000000000001887 ) ;
#8551 = CARTESIAN_POINT ( 'NONE',  ( 15.48609859788809473, -0.1138661108244446996, 5.199999999057606459 ) ) ;
#8552 = AXIS2_PLACEMENT_3D ( 'NONE', #31223, #9549, #29924 ) ;
#8553 = CARTESIAN_POINT ( 'NONE',  ( -54.93749999999998579, 1.962990915244722689, 3.399999999999812506 ) ) ;
#8554 = TOROIDAL_SURFACE ( 'NONE', #24748, 1.975000000000001865, 0.1000000000000000056 ) ;
#8556 = DIRECTION ( 'NONE',  ( 0.000000000000000000, 0.000000000000000000, 1.000000000000000000 ) ) ;
#8555 = CARTESIAN_POINT ( 'NONE',  ( 50.80258015808398397, 5.323456221955952384E-13, -1.996089927833914146 ) ) ;
#8557 = PRODUCT_DEFINITION ( 'UNKNOWN', '', #27800, #14255 ) ;
#8558 = CARTESIAN_POINT ( 'NONE',  ( 52.94597018949752965, 4.198214444775582699, -2.047133864835171124 ) ) ;
#8560 = CARTESIAN_POINT ( 'NONE',  ( 51.80000000000001137, 4.175664755576646847, -1.929721184274108436 ) ) ;
#8559 = DIRECTION ( 'NONE',  ( 2.586136946169074517E-16, -1.000000000000000000, 0.000000000000000000 ) ) ;
#8561 = ORIENTED_EDGE ( 'NONE', *, *, #26244, .F. ) ;
#8562 = CARTESIAN_POINT ( 'NONE',  ( 50.50000000000001421, -0.6462379109120512943, -4.048750000000022276 ) ) ;
#8563 = CARTESIAN_POINT ( 'NONE',  ( 64.99999999999997158, 4.990435706524439459E-16, -4.050000000000681943 ) ) ;
#8565 = CARTESIAN_POINT ( 'NONE',  ( -59.66583922906154669, -2.374710448338320568, -1.229169263546879165 ) ) ;
#8564 = CARTESIAN_POINT ( 'NONE',  ( 58.75000000694004854, 1.856761646088006978, 0.5233439189825915827 ) ) ;
#8566 = CARTESIAN_POINT ( 'NONE',  ( 57.05000000000001137, 0.7500000000000000000, 2.490438859776672231 ) ) ;
#8567 = ORIENTED_EDGE ( 'NONE', *, *, #4072, .F. ) ;
#8568 = CARTESIAN_POINT ( 'NONE',  ( 51.65273894882759009, 3.822289909571943145, 2.049999999999813305 ) ) ;
#8569 = CARTESIAN_POINT ( 'NONE',  ( 24.05318950684998924, 5.396204383593524945, -1.550000000000083533 ) ) ;
#8570 = EDGE_CURVE ( 'NONE', #21265, #9091, #16425, .T. ) ;
#8571 = ORIENTED_EDGE ( 'NONE', *, *, #131, .F. ) ;
#8572 = DIRECTION ( 'NONE',  ( -1.000000000000000000, 0.000000000000000000, 0.000000000000000000 ) ) ;
#8573 = ORIENTED_EDGE ( 'NONE', *, *, #22922, .T. ) ;
#8574 = LINE ( 'NONE', #9084, #12757 ) ;
#8575 = CARTESIAN_POINT ( 'NONE',  ( 68.00000000000000000, -0.7500000000000000000, -1.988246715074070137 ) ) ;
#8576 = EDGE_LOOP ( 'NONE', ( #27039, #26553, #26747, #1964, #9577, #25764 ) ) ;
#8577 = SURFACE_SIDE_STYLE ('',( #4140 ) ) ;
#8578 = CARTESIAN_POINT ( 'NONE',  ( -55.13452994616203995, 2.181782848997977050E-14, -3.600000000000195932 ) ) ;
#8579 = VECTOR ( 'NONE', #29757, 1000.000000000000000 ) ;
#8580 = CARTESIAN_POINT ( 'NONE',  ( -58.51905989232412253, 2.944486372867092250, 1.699999999999803446 ) ) ;
#8581 = AXIS2_PLACEMENT_3D ( 'NONE', #22351, #10301, #7765 ) ;
#8582 = ORIENTED_EDGE ( 'NONE', *, *, #27375, .F. ) ;
#8583 = CARTESIAN_POINT ( 'NONE',  ( 57.04071222441830713, 0.7791709056946051204, -1.732885792771923672 ) ) ;
#8584 = ORIENTED_EDGE ( 'NONE', *, *, #1261, .F. ) ;
#8585 = ORIENTED_EDGE ( 'NONE', *, *, #23175, .T. ) ;
#8586 = AXIS2_PLACEMENT_3D ( 'NONE', #27788, #8471, #12587 ) ;
#8587 = EDGE_CURVE ( 'NONE', #36, #30639, #17603, .T. ) ;
#8588 = CARTESIAN_POINT ( 'NONE',  ( -55.37499999999996447, -2.944486372867076707, -1.700000000000207345 ) ) ;
#8589 = CARTESIAN_POINT ( 'NONE',  ( 60.87107532335745930, 0.5000002988029885742, 1.554802360349133661 ) ) ;
#8590 = CARTESIAN_POINT ( 'NONE',  ( 25.48092967892657512, 5.262749364038175059, -1.425000000000088862 ) ) ;
#8591 = DIRECTION ( 'NONE',  ( -0.8262273428075540549, 0.5633368246415005887, 0.000000000000000000 ) ) ;
#8592 = CARTESIAN_POINT ( 'NONE',  ( -60.64999999999998437, 2.699162634652024551, 0.06723891505929238677 ) ) ;
#8593 =( BOUNDED_SURFACE ( )  B_SPLINE_SURFACE ( 3, 2, ( 
 ( #15143, #16798, #28826 ),
 ( #19905, #21871, #24943 ),
 ( #2542, #26593, #12192 ),
 ( #7847, #576, #26290 ) ),
 .UNSPECIFIED., .F., .F., .F. ) 
 B_SPLINE_SURFACE_WITH_KNOTS ( ( 4, 4 ),
 ( 3, 3 ),
 ( 5.086771802766119954, 5.213876728150149020 ),
 ( 0.000000000000000000, 1.000000000000000000 ),
 .UNSPECIFIED. ) 
 GEOMETRIC_REPRESENTATION_ITEM ( )  RATIONAL_B_SPLINE_SURFACE ( (
 ( 1.000000000000000000, 0.8113889037030935780, 1.000000000000000000),
 ( 1.000000000000000000, 0.8219112105083469233, 1.000000000000000000),
 ( 1.000000000000000000, 0.8319656872388402347, 1.000000000000000000),
 ( 1.000000000000000000, 0.8415238966082420058, 1.000000000000000000) ) ) 
 REPRESENTATION_ITEM ( '' )  SURFACE ( )  );
#8594 = CIRCLE ( 'NONE', #24784, 4.000000000000022204 ) ;
#8596 = DIRECTION ( 'NONE',  ( -2.117927888850090838E-16, 0.02490330187381123786, -0.9996898646859343485 ) ) ;
#8595 = FACE_OUTER_BOUND ( 'NONE', #14161, .T. ) ;
#8597 = B_SPLINE_CURVE_WITH_KNOTS ( 'NONE', 3,
 ( #25230, #3075, #10524, #20348, #10348, #27448 ),
 .UNSPECIFIED., .F., .F.,
 ( 4, 2, 4 ),
 ( 0.0002203024014533751739, 0.0003053046653303950015, 0.0003903069292074148834 ),
 .UNSPECIFIED. ) ;
#8598 = SURFACE_STYLE_USAGE ( .BOTH. , #30287 ) ;
#8599 = DIRECTION ( 'NONE',  ( 0.000000000000000000, 0.000000000000000000, -1.000000000000000000 ) ) ;
#8600 = CARTESIAN_POINT ( 'NONE',  ( 51.25000000000001421, 5.368159983410797313E-13, 3.111507638930570854E-58 ) ) ;
#8601 = CARTESIAN_POINT ( 'NONE',  ( 58.66118217212494557, -1.632243256842334844, -0.9228675180752388130 ) ) ;
#8602 = CARTESIAN_POINT ( 'NONE',  ( 53.86856682907188798, 7.562246134602117920, -2.050000000000188116 ) ) ;
#8603 = FACE_OUTER_BOUND ( 'NONE', #15956, .T. ) ;
#8604 = ORIENTED_EDGE ( 'NONE', *, *, #5524, .F. ) ;
#8605 = CYLINDRICAL_SURFACE ( 'NONE', #29276, 0.2500000000000002220 ) ;
#8606 = AXIS2_PLACEMENT_3D ( 'NONE', #28088, #6411, #5783 ) ;
#8607 = ADVANCED_FACE ( 'NONE', ( #21635 ), #11790, .F. ) ;
#8608 = ORIENTED_EDGE ( 'NONE', *, *, #4741, .F. ) ;
#8609 = CARTESIAN_POINT ( 'NONE',  ( 34.56269065792915995, 8.313757757582562746, -2.050000000000119726 ) ) ;
#8611 = CARTESIAN_POINT ( 'NONE',  ( 47.00000000000002842, -3.995259070520241540, 2.068697874511656654 ) ) ;
#8610 = CARTESIAN_POINT ( 'NONE',  ( -55.68749999999999289, 1.962990915244722689, 3.399999999999809841 ) ) ;
#8612 = ADVANCED_FACE ( 'NONE', ( #14163 ), #4342, .F. ) ;
#8613 = ORIENTED_EDGE ( 'NONE', *, *, #2052, .T. ) ;
#8614 = ORIENTED_EDGE ( 'NONE', *, *, #31068, .T. ) ;
#8615 = FACE_OUTER_BOUND ( 'NONE', #12213, .T. ) ;
#8616 = ORIENTED_EDGE ( 'NONE', *, *, #8148, .F. ) ;
#8617 = CARTESIAN_POINT ( 'NONE',  ( 58.65838214097809811, -1.606847897767968547, 0.9664062014974877934 ) ) ;
#8618 = VERTEX_POINT ( 'NONE', #9425 ) ;
#8619 = CARTESIAN_POINT ( 'NONE',  ( 22.61091062455492562, 6.637672123835907101, -1.950000000000045253 ) ) ;
#8620 = CARTESIAN_POINT ( 'NONE',  ( -61.58692253671846828, -2.617039774925715268, 0.3716872663236084340 ) ) ;
#8621 = CARTESIAN_POINT ( 'NONE',  ( -54.49999999999997158, -3.430639028629426601, -0.8101486624347474796 ) ) ;
#8622 = ORIENTED_EDGE ( 'NONE', *, *, #21117, .F. ) ;
#8623 = EDGE_CURVE ( 'NONE', #27956, #30697, #7676, .T. ) ;
#8624 = CARTESIAN_POINT ( 'NONE',  ( 46.99358615024069508, -4.235076411888983650, -1.097987773005456580 ) ) ;
#8625 = CARTESIAN_POINT ( 'NONE',  ( -62.09999999999997300, -2.738044307818161549, 0.2465463003561280952 ) ) ;
#8626 = CARTESIAN_POINT ( 'NONE',  ( 51.18285175554922972, -0.9660043368199603409, 1.457922727165797294 ) ) ;
#8627 = CARTESIAN_POINT ( 'NONE',  ( 51.31572262954152563, 1.002608958138273554, 1.584424273060082378 ) ) ;
#8628 = CARTESIAN_POINT ( 'NONE',  ( 58.75000000000000711, 1.320165430233467552, 1.457266603154374618 ) ) ;
#8629 = TOROIDAL_SURFACE ( 'NONE', #19774, 3.524999999999996358, 0.1000000000000000056 ) ;
#8630 = CARTESIAN_POINT ( 'NONE',  ( 57.04306286658350444, 0.7495164233357125561, -1.778776689171566172 ) ) ;
#8632 = DIRECTION ( 'NONE',  ( 0.000000000000000000, -4.336808689942024836E-15, 1.000000000000000000 ) ) ;
#8631 = CARTESIAN_POINT ( 'NONE',  ( -61.10430241999939938, -2.596047117859637154, 0.7520320166841959475 ) ) ;
#8633 = EDGE_CURVE ( 'NONE', #17058, #11190, #11729, .T. ) ;
#8634 = CARTESIAN_POINT ( 'NONE',  ( 57.00000000000001421, 0.7500000000000000000, 3.499999999999999556 ) ) ;
#8635 = FACE_OUTER_BOUND ( 'NONE', #3353, .T. ) ;
#8636 = DIRECTION ( 'NONE',  ( 0.000000000000000000, -0.9996898646859344595, -0.02490330187381124480 ) ) ;
#8637 = EDGE_LOOP ( 'NONE', ( #27854, #16216, #9992, #1029 ) ) ;
#8638 = DIRECTION ( 'NONE',  ( 0.000000000000000000, 0.000000000000000000, -1.000000000000000000 ) ) ;
#8639 = ORIENTED_EDGE ( 'NONE', *, *, #11931, .T. ) ;
#8640 = EDGE_CURVE ( 'NONE', #10683, #3969, #23837, .T. ) ;
#8641 = CARTESIAN_POINT ( 'NONE',  ( 50.80000000000002558, -4.031600731908414836, 1.173113608511496597 ) ) ;
#8642 = ORIENTED_EDGE ( 'NONE', *, *, #7085, .F. ) ;
#8643 = EDGE_CURVE ( 'NONE', #4204, #17696, #13821, .T. ) ;
#8644 = CARTESIAN_POINT ( 'NONE',  ( 52.91918222397609384, 8.304852724747799897, 1.919164453910085610 ) ) ;
#8645 = CARTESIAN_POINT ( 'NONE',  ( -57.72085481156722864, 1.184343223768590914, 3.558065644182727194 ) ) ;
#8647 = CARTESIAN_POINT ( 'NONE',  ( 51.80000000000001137, -3.550773357292064780, -2.049880134336005799 ) ) ;
#8646 = DIRECTION ( 'NONE',  ( 3.002035892788116966E-16, -0.9996898646859343485, -0.02490330187381123786 ) ) ;
#8648 = EDGE_CURVE ( 'NONE', #22384, #9517, #26399, .T. ) ;
#8649 = VERTEX_POINT ( 'NONE', #9267 ) ;
#8650 = ORIENTED_EDGE ( 'NONE', *, *, #10469, .T. ) ;
#8651 = CARTESIAN_POINT ( 'NONE',  ( 27.81714062797481191, 5.541011620835246454, -2.050000000000097522 ) ) ;
#8652 = DIRECTION ( 'NONE',  ( 0.000000000000000000, -1.000000000000000000, -4.336808689942015369E-15 ) ) ;
#8653 = ORIENTED_EDGE ( 'NONE', *, *, #1134, .F. ) ;
#8655 = LINE ( 'NONE', #10873, #7952 ) ;
#8654 = PLANE ( 'NONE',  #17609 ) ;
#8656 = CARTESIAN_POINT ( 'NONE',  ( -56.01905989232412963, -2.944486372867090918, 1.699999999999787015 ) ) ;
#8657 = ORIENTED_EDGE ( 'NONE', *, *, #16190, .T. ) ;
#8658 = CARTESIAN_POINT ( 'NONE',  ( -36.56242893520593640, 5.074157625981714048, -1.874066637979897143 ) ) ;
#8659 = B_SPLINE_CURVE_WITH_KNOTS ( 'NONE', 3,
 ( #19607, #9772, #7394, #23878, #28620, #17073, #16602, #26725, #26245 ),
 .UNSPECIFIED., .F., .F.,
 ( 4, 1, 1, 1, 1, 1, 4 ),
 ( 0.000000000000000000, 0.08990530927501938496, 0.2069505209790863942, 0.2957249676700259844, 0.5865340158044511920, 0.7553074047937105018, 0.9685669348269267953 ),
 .UNSPECIFIED. ) ;
#8660 = CARTESIAN_POINT ( 'NONE',  ( 58.75000018595668649, 1.857295262527451696, -0.5493460779666961002 ) ) ;
#8661 = DIRECTION ( 'NONE',  ( -1.000000000000000000, -3.053848253006669023E-16, 2.042510438544995415E-16 ) ) ;
#8662 = CARTESIAN_POINT ( 'NONE',  ( -54.69702994616206837, -2.078460969082657872, 3.599999999999797584 ) ) ;
#8663 = VECTOR ( 'NONE', #8766, 1000.000000000000000 ) ;
#8664 = CARTESIAN_POINT ( 'NONE',  ( -59.29999999999997584, 2.330309927981285032E-15, 4.253626757584724400E-16 ) ) ;
#8665 = ADVANCED_FACE ( 'NONE', ( #16716 ), #18930, .T. ) ;
#8666 = CARTESIAN_POINT ( 'NONE',  ( -58.17292740578360366, 2.256877952708275181, -2.542931754211918971 ) ) ;
#8668 = EDGE_CURVE ( 'NONE', #8968, #9407, #10206, .T. ) ;
#8667 = CARTESIAN_POINT ( 'NONE',  ( 58.75000000000001421, 0.5000000000004131140, 1.863080903344439321 ) ) ;
#8669 = CARTESIAN_POINT ( 'NONE',  ( 61.00000000000002842, -0.8112099027092640746, -1.409560742431901437 ) ) ;
#8670 = CARTESIAN_POINT ( 'NONE',  ( 58.50000000000001421, 0.8000000000000000444, 2.471260002560649927 ) ) ;
#8671 = ORIENTED_EDGE ( 'NONE', *, *, #24321, .T. ) ;
#8672 = CIRCLE ( 'NONE', #3130, 0.09999999999999982514 ) ;
#8673 = DIRECTION ( 'NONE',  ( 1.000000000000000000, -0.000000000000000000, -1.047444401652940007E-14 ) ) ;
#8674 = ORIENTED_EDGE ( 'NONE', *, *, #2101, .F. ) ;
#8675 = CARTESIAN_POINT ( 'NONE',  ( -73.89999999999997726, 0.7497673985144486242, 0.01867747640536001827 ) ) ;
#8677 = DIRECTION ( 'NONE',  ( -0.9977167620779625601, -0.06753712067201329827, 0.000000000000000000 ) ) ;
#8676 = CARTESIAN_POINT ( 'NONE',  ( 48.42250533816334013, 1.328329461116622090, 3.879000873601222477 ) ) ;
#8678 = ORIENTED_EDGE ( 'NONE', *, *, #13910, .T. ) ;
#8679 = EDGE_LOOP ( 'NONE', ( #12304, #2976, #244, #8584 ) ) ;
#8680 = DIRECTION ( 'NONE',  ( -1.000000000000000000, -5.172273892338149033E-16, 0.000000000000000000 ) ) ;
#8681 = AXIS2_PLACEMENT_3D ( 'NONE', #28490, #23430, #16147 ) ;
#8682 = AXIS2_PLACEMENT_3D ( 'NONE', #2282, #11948, #28742 ) ;
#8683 = CARTESIAN_POINT ( 'NONE',  ( 29.29107486424064177, 6.659593085418572755, -1.425000000000101963 ) ) ;
#8684 = CARTESIAN_POINT ( 'NONE',  ( 61.25000000000004263, -1.470078920827889268, 1.470078920827824209 ) ) ;
#8685 = ORIENTED_EDGE ( 'NONE', *, *, #14452, .T. ) ;
#8686 = CARTESIAN_POINT ( 'NONE',  ( -57.79792740578359656, -2.256877952708263635, 2.542931754211924744 ) ) ;
#8687 = CARTESIAN_POINT ( 'NONE',  ( 58.45000000000001705, 0.8000000000000001554, 1.778341924377873973 ) ) ;
#8688 = APPLICATION_PROTOCOL_DEFINITION ( 'draft international standard', 'automotive_design', 1998, #26389 ) ;
#8689 = CARTESIAN_POINT ( 'NONE',  ( -59.40397935374117111, 2.384164297664157495, 1.250136525132547805 ) ) ;
#8690 = ORIENTED_EDGE ( 'NONE', *, *, #30295, .F. ) ;
#8691 = CARTESIAN_POINT ( 'NONE',  ( 41.48619405471883681, -151.3359592902621955, -2.050000000000163691 ) ) ;
#8692 = ORIENTED_EDGE ( 'NONE', *, *, #1811, .F. ) ;
#8693 = CARTESIAN_POINT ( 'NONE',  ( 61.24796382359978253, 0.9549219522845532326, -1.676592304036239378 ) ) ;
#8694 = DIRECTION ( 'NONE',  ( 0.000000000000000000, 1.000000000000000000, 0.000000000000000000 ) ) ;
#8695 = FACE_OUTER_BOUND ( 'NONE', #18389, .T. ) ;
#8696 = EDGE_CURVE ( 'NONE', #10424, #9403, #1605, .T. ) ;
#8697 = EDGE_CURVE ( 'NONE', #22982, #8368, #12729, .T. ) ;
#8698 = DIRECTION ( 'NONE',  ( 3.083952846180964840E-15, 0.000000000000000000, 1.000000000000000000 ) ) ;
#8701 = ADVANCED_FACE ( 'NONE', ( #23506 ), #1803, .T. ) ;
#8700 = DIRECTION ( 'NONE',  ( -0.000000000000000000, 1.000000000000000000, 1.532429380227459806E-15 ) ) ;
#8699 = CARTESIAN_POINT ( 'NONE',  ( 51.84772254680354564, -0.6924618999061495916, 1.653428777428161078 ) ) ;
#8702 = CARTESIAN_POINT ( 'NONE',  ( 52.43766309949614168, 4.002594832745192122, -2.045777940973402043 ) ) ;
#8704 = CARTESIAN_POINT ( 'NONE',  ( -54.50000000000000000, 3.067956443743977690, -1.885759217255443376 ) ) ;
#8703 = DIRECTION ( 'NONE',  ( 1.000000000000000000, 0.000000000000000000, -3.491481338843133355E-15 ) ) ;
#8705 = ORIENTED_EDGE ( 'NONE', *, *, #13622, .T. ) ;
#8706 = FACE_OUTER_BOUND ( 'NONE', #13374, .T. ) ;
#8707 = LINE ( 'NONE', #18392, #19413 ) ;
#8708 = VECTOR ( 'NONE', #30101, 1000.000000000000114 ) ;
#8710 = CARTESIAN_POINT ( 'NONE',  ( 47.02562379653426206, -3.759602463706844144, -1.865002073832594975 ) ) ;
#8709 = DIRECTION ( 'NONE',  ( 0.000000000000000000, 0.000000000000000000, -1.000000000000000000 ) ) ;
#8711 = PLANE ( 'NONE',  #6450 ) ;
#8712 = ORIENTED_EDGE ( 'NONE', *, *, #19425, .T. ) ;
#8713 = CARTESIAN_POINT ( 'NONE',  ( 53.31748909063355768, 8.199041228893841904, 2.049999999999814193 ) ) ;
#8714 = DIRECTION ( 'NONE',  ( 0.000000000000000000, -1.000000000000000000, -1.532429380227459806E-15 ) ) ;
#8715 = EDGE_CURVE ( 'NONE', #4862, #16826, #18773, .T. ) ;
#8716 = ORIENTED_EDGE ( 'NONE', *, *, #14220, .F. ) ;
#8717 = DIRECTION ( 'NONE',  ( 0.000000000000000000, 1.000000000000000000, -8.673617379884030739E-15 ) ) ;
#8718 = ORIENTED_EDGE ( 'NONE', *, *, #147, .T. ) ;
#8719 = CARTESIAN_POINT ( 'NONE',  ( 16.08093158123429234, 3.408535483610603656, -4.200031884472213761 ) ) ;
#8720 = CARTESIAN_POINT ( 'NONE',  ( 47.12198605825954445, -4.132863666287243554, -2.022846738277279233 ) ) ;
#8721 = ORIENTED_EDGE ( 'NONE', *, *, #13093, .T. ) ;
#8722 = CARTESIAN_POINT ( 'NONE',  ( -54.57202994616206126, -4.156921938165296204, -2.089175772356712318E-13 ) ) ;
#8723 = CARTESIAN_POINT ( 'NONE',  ( -57.83155989232412253, 3.925981830489463142, -1.911011283245466534E-13 ) ) ;
#8724 = ORIENTED_EDGE ( 'NONE', *, *, #27305, .F. ) ;
#8725 = DIRECTION ( 'NONE',  ( 1.000000000000000000, 3.054025858079668409E-16, -2.042474015755241579E-16 ) ) ;
#8726 = ORIENTED_EDGE ( 'NONE', *, *, #25114, .T. ) ;
#8727 = ORIENTED_EDGE ( 'NONE', *, *, #3174, .F. ) ;
#8728 = CARTESIAN_POINT ( 'NONE',  ( -56.81249999999997158, -1.962990915244707368, -3.400000000000208633 ) ) ;
#8729 =( BOUNDED_SURFACE ( )  B_SPLINE_SURFACE ( 3, 2, ( 
 ( #2515, #29099, #7413 ),
 ( #7109, #278, #19158 ),
 ( #27018, #31160, #24038 ),
 ( #14690, #29259, #26738 ),
 ( #14831, #5032, #2347 ),
 ( #5327, #14990, #2180 ),
 ( #24350, #4874, #2663 ),
 ( #21695, #7250, #21984 ),
 ( #9945, #9495, #28797 ),
 ( #16769, #12013, #28942 ),
 ( #16918, #26561, #14539 ),
 ( #19621, #24204, #30018 ),
 ( #25281, #20243, #12766 ),
 ( #8334, #27491, #18008 ),
 ( #739, #27657, #6130 ),
 ( #8187, #17700, #5985 ) ),
 .UNSPECIFIED., .F., .F., .F. ) 
 B_SPLINE_SURFACE_WITH_KNOTS ( ( 4, 2, 2, 2, 2, 2, 2, 4 ),
 ( 3, 3 ),
 ( 0.001780502285214203163, 0.002558945925323785446, 0.002753556835351180909, 0.002948167745378576371, 0.003337389565433367296, 0.003726611385488158654, 0.004115833205542950013, 0.004894276845652531863 ),
 ( 0.000000000000000000, 1.000000000000000000 ),
 .UNSPECIFIED. ) 
 GEOMETRIC_REPRESENTATION_ITEM ( )  RATIONAL_B_SPLINE_SURFACE ( (
 ( 1.000000000000000000, 0.9418517008537237167, 1.000000000000000000),
 ( 1.000000000000000000, 0.9417987965885079582, 1.000000000000000000),
 ( 1.000000000000000000, 0.9418198861734077276, 1.000000000000000000),
 ( 1.000000000000000000, 0.9434060303845566153, 1.000000000000000000),
 ( 1.000000000000000000, 0.9437939819948232278, 1.000000000000000000),
 ( 1.000000000000000000, 0.9445989566712728047, 1.000000000000000000),
 ( 1.000000000000000000, 0.9450169930049754363, 1.000000000000000000),
 ( 1.000000000000000000, 0.9461610507673754444, 1.000000000000000000),
 ( 1.000000000000000000, 0.9467217966427202702, 1.000000000000000000),
 ( 1.000000000000000000, 0.9467345476124352510, 1.000000000000000000),
 ( 1.000000000000000000, 0.9461964028052860520, 1.000000000000000000),
 ( 1.000000000000000000, 0.9446801822473911425, 1.000000000000000000),
 ( 1.000000000000000000, 0.9437582546536744665, 1.000000000000000000),
 ( 1.000000000000000000, 0.9418129560295230851, 1.000000000000000000),
 ( 1.000000000000000000, 0.9418016889777798273, 1.000000000000000000),
 ( 1.000000000000000000, 0.9418517008537228286, 1.000000000000000000) ) ) 
 REPRESENTATION_ITEM ( '' )  SURFACE ( )  );
#8730 = CARTESIAN_POINT ( 'NONE',  ( 61.02723049001765077, 0.5636288612511761720, 1.705074539937785572 ) ) ;
#8731 = CARTESIAN_POINT ( 'NONE',  ( 22.44093457455321783, 6.836382162713701582, -1.425000000000078426 ) ) ;
#8732 = CIRCLE ( 'NONE', #7240, 30.00000000000000000 ) ;
#8733 = LINE ( 'NONE', #25692, #9423 ) ;
#8734 = FACE_OUTER_BOUND ( 'NONE', #22474, .T. ) ;
#8735 = EDGE_CURVE ( 'NONE', #15593, #616, #1978, .T. ) ;
#8737 = CARTESIAN_POINT ( 'NONE',  ( 51.70000000000002416, 6.982261990806648555E-14, -1.793082891011605378E-13 ) ) ;
#8736 = DIRECTION ( 'NONE',  ( 0.000000000000000000, 0.000000000000000000, 1.000000000000000000 ) ) ;
#8738 = DIRECTION ( 'NONE',  ( 0.000000000000000000, 0.000000000000000000, 1.000000000000000000 ) ) ;
#8739 = CARTESIAN_POINT ( 'NONE',  ( -71.44781903063172024, -0.2962147058074217632, 1.444404304980893006 ) ) ;
#8740 = CARTESIAN_POINT ( 'NONE',  ( 53.94245690748189048, 6.674762429336749570, 1.915449902665258275 ) ) ;
#8741 = DIRECTION ( 'NONE',  ( 0.000000000000000000, -1.000000000000000000, -1.224646799147352961E-16 ) ) ;
#8742 = ORIENTED_EDGE ( 'NONE', *, *, #16715, .F. ) ;
#8743 = DIRECTION ( 'NONE',  ( 0.9993908270191184107, -0.03489949670185085034, -3.491481338843133355E-15 ) ) ;
#8744 =( LENGTH_UNIT ( ) NAMED_UNIT ( * ) SI_UNIT ( .MILLI., .METRE. ) );
#8745 = ADVANCED_FACE ( 'NONE', ( #28573 ), #7919, .T. ) ;
#8746 = VERTEX_POINT ( 'NONE', #17321 ) ;
#8747 =( NAMED_UNIT ( * ) SI_UNIT ( $, .STERADIAN. ) SOLID_ANGLE_UNIT ( ) );
#8748 = AXIS2_PLACEMENT_3D ( 'NONE', #11693, #21373, #14536 ) ;
#8749 = DIRECTION ( 'NONE',  ( 1.000000000000000000, 0.000000000000000000, 0.000000000000000000 ) ) ;
#8751 = CARTESIAN_POINT ( 'NONE',  ( 50.25000000000004263, -1.895722432253035050, 0.6373668173470157239 ) ) ;
#8750 = CARTESIAN_POINT ( 'NONE',  ( -55.18749999999996447, 1.962990915244749557, -3.400000000000187317 ) ) ;
#8752 = ORIENTED_EDGE ( 'NONE', *, *, #1858, .T. ) ;
#8753 = AXIS2_PLACEMENT_3D ( 'NONE', #17921, #5890, #9207 ) ;
#8754 = VERTEX_POINT ( 'NONE', #7518 ) ;
#8755 = DIRECTION ( 'NONE',  ( 1.000000000000000000, 1.047444401652940007E-14, 0.000000000000000000 ) ) ;
#8756 = ORIENTED_EDGE ( 'NONE', *, *, #17396, .T. ) ;
#8757 = CARTESIAN_POINT ( 'NONE',  ( 58.75000000694009827, -1.682988785000789855, 0.9428687169914291566 ) ) ;
#8758 = DIRECTION ( 'NONE',  ( 0.000000000000000000, 0.2008964009354148039, -0.9796124928211140670 ) ) ;
#8759 = ORIENTED_EDGE ( 'NONE', *, *, #17518, .F. ) ;
#8760 = CARTESIAN_POINT ( 'NONE',  ( 23.07431837909838634, 6.199584074734630690, -1.950000000000079670 ) ) ;
#8761 = DIRECTION ( 'NONE',  ( 1.000000000000000000, 0.000000000000000000, 0.000000000000000000 ) ) ;
#8762 = B_SPLINE_CURVE_WITH_KNOTS ( 'NONE', 3,
 ( #12826, #20155, #22508, #27255, #15541, #19830, #503, #29459, #7774, #10309, #29784, #8099, #8247 ),
 .UNSPECIFIED., .F., .F.,
 ( 4, 3, 3, 3, 4 ),
 ( 8.131516293641283255E-20, 1.679636492926620125E-05, 3.358850293755425803E-05, 5.044195101993695514E-05, 6.090334109303062704E-05 ),
 .UNSPECIFIED. ) ;
#8763 = DIRECTION ( 'NONE',  ( 0.000000000000000000, -0.000000000000000000, 1.000000000000000000 ) ) ;
#8764 = ORIENTED_EDGE ( 'NONE', *, *, #5206, .F. ) ;
#8765 =( BOUNDED_CURVE ( )  B_SPLINE_CURVE ( 3, ( #11449, #16049, #1953, #11278 ),
 .UNSPECIFIED., .F., .T. ) 
 B_SPLINE_CURVE_WITH_KNOTS ( ( 4, 4 ),
 ( 0.8682581838661508344, 1.057606415020297064 ),
 .UNSPECIFIED. ) 
 CURVE ( )  GEOMETRIC_REPRESENTATION_ITEM ( )  RATIONAL_B_SPLINE_CURVE ( ( 1.000000000000000000, 0.9970145015783106190, 0.9970145015783106190, 1.000000000000000000 ) ) 
 REPRESENTATION_ITEM ( '' )  );
#8766 = DIRECTION ( 'NONE',  ( -3.491481338843133355E-15, -3.491481338843133355E-15, 1.000000000000000000 ) ) ;
#8767 = CARTESIAN_POINT ( 'NONE',  ( 36.50000000000002132, 0.7794871794871797155, -1.732743413496390161 ) ) ;
#8768 = CARTESIAN_POINT ( 'NONE',  ( 69.20000000000005969, 0.7500000000000000000, 1.988246715072633952 ) ) ;
#8769 = CARTESIAN_POINT ( 'NONE',  ( -73.89999999999997726, -2.435524336289708093E-15, 4.607889071584891164E-15 ) ) ;
#8770 = CARTESIAN_POINT ( 'NONE',  ( 58.75000000694006275, 1.346330794793899166, 1.381609951798974834 ) ) ;
#8771 = ADVANCED_FACE ( 'NONE', ( #10513 ), #20189, .T. ) ;
#8772 = DIRECTION ( 'NONE',  ( -0.9993908270190957621, 0.03489949670250100389, 3.492120980335537899E-15 ) ) ;
#8773 = DIRECTION ( 'NONE',  ( 0.000000000000000000, 0.9985773570673163180, 0.05332224631852457153 ) ) ;
#8775 = CARTESIAN_POINT ( 'NONE',  ( 51.77496349830696687, -4.051364836626919264, 1.951815467915475777 ) ) ;
#8774 = CARTESIAN_POINT ( 'NONE',  ( -61.11832338958137711, -2.528658595614148741, 0.7486059352628685604 ) ) ;
#8776 = AXIS2_PLACEMENT_3D ( 'NONE', #24083, #14262, #7460 ) ;
#8777 = EDGE_CURVE ( 'NONE', #7978, #4176, #14508, .T. ) ;
#8778 = CARTESIAN_POINT ( 'NONE',  ( 58.65000000000003411, -1.022750809560422747, 1.571497941946552457 ) ) ;
#8779 = CARTESIAN_POINT ( 'NONE',  ( -59.15835481156722864, -0.7533615035078041755, 3.673546848079178861 ) ) ;
#8780 = DIRECTION ( 'NONE',  ( -1.000000000000000000, -0.000000000000000000, 3.491481338843133355E-15 ) ) ;
#8781 = VERTEX_POINT ( 'NONE', #4980 ) ;
#8782 = CIRCLE ( 'NONE', #20950, 0.1500000000000000777 ) ;
#8783 = ORIENTED_EDGE ( 'NONE', *, *, #12718, .F. ) ;
#8784 = EDGE_CURVE ( 'NONE', #14413, #16551, #2463, .T. ) ;
#8785 = CARTESIAN_POINT ( 'NONE',  ( 51.70000000000003126, -3.550773357292059007, 2.049880134335641202 ) ) ;
#8786 = VERTEX_POINT ( 'NONE', #12710 ) ;
#8787 = CARTESIAN_POINT ( 'NONE',  ( 52.11477178369204921, 3.843881278534198476, 2.049999999999818190 ) ) ;
#8788 = CARTESIAN_POINT ( 'NONE',  ( -58.28335481156722864, -4.108500314926510022, 1.367561758111407677 ) ) ;
#8790 = CARTESIAN_POINT ( 'NONE',  ( -62.29999999999998295, 2.749147127886321318, 0.06848408015298348972 ) ) ;
#8789 = CARTESIAN_POINT ( 'NONE',  ( 51.80000000000001847, 2.478823385132571406E-14, 4.100000000000022737 ) ) ;
#8791 = ORIENTED_EDGE ( 'NONE', *, *, #3790, .F. ) ;
#8792 = DIRECTION ( 'NONE',  ( 0.000000000000000000, 0.000000000000000000, -1.000000000000000000 ) ) ;
#8793 = VECTOR ( 'NONE', #30033, 1000.000000000000000 ) ;
#8794 = DIRECTION ( 'NONE',  ( -1.000000000000000000, -3.053848253006669023E-16, 2.042510438544995415E-16 ) ) ;
#8795 = ORIENTED_EDGE ( 'NONE', *, *, #12665, .T. ) ;
#8796 = B_SPLINE_CURVE_WITH_KNOTS ( 'NONE', 3,
 ( #29688, #10542, #22890, #1038, #3420, #12888, #17828, #17671, #29846, #5951 ),
 .UNSPECIFIED., .F., .F.,
 ( 4, 2, 2, 2, 4 ),
 ( 0.000000000000000000, 3.859340476725683618E-05, 7.718680953451367236E-05, 0.0001543736190690279410, 0.0003087472381380618452 ),
 .UNSPECIFIED. ) ;
#8798 = PLANE ( 'NONE',  #11005 ) ;
#8797 = DIRECTION ( 'NONE',  ( 1.000000000000000000, 3.053848253006669023E-16, -2.042510438544995415E-16 ) ) ;
#8799 = DIRECTION ( 'NONE',  ( 1.000000000000000000, 1.047444401652940007E-14, 0.000000000000000000 ) ) ;
#8800 = VERTEX_POINT ( 'NONE', #24441 ) ;
#8801 = AXIS2_PLACEMENT_3D ( 'NONE', #25628, #16299, #4246 ) ;
#8802 = CARTESIAN_POINT ( 'NONE',  ( -36.38139716712170468, 5.370189181195062389, -0.6649548426257293476 ) ) ;
#8803 = ADVANCED_FACE ( 'NONE', ( #26965, #22089 ), #681, .T. ) ;
#8804 = PLANE ( 'NONE',  #18834 ) ;
#8805 = CYLINDRICAL_SURFACE ( 'NONE', #26086, 0.1000000000000000472 ) ;
#8806 = CYLINDRICAL_SURFACE ( 'NONE', #26887, 2.625000000001610267 ) ;
#8807 = CARTESIAN_POINT ( 'NONE',  ( -57.25952994616203995, 3.117691453623994580, -1.800000000000189671 ) ) ;
#8808 = TOROIDAL_SURFACE ( 'NONE', #15884, 1.524417381223824197, 0.05000000000000000278 ) ;
#8809 = EDGE_CURVE ( 'NONE', #17711, #15786, #5274, .T. ) ;
#8810 = DIRECTION ( 'NONE',  ( 1.000000000000000000, 2.586136946169074517E-16, -0.000000000000000000 ) ) ;
#8811 = ADVANCED_FACE ( 'NONE', ( #29204 ), #12182, .T. ) ;
#8812 = EDGE_CURVE ( 'NONE', #18413, #21138, #27404, .T. ) ;
#8813 = AXIS2_PLACEMENT_3D ( 'NONE', #21486, #9754, #9615 ) ;
#8814 = AXIS2_PLACEMENT_3D ( 'NONE', #22870, #3686, #20347 ) ;
#8815 = CARTESIAN_POINT ( 'NONE',  ( -55.98542740578360366, 0.7887156198831754006, -3.845940847736172508 ) ) ;
#8816 = AXIS2_PLACEMENT_3D ( 'NONE', #25757, #18485, #13236 ) ;
#8817 = CARTESIAN_POINT ( 'NONE',  ( -59.57202994616203995, 2.078460969082689846, -3.600000000000193268 ) ) ;
#8818 = CARTESIAN_POINT ( 'NONE',  ( -35.98994760229916068, -0.4576450652446866219, 5.200000002521323772 ) ) ;
#8819 = CARTESIAN_POINT ( 'NONE',  ( 15.03925126672132961, 3.426725943139601327, -3.937891353488703228 ) ) ;
#8820 = ORIENTED_EDGE ( 'NONE', *, *, #29245, .T. ) ;
#8821 = EDGE_CURVE ( 'NONE', #1692, #21492, #17289, .T. ) ;
#8822 = CARTESIAN_POINT ( 'NONE',  ( 58.75000000694006275, 1.658042653848306625, 0.9860766836000441904 ) ) ;
#8823 = ORIENTED_EDGE ( 'NONE', *, *, #19750, .F. ) ;
#8824 = CIRCLE ( 'NONE', #26542, 2.700000000000000178 ) ;
#8825 = DIRECTION ( 'NONE',  ( -1.000000000000000000, 1.219044193948983948E-29, -3.491481338843133355E-15 ) ) ;
#8827 = DIRECTION ( 'NONE',  ( 1.189524669241239263E-14, 0.000000000000000000, 1.000000000000000000 ) ) ;
#8826 = CARTESIAN_POINT ( 'NONE',  ( 56.99999999998442490, 0.7044205509462206916, -2.449516039469794570 ) ) ;
#8828 = ORIENTED_EDGE ( 'NONE', *, *, #13570, .T. ) ;
#8829 = VERTEX_POINT ( 'NONE', #10765 ) ;
#8830 = FACE_BOUND ( 'NONE', #28418, .T. ) ;
#8832 = DIRECTION ( 'NONE',  ( 1.000000000000000000, 3.053848253006669023E-16, -2.042510438544995169E-16 ) ) ;
#8831 = FACE_OUTER_BOUND ( 'NONE', #18144, .T. ) ;
#8833 = ORIENTED_EDGE ( 'NONE', *, *, #2225, .F. ) ;
#8834 = CARTESIAN_POINT ( 'NONE',  ( -57.92292740578360366, 1.073804522883521795, 3.225979517392336682 ) ) ;
#8835 = EDGE_CURVE ( 'NONE', #616, #6201, #21324, .T. ) ;
#8836 = CIRCLE ( 'NONE', #15943, 2.729289321881338548 ) ;
#8837 = APPLICATION_PROTOCOL_DEFINITION ( 'draft international standard', 'automotive_design', 1998, #27395 ) ;
#8838 = CARTESIAN_POINT ( 'NONE',  ( 52.69134963215454803, 4.542747918341202507, -1.570391857504957134 ) ) ;
#8839 = FACE_OUTER_BOUND ( 'NONE', #21108, .T. ) ;
#8840 = EDGE_CURVE ( 'NONE', #10424, #5154, #19341, .T. ) ;
#8841 = CIRCLE ( 'NONE', #4813, 2.649999999999999911 ) ;
#8842 = CYLINDRICAL_SURFACE ( 'NONE', #2241, 1.625000000000001332 ) ;
#8843 = ORIENTED_EDGE ( 'NONE', *, *, #1652, .F. ) ;
#8844 = CARTESIAN_POINT ( 'NONE',  ( 57.02678890911435872, -0.7442859487862443224, 1.783438914669892128 ) ) ;
#8845 = AXIS2_PLACEMENT_3D ( 'NONE', #2708, #19669, #24854 ) ;
#8846 = ORIENTED_EDGE ( 'NONE', *, *, #14484, .F. ) ;
#8847 = CARTESIAN_POINT ( 'NONE',  ( 61.24504608472940248, 0.9290853280814357351, -1.697615787669267240 ) ) ;
#8848 = ADVANCED_FACE ( 'NONE', ( #18232 ), #25374, .T. ) ;
#8849 = CARTESIAN_POINT ( 'NONE',  ( -62.04999999999998295, -2.671081280896084653, -0.3941126626315437642 ) ) ;
#8850 = DIRECTION ( 'NONE',  ( 0.000000000000000000, 0.000000000000000000, 1.000000000000000000 ) ) ;
#8851 = ADVANCED_FACE ( 'NONE', ( #6329 ), #25185, .F. ) ;
#8852 = DIRECTION ( 'NONE',  ( -0.000000000000000000, 1.000000000000000000, 3.491481338843133355E-15 ) ) ;
#8854 = CARTESIAN_POINT ( 'NONE',  ( -67.34999999999998010, -2.149333209074760109, -0.05354209902869064286 ) ) ;
#8853 = CARTESIAN_POINT ( 'NONE',  ( 51.25000000000002842, -0.9938153758920951208, 1.589954715908409977 ) ) ;
#8855 = VECTOR ( 'NONE', #17382, 1000.000000000000114 ) ;
#8856 = AXIS2_PLACEMENT_3D ( 'NONE', #14679, #12447, #31308 ) ;
#8857 = CARTESIAN_POINT ( 'NONE',  ( 47.73415789227374972, -4.410482998349072759, -1.311567113539440221 ) ) ;
#8859 = CARTESIAN_POINT ( 'NONE',  ( 60.75000000000002842, -0.6499999999993638644, 1.489337100860647967 ) ) ;
#8858 = CARTESIAN_POINT ( 'NONE',  ( -64.29999999999996874, 4.961699865966959239E-16, 2.647079050581693988E-15 ) ) ;
#8860 = AXIS2_PLACEMENT_3D ( 'NONE', #28394, #3851, #26004 ) ;
#8861 = ORIENTED_EDGE ( 'NONE', *, *, #21512, .F. ) ;
#8862 = FACE_OUTER_BOUND ( 'NONE', #22448, .T. ) ;
#8863 = CARTESIAN_POINT ( 'NONE',  ( 47.00000000000002132, -3.726179070414207928, -1.710435481158852467 ) ) ;
#8865 = DIRECTION ( 'NONE',  ( 3.491481338843133355E-15, 0.000000000000000000, 1.000000000000000000 ) ) ;
#8864 = CARTESIAN_POINT ( 'NONE',  ( 58.75000000000000000, 1.871930101357349940, 0.6019471833021664553 ) ) ;
#8866 = CARTESIAN_POINT ( 'NONE',  ( 15.44259799936803468, -5.012895491272645998, 1.399447560527413925 ) ) ;
#8867 = VECTOR ( 'NONE', #29532, 1000.000000000000000 ) ;
#8868 = ORIENTED_EDGE ( 'NONE', *, *, #23755, .T. ) ;
#8869 = CARTESIAN_POINT ( 'NONE',  ( 53.82520270936416296, 4.899646637710924679, 2.049999999999811973 ) ) ;
#8870 = CARTESIAN_POINT ( 'NONE',  ( -60.49999999999995737, 0.8638545240222846866, -4.212333719130787912 ) ) ;
#8871 = AXIS2_PLACEMENT_3D ( 'NONE', #22463, #23213, #27941 ) ;
#8872 = ORIENTED_EDGE ( 'NONE', *, *, #13024, .T. ) ;
#8873 = DIRECTION ( 'NONE',  ( 1.000000000000000000, 1.047444401652940007E-14, 0.000000000000000000 ) ) ;
#8874 = EDGE_LOOP ( 'NONE', ( #18914, #3079, #21519, #2086 ) ) ;
#8875 = EDGE_CURVE ( 'NONE', #1101, #27607, #603, .T. ) ;
#8876 = CARTESIAN_POINT ( 'NONE',  ( 58.75000000000000000, 1.963941025093405957, 0.09694516908175258851 ) ) ;
#8877 = ORIENTED_EDGE ( 'NONE', *, *, #1021, .F. ) ;
#8878 =( NAMED_UNIT ( * ) PLANE_ANGLE_UNIT ( ) SI_UNIT ( $, .RADIAN. ) );
#8879 = ADVANCED_FACE ( 'NONE', ( #8238 ), #7913, .T. ) ;
#8880 = CARTESIAN_POINT ( 'NONE',  ( -54.88452994616206126, 3.117691453623979481, 1.799999999999816858 ) ) ;
#8881 = CARTESIAN_POINT ( 'NONE',  ( -58.20655989232411542, -3.925981830489445379, -2.207870066386390016E-13 ) ) ;
#8882 = ORIENTED_EDGE ( 'NONE', *, *, #24868, .T. ) ;
#8883 = ADVANCED_FACE ( 'NONE', ( #15359 ), #10622, .T. ) ;
#8884 = EDGE_LOOP ( 'NONE', ( #10902, #26807, #5141, #7105 ) ) ;
#8885 = AXIS2_PLACEMENT_3D ( 'NONE', #13368, #23062, #11027 ) ;
#8886 = VERTEX_POINT ( 'NONE', #21075 ) ;
#8887 = CARTESIAN_POINT ( 'NONE',  ( -56.31249999999998579, -1.962990915244731793, 3.399999999999792077 ) ) ;
#8888 = VECTOR ( 'NONE', #5574, 1000.000000000000000 ) ;
#8889 = CARTESIAN_POINT ( 'NONE',  ( 57.02825620192501077, -0.8138444489294278661, 2.469346200785457413 ) ) ;
#8890 = CARTESIAN_POINT ( 'NONE',  ( 51.80000000000002558, 4.349402395915089592, 1.698746272247092959 ) ) ;
#8891 = AXIS2_PLACEMENT_3D ( 'NONE', #20868, #1678, #13386 ) ;
#8892 = LINE ( 'NONE', #28381, #27596 ) ;
#8893 = AXIS2_PLACEMENT_3D ( 'NONE', #18129, #11444, #1309 ) ;
#8894 = DIRECTION ( 'NONE',  ( 0.000000000000000000, 0.000000000000000000, -1.000000000000000000 ) ) ;
#8895 = AXIS2_PLACEMENT_3D ( 'NONE', #18270, #13320, #27442 ) ;
#8896 = CIRCLE ( 'NONE', #26611, 2.800000000000000266 ) ;
#8897 = AXIS2_PLACEMENT_3D ( 'NONE', #27806, #6263, #27643 ) ;
#8899 = CARTESIAN_POINT ( 'NONE',  ( 47.00000000000002132, 1.426739617975221641, 3.843750000000023093 ) ) ;
#8898 = DIRECTION ( 'NONE',  ( 1.000000000000000000, 1.047444401652940007E-14, 0.000000000000000000 ) ) ;
#8900 = LINE ( 'NONE', #1614, #2361 ) ;
#8901 = CARTESIAN_POINT ( 'NONE',  ( 52.20711756518982583, 0.7500000000005468959, -1.718465885608440269 ) ) ;
#8902 = CARTESIAN_POINT ( 'NONE',  ( 15.03925126672122303, 5.377732432866646484, -0.5657657256215100627 ) ) ;
#8903 = CARTESIAN_POINT ( 'NONE',  ( 58.74999981196286569, -1.649561145038163756, -1.050519579371713252 ) ) ;
#8904 = CARTESIAN_POINT ( 'NONE',  ( 57.05000000000001847, 0.7500000000000000000, -2.421260002560650104 ) ) ;
#8905 = AXIS2_PLACEMENT_3D ( 'NONE', #9229, #18581, #13948 ) ;
#8906 = CARTESIAN_POINT ( 'NONE',  ( -44.49999999999999289, -1.500000000000004663, 3.363870538531272825 ) ) ;
#8907 = VERTEX_POINT ( 'NONE', #23600 ) ;
#8909 = CARTESIAN_POINT ( 'NONE',  ( 50.40000000000001279, -0.6304760106459028624, 3.950000000000022826 ) ) ;
#8908 = DIRECTION ( 'NONE',  ( 1.000000000000000000, 0.000000000000000000, 0.000000000000000000 ) ) ;
#8910 = CIRCLE ( 'NONE', #8885, 4.199999999999993072 ) ;
#8911 = CIRCLE ( 'NONE', #5397, 0.1000000000000000472 ) ;
#8912 = AXIS2_PLACEMENT_3D ( 'NONE', #3802, #17612, #27257 ) ;
#8913 = VERTEX_POINT ( 'NONE', #9025 ) ;
#8914 = DIRECTION ( 'NONE',  ( -3.002035892788116966E-16, 0.9996898646859343485, 0.02490330187381124133 ) ) ;
#8915 = DIRECTION ( 'NONE',  ( 3.002035892788117952E-16, -0.9996898646859344595, -0.02490330187381124133 ) ) ;
#8916 = CARTESIAN_POINT ( 'NONE',  ( -55.25952994616203995, -3.117691453623963938, -1.800000000000207434 ) ) ;
#8917 = EDGE_LOOP ( 'NONE', ( #30908, #4664, #20107, #2395 ) ) ;
#8918 = AXIS2_PLACEMENT_3D ( 'NONE', #10159, #27088, #5411 ) ;
#8919 = ORIENTED_EDGE ( 'NONE', *, *, #14292, .T. ) ;
#8920 = CARTESIAN_POINT ( 'NONE',  ( -57.77499999999997016, -0.9643027244899882167, 4.702139965541347166 ) ) ;
#8921 = ORIENTED_EDGE ( 'NONE', *, *, #29386, .T. ) ;
#8922 = TOROIDAL_SURFACE ( 'NONE', #19054, 4.000000000000022204, 0.1000000000000000056 ) ;
#8923 = ADVANCED_FACE ( 'NONE', ( #11716, #16791 ), #19011, .T. ) ;
#8924 = CARTESIAN_POINT ( 'NONE',  ( 58.75000018803721247, -1.701355787207014192, 0.9251739982210235302 ) ) ;
#8925 = ORIENTED_EDGE ( 'NONE', *, *, #17110, .T. ) ;
#8926 = CYLINDRICAL_SURFACE ( 'NONE', #12528, 0.2500000000000000000 ) ;
#8927 = AXIS2_PLACEMENT_3D ( 'NONE', #15411, #27598, #15732 ) ;
#8928 = AXIS2_PLACEMENT_3D ( 'NONE', #11231, #20906, #23909 ) ;
#8929 =( BOUNDED_CURVE ( )  B_SPLINE_CURVE ( 3, ( #5810, #17854, #25121, #5654 ),
 .UNSPECIFIED., .F., .T. ) 
 B_SPLINE_CURVE_WITH_KNOTS ( ( 4, 4 ),
 ( 4.041453792691655167, 4.300872134317202722 ),
 .UNSPECIFIED. ) 
 CURVE ( )  GEOMETRIC_REPRESENTATION_ITEM ( )  RATIONAL_B_SPLINE_CURVE ( ( 1.000000000000000000, 0.9943997021150918769, 0.9943997021150918769, 1.000000000000000000 ) ) 
 REPRESENTATION_ITEM ( '' )  );
#8930 = DIRECTION ( 'NONE',  ( -1.000000000000000000, 0.000000000000000000, 1.047444401652940007E-14 ) ) ;
#8931 = FACE_BOUND ( 'NONE', #10499, .T. ) ;
#8932 = VERTEX_POINT ( 'NONE', #2053 ) ;
#8933 = EDGE_LOOP ( 'NONE', ( #8742, #26296 ) ) ;
#8934 = CARTESIAN_POINT ( 'NONE',  ( 47.00000000000002132, -4.227689052994015206, -1.125730994152046582 ) ) ;
#8935 = DIRECTION ( 'NONE',  ( -1.000000000000000000, 1.219044193948983948E-29, -3.491481338843133355E-15 ) ) ;
#8936 = CARTESIAN_POINT ( 'NONE',  ( 56.95206911348624601, -0.7375298837344119729, -2.493227876267903653 ) ) ;
#8937 = CIRCLE ( 'NONE', #18073, 0.7500000000000002220 ) ;
#8938 = LINE ( 'NONE', #28266, #13425 ) ;
#8939 = DIRECTION ( 'NONE',  ( -1.047444401652940007E-14, 0.000000000000000000, -1.000000000000000000 ) ) ;
#8940 = AXIS2_PLACEMENT_3D ( 'NONE', #18799, #1835, #23857 ) ;
#8941 = EDGE_CURVE ( 'NONE', #12243, #29519, #6405, .T. ) ;
#8942 = DIRECTION ( 'NONE',  ( -1.000000000000000000, 0.000000000000000000, 0.000000000000000000 ) ) ;
#8943 = CIRCLE ( 'NONE', #26659, 0.4576450603546982632 ) ;
#8944 = CARTESIAN_POINT ( 'NONE',  ( 59.34999999999998721, 1.401298464324817071E-42, -4.000000000000621725 ) ) ;
#8945 = DIRECTION ( 'NONE',  ( -4.275831445896958607E-31, 1.000000000000000000, -1.224646799147353207E-16 ) ) ;
#8946 = CLOSED_SHELL ( 'NONE', ( #19391, #20297, #21050, #11430, #25856, #7657, #6799, #11241, #7364, #25289 ) ) ;
#8947 = AXIS2_PLACEMENT_3D ( 'NONE', #498, #11799, #24555 ) ;
#8948 = CARTESIAN_POINT ( 'NONE',  ( -59.28507118137919463, -2.275557563509374326, 1.363277995769353934 ) ) ;
#8949 = CARTESIAN_POINT ( 'NONE',  ( 15.03925126672132961, 4.018128179617565188, -3.618665901676623164 ) ) ;
#8950 = VECTOR ( 'NONE', #5991, 1000.000000000000000 ) ;
#8951 = CARTESIAN_POINT ( 'NONE',  ( -35.85663232820583346, -3.817150320980684075, 2.203324261490539282 ) ) ;
#8952 = VECTOR ( 'NONE', #1196, 1000.000000000000000 ) ;
#8953 = CARTESIAN_POINT ( 'NONE',  ( 61.25000000000000000, 1.960427193528571532, 0.3958853607757182314 ) ) ;
#8954 = VECTOR ( 'NONE', #11707, 1000.000000000000000 ) ;
#8955 = VERTEX_POINT ( 'NONE', #4260 ) ;
#8956 = ORIENTED_EDGE ( 'NONE', *, *, #2074, .T. ) ;
#8957 = ORIENTED_EDGE ( 'NONE', *, *, #12313, .T. ) ;
#8958 = CARTESIAN_POINT ( 'NONE',  ( 51.41799912780150805, -3.967692247893626512, 1.365930198224605707 ) ) ;
#8959 = EDGE_LOOP ( 'NONE', ( #17781, #5187, #17851, #7465 ) ) ;
#8960 = CARTESIAN_POINT ( 'NONE',  ( 53.71202192472755144, 7.447163568589559191, 2.049999999999939426 ) ) ;
#8961 = CARTESIAN_POINT ( 'NONE',  ( -57.53335481156722864, -4.108500314926510022, 1.367561758111407455 ) ) ;
#8963 = CARTESIAN_POINT ( 'NONE',  ( -36.30424252565907750, 2.966783028120403731, 4.272059443775344079 ) ) ;
#8962 = DIRECTION ( 'NONE',  ( 1.000000000000000000, -1.219044193948983948E-29, 3.491481338843133355E-15 ) ) ;
#8964 = CONICAL_SURFACE ( 'NONE', #24649, 1.350000000000000089, 0.04164257909858841422 ) ;
#8965 = ORIENTED_EDGE ( 'NONE', *, *, #738, .F. ) ;
#8966 = CARTESIAN_POINT ( 'NONE',  ( 51.80000000000001847, -0.2842225609755594795, -1.577752156565102655E-15 ) ) ;
#8967 = AXIS2_PLACEMENT_3D ( 'NONE', #30862, #9793, #28483 ) ;
#8968 = VERTEX_POINT ( 'NONE', #16312 ) ;
#8969 = ADVANCED_FACE ( 'NONE', ( #6977 ), #21595, .T. ) ;
#8970 = DIRECTION ( 'NONE',  ( -1.000000000000000000, -1.047444401652940007E-14, -0.000000000000000000 ) ) ;
#8971 =( BOUNDED_SURFACE ( )  B_SPLINE_SURFACE ( 3, 2, ( 
 ( #21646, #9603, #4351 ),
 ( #16394, #9277, #19263 ),
 ( #28899, #2462, #14482 ),
 ( #24157, #6585, #16244 ),
 ( #4193, #23517, #1816 ),
 ( #30803, #9116, #28429 ),
 ( #6733, #21329, #30962 ),
 ( #18940, #28584, #24448 ),
 ( #22254, #17188, #27134 ),
 ( #392, #7668, #10346 ) ),
 .UNSPECIFIED., .F., .F., .F. ) 
 B_SPLINE_SURFACE_WITH_KNOTS ( ( 4, 2, 2, 2, 4 ),
 ( 3, 3 ),
 ( 0.0001706658715701353925, 0.0002229276920781100868, 0.0002751895125860847539, 0.0003274513330940594211, 0.0003797131536020340883 ),
 ( 0.000000000000000000, 1.000000000000000000 ),
 .UNSPECIFIED. ) 
 GEOMETRIC_REPRESENTATION_ITEM ( )  RATIONAL_B_SPLINE_SURFACE ( (
 ( 1.000000000000000000, 0.7071067811873461562, 1.000000000000000000),
 ( 1.000000000000000000, 0.7375607040708931361, 1.000000000000000000),
 ( 1.000000000000000000, 0.7730431127425965165, 1.000000000000000000),
 ( 1.000000000000000000, 0.8321012486971868238, 1.000000000000000000),
 ( 1.000000000000000000, 0.8541932017382776188, 1.000000000000000000),
 ( 1.000000000000000000, 0.8545723906027511418, 1.000000000000000000),
 ( 1.000000000000000000, 0.8327032135021242842, 1.000000000000000000),
 ( 1.000000000000000000, 0.7734559727054323153, 1.000000000000000000),
 ( 1.000000000000000000, 0.7377766653991476575, 1.000000000000000000),
 ( 1.000000000000000000, 0.7071067811865509034, 1.000000000000000000) ) ) 
 REPRESENTATION_ITEM ( '' )  SURFACE ( )  );
#8972 = CIRCLE ( 'NONE', #22646, 0.05000000000000009298 ) ;
#8973 = ORIENTED_EDGE ( 'NONE', *, *, #13599, .T. ) ;
#8975 = CYLINDRICAL_SURFACE ( 'NONE', #4924, 0.1000000000000000472 ) ;
#8974 = CARTESIAN_POINT ( 'NONE',  ( 15.03925126672132784, 4.683225679163323996, 2.703237727951258051 ) ) ;
#8976 = CARTESIAN_POINT ( 'NONE',  ( -35.85663232820584057, 3.056483311920880297, -4.206888370749704897 ) ) ;
#8977 = ORIENTED_EDGE ( 'NONE', *, *, #31061, .F. ) ;
#8978 = CARTESIAN_POINT ( 'NONE',  ( -36.76447480099743359, 4.924630501335110822, -2.234249019593746333 ) ) ;
#8979 = EDGE_CURVE ( 'NONE', #25687, #5427, #6912, .T. ) ;
#8980 = CARTESIAN_POINT ( 'NONE',  ( 58.73371041428907091, 1.830356084956107798, -0.4073466955372750942 ) ) ;
#8981 = AXIS2_PLACEMENT_3D ( 'NONE', #4374, #16110, #9142 ) ;
#8982 = CARTESIAN_POINT ( 'NONE',  ( 46.90000000000001990, -4.131056160354152240, 1.099999999999999867 ) ) ;
#8983 = CARTESIAN_POINT ( 'NONE',  ( -61.34999999999997300, 1.397055221233662433E-15, 2.044538471210920981E-15 ) ) ;
#8984 = AXIS2_PLACEMENT_3D ( 'NONE', #4669, #14324, #24450 ) ;
#8985 = CARTESIAN_POINT ( 'NONE',  ( -59.50952994616202574, 3.117691453623994580, -1.800000000000197664 ) ) ;
#8986 = CARTESIAN_POINT ( 'NONE',  ( -59.19999999999996732, 3.264622394567737729, -0.9498634748674483763 ) ) ;
#8987 = EDGE_CURVE ( 'NONE', #16661, #15552, #2365, .T. ) ;
#8988 = DIRECTION ( 'NONE',  ( -0.9993908270190953180, 0.03489949670251430575, 3.490905158897711881E-15 ) ) ;
#8989 = CARTESIAN_POINT ( 'NONE',  ( 67.95000000000003126, -1.025519176787267142E-28, -7.117384709231726808E-13 ) ) ;
#8990 = CIRCLE ( 'NONE', #25095, 3.399999999999999911 ) ;
#8991 = AXIS2_PLACEMENT_3D ( 'NONE', #22782, #27970, #15645 ) ;
#8992 = CARTESIAN_POINT ( 'NONE',  ( -57.86042740578360366, -0.7887156198831708487, 3.845940847736171619 ) ) ;
#8993 = CIRCLE ( 'NONE', #3447, 4.099999999999992539 ) ;
#8994 = CARTESIAN_POINT ( 'NONE',  ( -74.39999999999997726, -2.588216748940040213E-15, 4.710014593512140639E-15 ) ) ;
#8995 = ORIENTED_EDGE ( 'NONE', *, *, #22498, .F. ) ;
#8996 = ADVANCED_FACE ( 'NONE', ( #4587 ), #14237, .T. ) ;
#8997 = DIRECTION ( 'NONE',  ( 3.016910393003118404E-15, 0.000000000000000000, 1.000000000000000000 ) ) ;
#8998 = CARTESIAN_POINT ( 'NONE',  ( 54.40293493925265977, 6.717672571224094114, -2.002198665876510741 ) ) ;
#8999 = CARTESIAN_POINT ( 'NONE',  ( 52.88898622668489224, 4.646829164113958299, 1.580883332821158671 ) ) ;
#9000 = CARTESIAN_POINT ( 'NONE',  ( 51.45655683570189609, 0.9591657938401617622, 1.468576096419531352 ) ) ;
#9001 = VERTEX_POINT ( 'NONE', #14081 ) ;
#9002 = CARTESIAN_POINT ( 'NONE',  ( 58.74999981404332061, 1.734728236459932127, 0.9032433253523316496 ) ) ;
#9003 = ORIENTED_EDGE ( 'NONE', *, *, #25259, .F. ) ;
#9005 = CARTESIAN_POINT ( 'NONE',  ( 58.75000000000003553, -1.469015551795666674, 1.320082690054176666 ) ) ;
#9004 = FACE_OUTER_BOUND ( 'NONE', #13257, .T. ) ;
#9006 = ORIENTED_EDGE ( 'NONE', *, *, #12259, .F. ) ;
#9007 = ORIENTED_EDGE ( 'NONE', *, *, #18178, .F. ) ;
#9008 = CARTESIAN_POINT ( 'NONE',  ( -59.13463329438567229, -2.488830503680597328, -0.9121239897850130784 ) ) ;
#9009 = EDGE_CURVE ( 'NONE', #23673, #25393, #9519, .T. ) ;
#9010 = DIRECTION ( 'NONE',  ( 0.000000000000000000, -0.9996898646859344595, -0.02490330187381124133 ) ) ;
#9012 = CARTESIAN_POINT ( 'NONE',  ( -35.85663232820583346, -4.683225679163361299, 2.703237727951226077 ) ) ;
#9011 = CARTESIAN_POINT ( 'NONE',  ( 54.40000000000001990, 1.734723475976807094E-15, 0.000000000000000000 ) ) ;
#9013 = ORIENTED_EDGE ( 'NONE', *, *, #18150, .F. ) ;
#9014 = CARTESIAN_POINT ( 'NONE',  ( -60.98542740578359656, 2.936324665650206445, 2.606018187048499968 ) ) ;
#9015 = EDGE_CURVE ( 'NONE', #20639, #3532, #1902, .T. ) ;
#9016 = PLANE ( 'NONE',  #20844 ) ;
#9017 = CONTEXT_DEPENDENT_SHAPE_REPRESENTATION ( #1501, #13337 ) ;
#9018 = AXIS2_PLACEMENT_3D ( 'NONE', #25987, #9060, #11596 ) ;
#9019 = CARTESIAN_POINT ( 'NONE',  ( -59.38356253233095572, 2.342592582602649021, 1.264794915520445429 ) ) ;
#9020 = DIRECTION ( 'NONE',  ( 1.000000000000000000, 3.054025858079668409E-16, -2.042474015755241579E-16 ) ) ;
#9021 = CARTESIAN_POINT ( 'NONE',  ( -54.46895629856896903, 1.503487923075246480, -4.032311158269683560 ) ) ;
#9022 = ORIENTED_EDGE ( 'NONE', *, *, #20264, .F. ) ;
#9023 = B_SPLINE_CURVE_WITH_KNOTS ( 'NONE', 3,
 ( #12369, #17295, #19689, #5414, #29324, #7636, #18088, #20774, #28025, #15544, #22688, #20158, #1432, #3803, #13447, #25348 ),
 .UNSPECIFIED., .F., .F.,
 ( 4, 3, 3, 3, 3, 4 ),
 ( 0.000000000000000000, 2.715478742569115014E-05, 6.149153169279458048E-05, 9.810361480504433687E-05, 0.0001359429311246336211, 0.0001737107874904862475 ),
 .UNSPECIFIED. ) ;
#9024 = EDGE_CURVE ( 'NONE', #13995, #26742, #20196, .T. ) ;
#9025 = CARTESIAN_POINT ( 'NONE',  ( 50.50000000000002132, 2.428612866367529932E-14, -4.100000000000022737 ) ) ;
#9026 = CARTESIAN_POINT ( 'NONE',  ( -36.68133364217572989, 2.563573972737328788, -4.761506352252359520 ) ) ;
#9027 = CARTESIAN_POINT ( 'NONE',  ( -59.38281074049554320, 3.338301835134465101, 1.250136525132569787 ) ) ;
#9028 = CARTESIAN_POINT ( 'NONE',  ( -59.27103329757905925, 2.428242106091510699, -1.066113908650129893 ) ) ;
#9029 = CARTESIAN_POINT ( 'NONE',  ( 16.00221665700883378, -0.5763363385013805518, -5.380853831843025681 ) ) ;
#9031 = CARTESIAN_POINT ( 'NONE',  ( 41.48619405471884392, -151.3359592902621955, 1.549999999999835953 ) ) ;
#9030 = DIRECTION ( 'NONE',  ( -1.000000000000000000, -2.586136946169074517E-16, 0.000000000000000000 ) ) ;
#9032 = EDGE_CURVE ( 'NONE', #28342, #17261, #22637, .T. ) ;
#9033 =( GEOMETRIC_REPRESENTATION_CONTEXT ( 3 ) GLOBAL_UNCERTAINTY_ASSIGNED_CONTEXT ( ( #10133 ) ) GLOBAL_UNIT_ASSIGNED_CONTEXT ( ( #18108, #5595, #20175 ) ) REPRESENTATION_CONTEXT ( 'NONE', 'WORKASPACE' ) );
#9034 = CARTESIAN_POINT ( 'NONE',  ( -62.09999999999998010, -2.684508219953025243, -0.3645818587800867538 ) ) ;
#9036 = CARTESIAN_POINT ( 'NONE',  ( 50.32627973729707094, -1.373706569044463199, -3.853361913240786141 ) ) ;
#9035 = DIRECTION ( 'NONE',  ( -1.000000000000000000, 1.219044193948983948E-29, -3.491481338843133355E-15 ) ) ;
#9037 = ORIENTED_EDGE ( 'NONE', *, *, #27945, .F. ) ;
#9038 = AXIS2_PLACEMENT_3D ( 'NONE', #7599, #29579, #7898 ) ;
#9039 = FACE_OUTER_BOUND ( 'NONE', #9614, .T. ) ;
#9040 = CARTESIAN_POINT ( 'NONE',  ( 54.15675781068899397, 5.684314874070254042, -2.050000000000189004 ) ) ;
#9041 = B_SPLINE_CURVE_WITH_KNOTS ( 'NONE', 3,
 ( #28720, #18903, #21137, #26006, #4633, #13963 ),
 .UNSPECIFIED., .F., .F.,
 ( 4, 2, 4 ),
 ( 0.000000000000000000, 0.0001924639855377290119, 0.0003849279710754580238 ),
 .UNSPECIFIED. ) ;
#9043 = CARTESIAN_POINT ( 'NONE',  ( -36.42771574642716104, 5.277035221755925321, 1.205525476379240679 ) ) ;
#9042 = CARTESIAN_POINT ( 'NONE',  ( 58.74154451056408988, 1.784780193104163359, 0.5746581230792165984 ) ) ;
#9044 = CARTESIAN_POINT ( 'NONE',  ( 16.10624235918717773, -5.192953935288615597, 1.516181439821707500 ) ) ;
#9045 = ORIENTED_EDGE ( 'NONE', *, *, #25736, .F. ) ;
#9046 = VERTEX_POINT ( 'NONE', #22752 ) ;
#9047 = CARTESIAN_POINT ( 'NONE',  ( 48.30000000000001847, 0.6462379109121000331, 4.048750000000023164 ) ) ;
#9048 = CARTESIAN_POINT ( 'NONE',  ( 51.80000000000002558, -4.291790910095608425, 1.352971095042299954 ) ) ;
#9049 = ADVANCED_FACE ( 'NONE', ( #12751 ), #4892, .F. ) ;
#9050 = ORIENTED_EDGE ( 'NONE', *, *, #22961, .F. ) ;
#9051 = EDGE_CURVE ( 'NONE', #5002, #6209, #4690, .T. ) ;
#9052 = DIRECTION ( 'NONE',  ( 0.000000000000000000, -1.000000000000000000, -3.491481338843132961E-15 ) ) ;
#9053 = ORIENTED_EDGE ( 'NONE', *, *, #14681, .T. ) ;
#9054 = ADVANCED_FACE ( 'NONE', ( #5484 ), #30554, .T. ) ;
#9055 = CARTESIAN_POINT ( 'NONE',  ( 58.74999981404331351, 1.953940384112647033, -0.08513245267633837154 ) ) ;
#9056 = VERTEX_POINT ( 'NONE', #10697 ) ;
#9057 = CARTESIAN_POINT ( 'NONE',  ( 25.60313575641834660, 5.243666353503796174, 1.949999999999910472 ) ) ;
#9058 = CARTESIAN_POINT ( 'NONE',  ( -58.95655989232412253, -3.925981830489445379, -2.234056176427713674E-13 ) ) ;
#9059 = ORIENTED_EDGE ( 'NONE', *, *, #19326, .T. ) ;
#9060 = DIRECTION ( 'NONE',  ( 0.000000000000000000, 0.000000000000000000, 1.000000000000000000 ) ) ;
#9061 = EDGE_LOOP ( 'NONE', ( #22741, #4407, #19095, #28880 ) ) ;
#9062 = ORIENTED_EDGE ( 'NONE', *, *, #12693, .T. ) ;
#9063 = MECHANICAL_DESIGN_GEOMETRIC_PRESENTATION_REPRESENTATION (  '', ( #2521 ), #7557 ) ;
#9064 = AXIS2_PLACEMENT_3D ( 'NONE', #19656, #24529, #17412 ) ;
#9065 = CARTESIAN_POINT ( 'NONE',  ( -60.12499999999997868, -3.920666489018291502E-15, 3.399999999999785860 ) ) ;
#9066 = CARTESIAN_POINT ( 'NONE',  ( -59.19999999999997442, 8.366749974758448157E-15, -2.103076948839454410E-13 ) ) ;
#9067 = CARTESIAN_POINT ( 'NONE',  ( 58.65000000000000568, 1.571497941946485177, 1.022750809562084306 ) ) ;
#9068 = DIRECTION ( 'NONE',  ( 0.000000000000000000, -0.9996898646859343485, -0.02490330187381123786 ) ) ;
#9069 = CARTESIAN_POINT ( 'NONE',  ( 61.01567056675808942, 0.5566600462024857698, 1.706616170210761618 ) ) ;
#9071 = CARTESIAN_POINT ( 'NONE',  ( 69.25000000000001421, 4.557543281186736018E-17, -7.253552481446610839E-13 ) ) ;
#9070 =( LENGTH_UNIT ( ) NAMED_UNIT ( * ) SI_UNIT ( .MILLI., .METRE. ) );
#9072 = EDGE_CURVE ( 'NONE', #28914, #17227, #6205, .T. ) ;
#9073 = DIRECTION ( 'NONE',  ( 1.000000000000000000, 1.047444401652940007E-14, 0.000000000000000000 ) ) ;
#9074 = DIRECTION ( 'NONE',  ( -1.000000000000000000, -0.000000000000000000, -0.000000000000000000 ) ) ;
#9075 = CARTESIAN_POINT ( 'NONE',  ( 57.03253626007334987, 0.8141194241917997232, 2.469252834999610791 ) ) ;
#9077 = AXIS2_PLACEMENT_3D ( 'NONE', #5382, #26188, #7614 ) ;
#9076 = FACE_OUTER_BOUND ( 'NONE', #6092, .T. ) ;
#9078 = EDGE_CURVE ( 'NONE', #23530, #3064, #11474, .T. ) ;
#9079 = CARTESIAN_POINT ( 'NONE',  ( 50.38147505302058704, 1.153996415704716449, -3.890257736381618869 ) ) ;
#9080 = ORIENTED_EDGE ( 'NONE', *, *, #13802, .F. ) ;
#9082 = CARTESIAN_POINT ( 'NONE',  ( 48.48449022203101322, -1.386241252175273608, -3.851058308531627450 ) ) ;
#9081 = CARTESIAN_POINT ( 'NONE',  ( 50.56924445453659445, -0.1015585333197664281, 0.8011027422770335971 ) ) ;
#9083 = CARTESIAN_POINT ( 'NONE',  ( 47.00000000000002132, 2.428612866367529932E-14, -4.100000000000022737 ) ) ;
#9084 = CARTESIAN_POINT ( 'NONE',  ( -59.29999999999997584, 0.7533615035078071731, -3.673546848079177529 ) ) ;
#9085 = AXIS2_PLACEMENT_3D ( 'NONE', #13233, #5814, #27824 ) ;
#9086 = AXIS2_PLACEMENT_3D ( 'NONE', #24795, #21715, #2953 ) ;
#9087 = ORIENTED_EDGE ( 'NONE', *, *, #261, .T. ) ;
#9088 = CARTESIAN_POINT ( 'NONE',  ( 58.75000000000002132, 6.153735859711025284E-13, 3.111507638930570854E-58 ) ) ;
#9089 = CARTESIAN_POINT ( 'NONE',  ( 15.03925126672132961, -3.056483311920865642, 4.206888370749720885 ) ) ;
#9090 = CARTESIAN_POINT ( 'NONE',  ( -59.99999999999997158, -2.944486372867089141, 1.699999999999775913 ) ) ;
#9091 = VERTEX_POINT ( 'NONE', #19327 ) ;
#9092 = EDGE_LOOP ( 'NONE', ( #16111, #15743 ) ) ;
#9093 = ADVANCED_FACE ( 'NONE', ( #28964 ), #18472, .F. ) ;
#9094 = CARTESIAN_POINT ( 'NONE',  ( 58.75000000000004263, -2.008165151418373373, -0.5380862305909229759 ) ) ;
#9095 = ORIENTED_EDGE ( 'NONE', *, *, #28384, .T. ) ;
#9096 = TOROIDAL_SURFACE ( 'NONE', #18236, 2.750000000000000444, 0.05000000000000000278 ) ;
#9097 = CARTESIAN_POINT ( 'NONE',  ( 51.22715433738865443, 0.9941391646906797552, -1.410349289489640334 ) ) ;
#9098 = LINE ( 'NONE', #30943, #19993 ) ;
#9099 = ORIENTED_EDGE ( 'NONE', *, *, #26051, .F. ) ;
#9100 = DIRECTION ( 'NONE',  ( 0.000000000000000000, 0.9996898646859343485, 0.02490330187381116153 ) ) ;
#9101 = FACE_OUTER_BOUND ( 'NONE', #26818, .T. ) ;
#9102 = CARTESIAN_POINT ( 'NONE',  ( -37.18272003341174781, 5.407411300779116914, 0.000000000000000000 ) ) ;
#9103 = ORIENTED_EDGE ( 'NONE', *, *, #6348, .F. ) ;
#9104 = ORIENTED_EDGE ( 'NONE', *, *, #6682, .F. ) ;
#9105 = DIRECTION ( 'NONE',  ( -1.000000000000000000, -2.586136946169074517E-16, 0.000000000000000000 ) ) ;
#9106 = DIRECTION ( 'NONE',  ( 0.000000000000000000, 0.000000000000000000, 1.000000000000000000 ) ) ;
#9107 = CARTESIAN_POINT ( 'NONE',  ( -55.03335481156724995, 0.7533615035078067290, -3.673546848079180194 ) ) ;
#9108 = B_SPLINE_CURVE_WITH_KNOTS ( 'NONE', 3,
 ( #12752, #13361, #8171, #22429 ),
 .UNSPECIFIED., .F., .F.,
 ( 4, 4 ),
 ( 0.0001543670095910070058, 0.0003084486524517391867 ),
 .UNSPECIFIED. ) ;
#9109 = ORIENTED_EDGE ( 'NONE', *, *, #10356, .F. ) ;
#9110 = CARTESIAN_POINT ( 'NONE',  ( 49.05000000000002558, 1.401298464324817071E-42, -5.137714790107672405E-13 ) ) ;
#9111 = CARTESIAN_POINT ( 'NONE',  ( 58.74999981404331351, 1.441842230226507926, 1.321446761054005492 ) ) ;
#9112 = CIRCLE ( 'NONE', #18729, 0.1500000000000000777 ) ;
#9113 = CARTESIAN_POINT ( 'NONE',  ( 15.03925126672132961, -3.275050215668582787, -2.949461045527606462 ) ) ;
#9114 = CARTESIAN_POINT ( 'NONE',  ( 57.01256279823148532, 0.7331429619035759737, -1.793127402884417965 ) ) ;
#9116 = CARTESIAN_POINT ( 'NONE',  ( 58.72200624034183392, -0.9564954546387592904, 1.612834625125136201 ) ) ;
#9115 = CARTESIAN_POINT ( 'NONE',  ( 58.75000000000002132, -0.6121634413828838106, -1.877732920580933218 ) ) ;
#9117 = VECTOR ( 'NONE', #6569, 1000.000000000000227 ) ;
#9118 = PRODUCT_DEFINITION_SHAPE ( 'NONE', 'NONE',  #31328 ) ;
#9119 = ADVANCED_FACE ( 'NONE', ( #25262 ), #1361, .T. ) ;
#9120 = AXIS2_PLACEMENT_3D ( 'NONE', #23208, #27629, #1041 ) ;
#9121 = FACE_OUTER_BOUND ( 'NONE', #20480, .T. ) ;
#9122 = EDGE_CURVE ( 'NONE', #17229, #18794, #2879, .T. ) ;
#9123 = LINE ( 'NONE', #16396, #30726 ) ;
#9124 = CARTESIAN_POINT ( 'NONE',  ( 22.07280086217093640, 8.086143481909140007, -1.950000000000076339 ) ) ;
#9125 = DIRECTION ( 'NONE',  ( 0.000000000000000000, 0.2008964009354147484, -0.9796124928211138450 ) ) ;
#9126 = EDGE_CURVE ( 'NONE', #6920, #1141, #29261, .T. ) ;
#9127 = ORIENTED_EDGE ( 'NONE', *, *, #16317, .T. ) ;
#9128 = ORIENTED_EDGE ( 'NONE', *, *, #25696, .T. ) ;
#9129 = ORIENTED_EDGE ( 'NONE', *, *, #17202, .F. ) ;
#9130 = CARTESIAN_POINT ( 'NONE',  ( 51.82407985978792198, 0.5160799604426919984, -4.312591426429957409 ) ) ;
#9131 = ORIENTED_EDGE ( 'NONE', *, *, #28044, .F. ) ;
#9132 =( BOUNDED_CURVE ( )  B_SPLINE_CURVE ( 3, ( #21631, #26501, #2123, #28414 ),
 .UNSPECIFIED., .F., .T. ) 
 B_SPLINE_CURVE_WITH_KNOTS ( ( 4, 4 ),
 ( 5.097689251316671388, 5.213123141636014424 ),
 .UNSPECIFIED. ) 
 CURVE ( )  GEOMETRIC_REPRESENTATION_ITEM ( )  RATIONAL_B_SPLINE_CURVE ( ( 1.000000000000000000, 0.9988898929684264516, 0.9988898929684264516, 1.000000000000000000 ) ) 
 REPRESENTATION_ITEM ( '' )  );
#9133 = CARTESIAN_POINT ( 'NONE',  ( 53.90311770664830959, 7.548181632372875427, 2.049999999999811084 ) ) ;
#9134 = CARTESIAN_POINT ( 'NONE',  ( -55.97085481156723574, -3.673546848079175309, -0.7533615035078069511 ) ) ;
#9136 = CARTESIAN_POINT ( 'NONE',  ( 50.80000000000001847, -3.908336260473454615, -1.238913909466097918 ) ) ;
#9135 = CARTESIAN_POINT ( 'NONE',  ( -44.49999999999996447, 1.600000000000021627, -3.363870538531644971 ) ) ;
#9137 = ORIENTED_EDGE ( 'NONE', *, *, #27340, .T. ) ;
#9138 = ORIENTED_EDGE ( 'NONE', *, *, #14738, .F. ) ;
#9139 = DIRECTION ( 'NONE',  ( 1.000000000000000000, 0.000000000000000000, 0.000000000000000000 ) ) ;
#9140 = ORIENTED_EDGE ( 'NONE', *, *, #13911, .T. ) ;
#9141 = ADVANCED_FACE ( 'NONE', ( #16239 ), #25564, .F. ) ;
#9142 = DIRECTION ( 'NONE',  ( 0.000000000000000000, 0.000000000000000000, 1.000000000000000000 ) ) ;
#9143 = ORIENTED_EDGE ( 'NONE', *, *, #14286, .F. ) ;
#9144 = APPLICATION_CONTEXT ( 'automotive_design' ) ;
#9146 = DIRECTION ( 'NONE',  ( -1.000000000000000000, -3.053848253006669023E-16, 2.042510438544995415E-16 ) ) ;
#9145 = DIRECTION ( 'NONE',  ( -1.000000000000000000, -3.053848253006669023E-16, 2.042510438544995415E-16 ) ) ;
#9147 = VERTEX_POINT ( 'NONE', #28099 ) ;
#9148 = CARTESIAN_POINT ( 'NONE',  ( 52.83066561783866177, 8.351253849600817958, 1.927138392211706686 ) ) ;
#9149 = DIRECTION ( 'NONE',  ( 0.000000000000000000, 1.000000000000000000, 0.000000000000000000 ) ) ;
#9150 = AXIS2_PLACEMENT_3D ( 'NONE', #14778, #10335, #3062 ) ;
#9151 = CARTESIAN_POINT ( 'NONE',  ( -36.00197790576392265, 1.123735532908270329, -5.289358697221547168 ) ) ;
#9152 = CARTESIAN_POINT ( 'NONE',  ( 50.25000000000003553, -1.470078920827295965, -1.320078920827526758 ) ) ;
#9153 = PRODUCT_RELATED_PRODUCT_CATEGORY ( 'part', '', ( #11370 ) ) ;
#9154 = CARTESIAN_POINT ( 'NONE',  ( -57.88452994616205416, 3.117691453623979481, 1.799999999999806422 ) ) ;
#9155 = CARTESIAN_POINT ( 'NONE',  ( -59.14880559183723108, -2.486640902962416799, -0.9502595626627227121 ) ) ;
#9156 = FACE_OUTER_BOUND ( 'NONE', #11740, .T. ) ;
#9157 = CARTESIAN_POINT ( 'NONE',  ( 15.03925126672132961, 0.9159215771349776825, 4.311190327366002606 ) ) ;
#9158 = CARTESIAN_POINT ( 'NONE',  ( -55.61042740578360366, -0.7887156198831609677, 3.845940847736172952 ) ) ;
#9159 = EDGE_CURVE ( 'NONE', #30552, #19284, #12977, .T. ) ;
#9160 = CARTESIAN_POINT ( 'NONE',  ( -35.85663232820584057, 5.086913985776128300, 1.171642053949150331 ) ) ;
#9161 = ADVANCED_FACE ( 'NONE', ( #25733 ), #31206, .F. ) ;
#9162 = AXIS2_PLACEMENT_3D ( 'NONE', #1252, #10615, #27239 ) ;
#9163 = ORIENTED_EDGE ( 'NONE', *, *, #711, .F. ) ;
#9164 = DIRECTION ( 'NONE',  ( -0.9993908270190956511, 0.03489949670250096919, 3.491481338843132961E-15 ) ) ;
#9165 = CARTESIAN_POINT ( 'NONE',  ( -59.66491930162565893, -1.010609427307466612, -3.600000000000221245 ) ) ;
#9166 = CARTESIAN_POINT ( 'NONE',  ( -36.27260443516980359, 0.1928884786867368362, 5.200000000471248107 ) ) ;
#9167 = CARTESIAN_POINT ( 'NONE',  ( 48.34311953187607003, 1.211457450596386209, -3.917546004217189015 ) ) ;
#9168 = VERTEX_POINT ( 'NONE', #13826 ) ;
#9169 = DIRECTION ( 'NONE',  ( 1.000000000000000000, -0.000000000000000000, -0.000000000000000000 ) ) ;
#9170 = VERTEX_POINT ( 'NONE', #14319 ) ;
#9171 = CARTESIAN_POINT ( 'NONE',  ( 51.87453755317506676, 8.609476251808864333, 2.002198665876147032 ) ) ;
#9173 = CARTESIAN_POINT ( 'NONE',  ( 58.73371041428941908, -1.381461519772573698, 1.267950628961816095 ) ) ;
#9172 = CARTESIAN_POINT ( 'NONE',  ( 58.73379417893112731, 0.8670685180646029444, -1.662624490946997602 ) ) ;
#9174 = ORIENTED_EDGE ( 'NONE', *, *, #28595, .F. ) ;
#9175 = ORIENTED_EDGE ( 'NONE', *, *, #28628, .T. ) ;
#9176 = CARTESIAN_POINT ( 'NONE',  ( -59.46761860684627266, -2.377675374897907812, -1.175485268738968081 ) ) ;
#9177 = EDGE_CURVE ( 'NONE', #6393, #28678, #29679, .T. ) ;
#9178 = DIRECTION ( 'NONE',  ( 1.000000000000000000, 0.000000000000000000, 0.000000000000000000 ) ) ;
#9180 = CARTESIAN_POINT ( 'NONE',  ( 58.65000000000003411, -1.394635017527501297, 1.253243060178016455 ) ) ;
#9179 = CARTESIAN_POINT ( 'NONE',  ( -67.36397038208805554, 2.135367159695519934, 0.05319419038626561902 ) ) ;
#9181 = ORIENTED_EDGE ( 'NONE', *, *, #5083, .T. ) ;
#9182 = CARTESIAN_POINT ( 'NONE',  ( -56.12499999999997868, 2.489203624310591056, -2.804704140674918023 ) ) ;
#9183 = CARTESIAN_POINT ( 'NONE',  ( -54.55048689473264290, -3.664629505757012851, 1.761501643209058221 ) ) ;
#9184 = CARTESIAN_POINT ( 'NONE',  ( -36.52679053911622731, 2.412550141807381809, 4.840569432287361806 ) ) ;
#9185 = MECHANICAL_DESIGN_GEOMETRIC_PRESENTATION_REPRESENTATION (  '', ( #1567 ), #30916 ) ;
#9186 = DIRECTION ( 'NONE',  ( 0.000000000000000000, 0.000000000000000000, 1.000000000000000000 ) ) ;
#9187 = LINE ( 'NONE', #18848, #11164 ) ;
#9188 = CARTESIAN_POINT ( 'NONE',  ( -54.48478889579405404, 1.513794642953540270, -4.039462313877657529 ) ) ;
#9190 = VERTEX_POINT ( 'NONE', #12116 ) ;
#9189 = EDGE_CURVE ( 'NONE', #7404, #30905, #9600, .T. ) ;
#9191 = CARTESIAN_POINT ( 'NONE',  ( 57.00108727371435435, -0.7119914823645937529, 1.810661949215600863 ) ) ;
#9192 = APPLICATION_CONTEXT ( 'automotive_design' ) ;
#9193 = CARTESIAN_POINT ( 'NONE',  ( -36.58361892166062290, 3.091683853622045230, -4.437651790015090469 ) ) ;
#9194 = CARTESIAN_POINT ( 'NONE',  ( -39.16187796471576377, 5.407411300779124019, 0.000000000000000000 ) ) ;
#9195 = CARTESIAN_POINT ( 'NONE',  ( 58.75000000000002842, -1.039502773796102897, -1.800471618824325493 ) ) ;
#9196 = CARTESIAN_POINT ( 'NONE',  ( -54.39999999999997726, 8.366749974758487600E-15, -2.213041600731273397E-13 ) ) ;
#9197 = ADVANCED_FACE ( 'NONE', ( #2613 ), #226, .F. ) ;
#9198 = AXIS2_PLACEMENT_3D ( 'NONE', #16832, #12220, #23946 ) ;
#9200 = DIRECTION ( 'NONE',  ( -0.9993908270190953180, 0.03489949670251430575, 3.490905158897711881E-15 ) ) ;
#9199 = DIRECTION ( 'NONE',  ( 1.047444401652940007E-14, 8.673617379884032317E-15, 1.000000000000000000 ) ) ;
#9201 = CARTESIAN_POINT ( 'NONE',  ( 47.12253285714871964, -4.134031523355535143, -2.020495556749611676 ) ) ;
#9203 = DIRECTION ( 'NONE',  ( -1.000000000000000000, -2.586136946169074517E-16, 0.000000000000000000 ) ) ;
#9202 = DIRECTION ( 'NONE',  ( -3.491481338843133355E-15, 0.000000000000000000, -1.000000000000000000 ) ) ;
#9204 = EDGE_LOOP ( 'NONE', ( #19772, #27743, #11329, #4528 ) ) ;
#9205 = AXIS2_PLACEMENT_3D ( 'NONE', #5962, #1500, #15901 ) ;
#9206 = CARTESIAN_POINT ( 'NONE',  ( 61.25000000000004263, -1.499837071477705619, -1.323060376181415254 ) ) ;
#9207 = DIRECTION ( 'NONE',  ( 0.000000000000000000, 1.000000000000000000, 0.000000000000000000 ) ) ;
#9209 = CARTESIAN_POINT ( 'NONE',  ( -36.22909104983326500, 4.895911367891157440, 2.323639554370136917 ) ) ;
#9208 = CARTESIAN_POINT ( 'NONE',  ( 15.81621483022851926, -2.513248512186159633, -4.788125582312100725 ) ) ;
#9210 = CARTESIAN_POINT ( 'NONE',  ( 15.41080140630216988, -5.326563020867278730, 0.9981196555233698975 ) ) ;
#9211 = ORIENTED_EDGE ( 'NONE', *, *, #19459, .T. ) ;
#9212 = ORIENTED_EDGE ( 'NONE', *, *, #24799, .T. ) ;
#9213 = CARTESIAN_POINT ( 'NONE',  ( 51.31572262954152563, 0.7526089581382734428, -1.996089927833914146 ) ) ;
#9214 = CARTESIAN_POINT ( 'NONE',  ( -39.16187796471576377, -5.407411300779158658, 6.622168941172401012E-16 ) ) ;
#9215 = EDGE_CURVE ( 'NONE', #7041, #23567, #17560, .T. ) ;
#9216 = ORIENTED_EDGE ( 'NONE', *, *, #14012, .F. ) ;
#9217 = CARTESIAN_POINT ( 'NONE',  ( -63.82928932188132620, 6.399178848011186396E-16, 2.550935903222500290E-15 ) ) ;
#9218 = ORIENTED_EDGE ( 'NONE', *, *, #7094, .F. ) ;
#9219 = CARTESIAN_POINT ( 'NONE',  ( 58.65263613458530045, 1.873885868625531304, -0.06672978513348816476 ) ) ;
#9220 = ORIENTED_EDGE ( 'NONE', *, *, #21151, .T. ) ;
#9221 = FACE_OUTER_BOUND ( 'NONE', #19280, .T. ) ;
#9222 = ORIENTED_EDGE ( 'NONE', *, *, #26286, .T. ) ;
#9223 =( NAMED_UNIT ( * ) SI_UNIT ( $, .STERADIAN. ) SOLID_ANGLE_UNIT ( ) );
#9224 = EDGE_LOOP ( 'NONE', ( #3865, #309, #29515, #5845 ) ) ;
#9225 = CIRCLE ( 'NONE', #26896, 0.1500000000000001887 ) ;
#9226 = EDGE_CURVE ( 'NONE', #24848, #17885, #19583, .T. ) ;
#9227 = VERTEX_POINT ( 'NONE', #19098 ) ;
#9228 = CARTESIAN_POINT ( 'NONE',  ( -60.37499999999995737, 2.944486372867106905, -1.700000000000201794 ) ) ;
#9229 = CARTESIAN_POINT ( 'NONE',  ( 22.07280086217093640, 8.086143481909140007, -1.950000000000076339 ) ) ;
#9230 = DIRECTION ( 'NONE',  ( 0.000000000000000000, 0.000000000000000000, 1.000000000000000000 ) ) ;
#9231 = CYLINDRICAL_SURFACE ( 'NONE', #2825, 2.000000000000000000 ) ;
#9232 = LINE ( 'NONE', #18894, #6463 ) ;
#9233 = EDGE_CURVE ( 'NONE', #16594, #2692, #28748, .T. ) ;
#9235 = CARTESIAN_POINT ( 'NONE',  ( 50.25000000000000000, 1.470078920828055358, -1.470078920826818125 ) ) ;
#9234 = CARTESIAN_POINT ( 'NONE',  ( -59.96464466094062828, 2.127325729886550933E-15, 5.611146207266455330E-16 ) ) ;
#9236 = EDGE_CURVE ( 'NONE', #2824, #4687, #27346, .T. ) ;
#9237 = CIRCLE ( 'NONE', #18850, 0.1500000000000003830 ) ;
#9238 = EDGE_CURVE ( 'NONE', #3627, #3082, #2056, .T. ) ;
#9239 = CARTESIAN_POINT ( 'NONE',  ( -61.09488783161975789, -2.368993871844102372, -0.8791439831129040927 ) ) ;
#9240 = CARTESIAN_POINT ( 'NONE',  ( -36.52757395963738674, -3.857619034241774880, -3.790808625284033617 ) ) ;
#9241 = CARTESIAN_POINT ( 'NONE',  ( 58.74999999305997989, -1.683452862812675921, -0.9423072185564655978 ) ) ;
#9242 = CARTESIAN_POINT ( 'NONE',  ( 57.03820272507597622, 0.7500000014582769436, -2.490438835250821992 ) ) ;
#9243 = CARTESIAN_POINT ( 'NONE',  ( 50.36635169771310672, 1.250438735127648027, -3.874838289045730910 ) ) ;
#9244 = ORIENTED_EDGE ( 'NONE', *, *, #25507, .T. ) ;
#9246 = CARTESIAN_POINT ( 'NONE',  ( 50.45647961155643912, -1.212999249975888816, 3.917061424767716904 ) ) ;
#9245 = CARTESIAN_POINT ( 'NONE',  ( 51.31802667458096323, -1.005866567096536546, -1.281163073955422504 ) ) ;
#9247 = CARTESIAN_POINT ( 'NONE',  ( 54.24289646986905211, 6.361177601056704489, -2.050000000000189004 ) ) ;
#9248 = CARTESIAN_POINT ( 'NONE',  ( 58.75000000000002132, 6.153735859711025284E-13, 3.111507638930570854E-58 ) ) ;
#9249 = ORIENTED_EDGE ( 'NONE', *, *, #5312, .T. ) ;
#9250 = FACE_OUTER_BOUND ( 'NONE', #28529, .T. ) ;
#9251 = CARTESIAN_POINT ( 'NONE',  ( 61.09423418604053069, -0.6373668173463740150, -1.895722432252557432 ) ) ;
#9252 = CARTESIAN_POINT ( 'NONE',  ( -54.44702994616203995, -2.078460969082631227, -3.600000000000199485 ) ) ;
#9253 = ORIENTED_EDGE ( 'NONE', *, *, #21296, .T. ) ;
#9254 = EDGE_LOOP ( 'NONE', ( #13991, #6101, #25540, #12963 ) ) ;
#9255 = CARTESIAN_POINT ( 'NONE',  ( -35.85663232820584767, 4.383220986679468467, 0.4611378927914916992 ) ) ;
#9256 = ORIENTED_EDGE ( 'NONE', *, *, #25991, .T. ) ;
#9257 = CARTESIAN_POINT ( 'NONE',  ( 50.25000000000002842, -1.039502773796191937, -1.800471618824325493 ) ) ;
#9258 = SHAPE_REPRESENTATION ( 'Eraser Holder', ( #9018 ), #3487 ) ;
#9259 = CARTESIAN_POINT ( 'NONE',  ( -57.50952994616203995, -3.117691453623963938, -1.800000000000215206 ) ) ;
#9260 = VERTEX_POINT ( 'NONE', #1984 ) ;
#9261 = LINE ( 'NONE', #1795, #15581 ) ;
#9262 = DIRECTION ( 'NONE',  ( 1.000000000000000000, 1.047444401652940007E-14, 0.000000000000000000 ) ) ;
#9263 = EDGE_CURVE ( 'NONE', #8618, #29589, #3385, .T. ) ;
#9264 = CARTESIAN_POINT ( 'NONE',  ( 67.94999999999998863, -1.025519176787267142E-28, -4.100000000000712852 ) ) ;
#9265 = ORIENTED_EDGE ( 'NONE', *, *, #28787, .T. ) ;
#9266 = ORIENTED_EDGE ( 'NONE', *, *, #20783, .T. ) ;
#9267 = CARTESIAN_POINT ( 'NONE',  ( 61.25000000000000000, 1.895722432252729739, 0.6373668173479285493 ) ) ;
#9268 = EDGE_CURVE ( 'NONE', #19424, #2253, #30177, .T. ) ;
#9269 = CARTESIAN_POINT ( 'NONE',  ( -62.09999999999997300, -2.667934001961814516, 0.1539767545844223928 ) ) ;
#9270 = CARTESIAN_POINT ( 'NONE',  ( 56.99032252660322939, -0.7964187825544630783, -2.475026498169530687 ) ) ;
#9271 = ORIENTED_EDGE ( 'NONE', *, *, #21690, .F. ) ;
#9272 = DIRECTION ( 'NONE',  ( -1.000000000000000000, -3.053848253006669023E-16, 2.042510438544995415E-16 ) ) ;
#9273 = CARTESIAN_POINT ( 'NONE',  ( 56.99976900444080030, 0.7668859551697654320, 1.738368808232523044 ) ) ;
#9274 = CARTESIAN_POINT ( 'NONE',  ( -55.43749999999997868, 0.7533615035078096156, -3.673546848079177529 ) ) ;
#9275 = CARTESIAN_POINT ( 'NONE',  ( 58.65000000000004121, -1.827485639842249876, 0.4207625006690558500 ) ) ;
#9277 = CARTESIAN_POINT ( 'NONE',  ( 58.74160516400041132, -0.8556415768458849325, 1.668397168087476956 ) ) ;
#9276 = CARTESIAN_POINT ( 'NONE',  ( -36.11122220296840624, -2.734418404389801438, 4.440882220947544923 ) ) ;
#9278 = ADVANCED_FACE ( 'NONE', ( #6891 ), #2289, .F. ) ;
#9279 = CARTESIAN_POINT ( 'NONE',  ( 69.20000000000001705, 0.7500000000000000000, -2.288246715074080839 ) ) ;
#9280 = DIRECTION ( 'NONE',  ( 0.000000000000000000, -1.000000000000000000, -3.491481338843133355E-15 ) ) ;
#9281 = DIRECTION ( 'NONE',  ( 0.9993908270190958731, -0.03489949670250092062, -3.492262959426260213E-15 ) ) ;
#9282 = CIRCLE ( 'NONE', #3211, 3.624999999999996447 ) ;
#9283 = VERTEX_POINT ( 'NONE', #31274 ) ;
#9284 = AXIS2_PLACEMENT_3D ( 'NONE', #15376, #20777, #22691 ) ;
#9285 = DIRECTION ( 'NONE',  ( 0.000000000000000000, 0.000000000000000000, 1.000000000000000000 ) ) ;
#9286 = ORIENTED_EDGE ( 'NONE', *, *, #16418, .F. ) ;
#9287 = CARTESIAN_POINT ( 'NONE',  ( 52.10582242447214441, 8.700707108360601794, 2.049999999999818190 ) ) ;
#9288 = CARTESIAN_POINT ( 'NONE',  ( -55.36042740578360366, -2.936324665650200672, -2.606018187048498191 ) ) ;
#9290 = CARTESIAN_POINT ( 'NONE',  ( -36.04518387042616467, 3.779372851355696117, 3.883777284341113134 ) ) ;
#9289 = DIRECTION ( 'NONE',  ( 1.000000000000000000, 1.047444401652940007E-14, 0.000000000000000000 ) ) ;
#9291 = ORIENTED_EDGE ( 'NONE', *, *, #17860, .T. ) ;
#9292 = DIRECTION ( 'NONE',  ( 0.000000000000000000, 0.000000000000000000, 1.000000000000000000 ) ) ;
#9293 = ORIENTED_EDGE ( 'NONE', *, *, #24282, .T. ) ;
#9294 = LINE ( 'NONE', #6921, #1909 ) ;
#9295 = ORIENTED_EDGE ( 'NONE', *, *, #18332, .T. ) ;
#9297 = FACE_OUTER_BOUND ( 'NONE', #24923, .T. ) ;
#9296 = CARTESIAN_POINT ( 'NONE',  ( 50.37844020491943553, 1.181909706220234613, 3.885998080850100234 ) ) ;
#9298 = ORIENTED_EDGE ( 'NONE', *, *, #5393, .T. ) ;
#9299 = CARTESIAN_POINT ( 'NONE',  ( 57.05000000000001847, 0.6999999999999999556, 0.000000000000000000 ) ) ;
#9300 = EDGE_CURVE ( 'NONE', #11459, #30275, #25634, .T. ) ;
#9301 = CARTESIAN_POINT ( 'NONE',  ( 58.65266784251154775, 1.827264058875769370, -0.4207260278625468697 ) ) ;
#9302 = EDGE_CURVE ( 'NONE', #25704, #8120, #24330, .T. ) ;
#9303 = CARTESIAN_POINT ( 'NONE',  ( -54.46926330052497178, -1.503605180550108944, -3.302415457191589354 ) ) ;
#9304 = CARTESIAN_POINT ( 'NONE',  ( 57.00000000000002132, 0.6820512820512792951, -1.773360101234991770 ) ) ;
#9305 = ADVANCED_FACE ( 'NONE', ( #7523 ), #5410, .T. ) ;
#9307 = CARTESIAN_POINT ( 'NONE',  ( -56.07202994616204705, -4.156921938165296204, -2.141547992439359634E-13 ) ) ;
#9306 = VECTOR ( 'NONE', #14104, 1000.000000000000227 ) ;
#9308 = CARTESIAN_POINT ( 'NONE',  ( 48.40000000000001990, -1.391941090707485618, 3.850000000000022737 ) ) ;
#9309 = AXIS2_PLACEMENT_3D ( 'NONE', #4525, #13693, #21000 ) ;
#9310 = DIRECTION ( 'NONE',  ( 0.000000000000000000, 0.000000000000000000, 1.000000000000000000 ) ) ;
#9311 = CARTESIAN_POINT ( 'NONE',  ( -58.29792740578360366, -1.073804522883506030, -3.225979517392338902 ) ) ;
#9312 = ADVANCED_FACE ( 'NONE', ( #29659 ), #7985, .F. ) ;
#9313 = CARTESIAN_POINT ( 'NONE',  ( -54.49999999999997868, 0.000000000000000000, 4.650000000000000355 ) ) ;
#9314 = ORIENTED_EDGE ( 'NONE', *, *, #19570, .T. ) ;
#9315 = CARTESIAN_POINT ( 'NONE',  ( 60.81555826527926456, -0.6499999999993623101, -1.489337100860648855 ) ) ;
#9316 = CARTESIAN_POINT ( 'NONE',  ( 51.80000000000002558, 4.350000000000017408, 1.550321101314541927 ) ) ;
#9317 = CARTESIAN_POINT ( 'NONE',  ( 48.38952526309124380, 0.7808213810456217097, -4.027268569370236584 ) ) ;
#9318 = ORIENTED_EDGE ( 'NONE', *, *, #22937, .F. ) ;
#9319 = CARTESIAN_POINT ( 'NONE',  ( -59.69999999999997442, -3.237160264815294841, -1.238538609462289219 ) ) ;
#9320 = ORIENTED_EDGE ( 'NONE', *, *, #2508, .F. ) ;
#9321 = SURFACE_STYLE_FILL_AREA ( #11368 ) ;
#9322 = AXIS2_PLACEMENT_3D ( 'NONE', #27528, #25171, #3486 ) ;
#9324 = DIRECTION ( 'NONE',  ( 1.000000000000000000, 1.047444401652940007E-14, 0.000000000000000000 ) ) ;
#9323 = CARTESIAN_POINT ( 'NONE',  ( 58.75000000000000000, 2.008165151418601191, 0.5380862305919300592 ) ) ;
#9325 = ORIENTED_EDGE ( 'NONE', *, *, #29176, .T. ) ;
#9326 = PLANE ( 'NONE',  #23995 ) ;
#9327 = DIRECTION ( 'NONE',  ( 1.000000000000000000, 1.047444401652940007E-14, 0.000000000000000000 ) ) ;
#9329 = CARTESIAN_POINT ( 'NONE',  ( 58.65000000000003411, -1.372267738820216021, 1.278133834460509100 ) ) ;
#9328 = DIRECTION ( 'NONE',  ( -0.04332611568076707997, 0.9990609829735204173, 0.000000000000000000 ) ) ;
#9330 = ORIENTED_EDGE ( 'NONE', *, *, #18277, .F. ) ;
#9331 = CARTESIAN_POINT ( 'NONE',  ( -55.68749999999997868, -4.108500314926507357, 1.367561758111405901 ) ) ;
#9332 = CIRCLE ( 'NONE', #13338, 1.625000000000001332 ) ;
#9333 = DIRECTION ( 'NONE',  ( 1.000000000000000000, 0.000000000000000000, 0.000000000000000000 ) ) ;
#9334 = FACE_OUTER_BOUND ( 'NONE', #7037, .T. ) ;
#9335 = AXIS2_PLACEMENT_3D ( 'NONE', #7244, #16909, #14825 ) ;
#9336 = CARTESIAN_POINT ( 'NONE',  ( 41.48619405471885102, -151.3359592902621955, 2.049999999999835953 ) ) ;
#9337 = EDGE_CURVE ( 'NONE', #24348, #12125, #26625, .T. ) ;
#9338 = LINE ( 'NONE', #19005, #30621 ) ;
#9339 = CARTESIAN_POINT ( 'NONE',  ( -55.81249999999997868, 3.400000000000007905, -1.865662262041272555E-13 ) ) ;
#9340 = CARTESIAN_POINT ( 'NONE',  ( -54.49999516060625382, 1.549196738101655368, -4.063926895246979143 ) ) ;
#9341 = ORIENTED_EDGE ( 'NONE', *, *, #22679, .F. ) ;
#9342 = CARTESIAN_POINT ( 'NONE',  ( -57.18749999999995737, -4.108500314926507357, 1.367561758111402348 ) ) ;
#9343 = CARTESIAN_POINT ( 'NONE',  ( -36.63359589171323449, 2.513248512186358141, -4.788125582311988815 ) ) ;
#9344 = CARTESIAN_POINT ( 'NONE',  ( 48.33000880451179881, 1.140870969100562293, -3.938727831757874664 ) ) ;
#9345 = TOROIDAL_SURFACE ( 'NONE', #31070, 3.250821294908289971, 0.05000000000000000278 ) ;
#9346 = B_SPLINE_CURVE_WITH_KNOTS ( 'NONE', 3,
 ( #3396, #13649, #10814, #20349, #13496, #30588, #23188, #3550, #1470, #23333, #1615, #11130, #13042, #30126, #20956, #22724 ),
 .UNSPECIFIED., .F., .F.,
 ( 4, 3, 3, 3, 3, 4 ),
 ( -2.177409780395868905E-06, 0.000000000000000000, 1.647199373531835971E-05, 5.453032561112356195E-05, 8.914430023005045502E-05, 0.0001239676331529235916 ),
 .UNSPECIFIED. ) ;
#9347 = CARTESIAN_POINT ( 'NONE',  ( 58.66054497608038076, -0.4999999999994944599, -1.807104036850091688 ) ) ;
#9348 = FACE_OUTER_BOUND ( 'NONE', #11422, .T. ) ;
#9349 = EDGE_CURVE ( 'NONE', #556, #10413, #18065, .T. ) ;
#9350 = AXIS2_PLACEMENT_3D ( 'NONE', #23164, #8873, #3527 ) ;
#9352 = DIRECTION ( 'NONE',  ( -3.491481338843133355E-15, -3.491481338843133355E-15, 1.000000000000000000 ) ) ;
#9351 = LINE ( 'NONE', #11723, #3409 ) ;
#9353 = CARTESIAN_POINT ( 'NONE',  ( -62.09999999999998010, -2.720545749060827134, -0.4014110452728690825 ) ) ;
#9355 = CARTESIAN_POINT ( 'NONE',  ( 34.55000000000001847, 3.245314017740485962E-16, 2.649999999999999911 ) ) ;
#9354 = CARTESIAN_POINT ( 'NONE',  ( 64.00000000000001421, 1.163569835200988601E-28, 1.624999999999777955 ) ) ;
#9356 = ORIENTED_EDGE ( 'NONE', *, *, #5617, .F. ) ;
#9357 = CARTESIAN_POINT ( 'NONE',  ( 58.75000000000004974, -1.834410884275049947, 0.3880228184668815250 ) ) ;
#9358 = CARTESIAN_POINT ( 'NONE',  ( 54.19030381964616083, 6.697848500921247172, -2.050000000000189004 ) ) ;
#9360 = CARTESIAN_POINT ( 'NONE',  ( -36.11692583559979397, 5.377732435184220172, 0.5657657035923049360 ) ) ;
#9359 = DIRECTION ( 'NONE',  ( 1.000000000000000000, 0.000000000000000000, 0.000000000000000000 ) ) ;
#9361 = LINE ( 'NONE', #19026, #8452 ) ;
#9362 = VERTEX_POINT ( 'NONE', #24903 ) ;
#9363 = TOROIDAL_SURFACE ( 'NONE', #29068, 1.975000000000001865, 0.1000000000000000056 ) ;
#9364 = ORIENTED_EDGE ( 'NONE', *, *, #27794, .T. ) ;
#9365 = CARTESIAN_POINT ( 'NONE',  ( 50.33036399986577436, -1.366688880095578318, 3.854642372925541682 ) ) ;
#9366 = ORIENTED_EDGE ( 'NONE', *, *, #15692, .F. ) ;
#9367 = CARTESIAN_POINT ( 'NONE',  ( 57.02114944868134216, -0.7500000000000000000, -1.778342400449481442 ) ) ;
#9368 = CIRCLE ( 'NONE', #17448, 0.04999999999999987094 ) ;
#9369 = LINE ( 'NONE', #30, #19479 ) ;
#9370 = ORIENTED_EDGE ( 'NONE', *, *, #18752, .T. ) ;
#9371 = FACE_OUTER_BOUND ( 'NONE', #26619, .T. ) ;
#9372 = ORIENTED_EDGE ( 'NONE', *, *, #14341, .T. ) ;
#9373 = EDGE_CURVE ( 'NONE', #709, #23231, #3224, .T. ) ;
#9374 = CARTESIAN_POINT ( 'NONE',  ( -44.59999999999996589, -1.599999999999981215, -3.363870538531657850 ) ) ;
#9375 = VERTEX_POINT ( 'NONE', #29492 ) ;
#9376 = AXIS2_PLACEMENT_3D ( 'NONE', #24053, #14556, #23756 ) ;
#9377 = B_SPLINE_SURFACE_WITH_KNOTS ( 'NONE', 3, 3, ( 
 ( #19153, #24200, #23885, #14685 ),
 ( #26556, #433, #28793, #19302 ),
 ( #19764, #9782, #26255, #5178 ),
 ( #24033, #21518, #19448, #7104 ),
 ( #2176, #12008, #21689, #271 ),
 ( #7246, #24345, #17226, #16911 ),
 ( #12161, #4868, #14827, #14534 ),
 ( #4563, #14210, #11841, #16765 ),
 ( #31155, #12295, #26409, #129 ),
 ( #29092, #19617, #29254, #7566 ),
 ( #26868, #24486, #2796, #12452 ),
 ( #18001, #22767, #3443, #582 ),
 ( #1199, #3115, #5320, #14985 ),
 ( #29541, #15459, #27338, #12761 ),
 ( #20391, #15303, #24652, #22439 ),
 ( #912, #3589, #5650, #1059 ),
 ( #17366, #5979, #17850, #10564 ),
 ( #24948, #27014, #5497, #2965 ),
 ( #13083, #734, #10709, #7856 ),
 ( #3272, #30014, #8329, #22606 ),
 ( #10857, #25277, #27654, #12610 ),
 ( #17695, #15631, #20545, #17535 ),
 ( #12916, #10393, #20238, #22296 ),
 ( #22911, #10241, #27486, #29870 ),
 ( #8182, #30179, #15148, #20078 ),
 ( #19911, #5806, #25116, #29715 ),
 ( #13227, #27186, #24805, #8030 ),
 ( #23965, #31075, #7034, #2259 ),
 ( #14139, #21445, #23814, #26486 ),
 ( #14296, #1516, #8494, #28874 ),
 ( #2106, #27814, #16527, #18174 ),
 ( #16695, #25426, #24124, #4489 ),
 ( #13371, #28551, #2434, #26337 ),
 ( #30480, #11770, #6271, #7184 ),
 ( #9401, #11924, #9247, #21610 ),
 ( #20705, #4636, #18907, #25575 ),
 ( #3729, #6126, #14448, #15776 ) ),
 .UNSPECIFIED., .F., .F., .F.,
 ( 4, 1, 1, 1, 2, 1, 1, 1, 2, 1, 1, 1, 2, 1, 1, 1, 2, 1, 1, 1, 2, 1, 1, 1, 2, 1, 1, 1, 4 ),
 ( 4, 4 ),
 ( 0.000000000000000000, 0.09793917091270401554, 0.1958783418254080311, 0.2938175127381121299, 0.3917566836508161732, 0.4059014630279186298, 0.4200462424050210863, 0.4341910217821235984, 0.4483358011592260550, 0.4506387114483191292, 0.4529416217374121478, 0.4552445320265053330, 0.4575474423155982961, 0.4619892840416085500, 0.4664311257676187483, 0.4708729674936289467, 0.4753148092196392005, 0.5855976156913508257, 0.6958804221630624509, 0.8061632286347739651, 0.9164460351064855903, 0.9208878768324958441, 0.9253297185585060980, 0.9297715602845164629, 0.9342134020105267167, 0.9365152712282671654, 0.9388171404460077252, 0.9411190096637481739, 0.9434208788814886226 ),
 ( 0.000000000000000000, 1.000000000000000000 ),
 .UNSPECIFIED. ) ;
#9378 = ORIENTED_EDGE ( 'NONE', *, *, #14628, .T. ) ;
#9379 = CARTESIAN_POINT ( 'NONE',  ( -60.99999999999997158, 2.944486372867092250, 1.699999999999795008 ) ) ;
#9380 = CARTESIAN_POINT ( 'NONE',  ( -57.43749999999997158, 3.238593381231836155, 2.874284765127032681 ) ) ;
#9381 = CARTESIAN_POINT ( 'NONE',  ( 54.40000000000001990, 1.734723475976807094E-15, 0.000000000000000000 ) ) ;
#9382 = CARTESIAN_POINT ( 'NONE',  ( 58.75000000000002132, 6.153735859711025284E-13, 3.111507638930570854E-58 ) ) ;
#9383 = AXIS2_PLACEMENT_3D ( 'NONE', #2246, #1613, #13957 ) ;
#9384 = DIRECTION ( 'NONE',  ( 1.000000000000000000, 4.678365685400793326E-16, -1.520093157366863638E-16 ) ) ;
#9385 = AXIS2_PLACEMENT_3D ( 'NONE', #25532, #6698, #21440 ) ;
#9386 = EDGE_CURVE ( 'NONE', #19192, #1382, #11999, .T. ) ;
#9388 = CARTESIAN_POINT ( 'NONE',  ( 51.80000048029754822, 4.021162616303429971, -2.019962949071075542 ) ) ;
#9387 = CARTESIAN_POINT ( 'NONE',  ( -36.52679053911622731, 5.349174094756181219, -0.7986533162260476271 ) ) ;
#9389 = CARTESIAN_POINT ( 'NONE',  ( -54.39999999999999147, 1.399999999999996136, 3.959797974644419849 ) ) ;
#9390 = CARTESIAN_POINT ( 'NONE',  ( 54.31409749668479492, 6.709390224138187975, 2.049999999999810640 ) ) ;
#9391 = AXIS2_PLACEMENT_3D ( 'NONE', #16868, #31099, #1806 ) ;
#9392 = CARTESIAN_POINT ( 'NONE',  ( -36.92398358572908990, -2.945786441214556017, -4.543674732827765794 ) ) ;
#9393 = ORIENTED_EDGE ( 'NONE', *, *, #17901, .F. ) ;
#9394 = CARTESIAN_POINT ( 'NONE',  ( -35.85663232820584057, -3.275050215670988418, 2.949461045525626268 ) ) ;
#9395 = TOROIDAL_SURFACE ( 'NONE', #19532, 2.525000000001608846, 0.1000000000000000056 ) ;
#9396 = CARTESIAN_POINT ( 'NONE',  ( 54.16612471089924696, 6.839395989833654710, 2.049999999999811084 ) ) ;
#9397 = VERTEX_POINT ( 'NONE', #29822 ) ;
#9399 = CARTESIAN_POINT ( 'NONE',  ( 50.36059168657180862, -1.279117291415099000, 3.870058441400160198 ) ) ;
#9398 = LINE ( 'NONE', #17158, #30165 ) ;
#9400 = EDGE_CURVE ( 'NONE', #8546, #14020, #16033, .T. ) ;
#9401 = CARTESIAN_POINT ( 'NONE',  ( 54.16748273148216697, 5.680716993501275347, -2.050000000000189893 ) ) ;
#9402 = CARTESIAN_POINT ( 'NONE',  ( 58.65000000000001990, 6.143261415694495821E-13, 3.111507638930570854E-58 ) ) ;
#9403 = VERTEX_POINT ( 'NONE', #24600 ) ;
#9404 = CARTESIAN_POINT ( 'NONE',  ( 47.00000000000002132, -3.701035844659722240, 1.983438066289691770 ) ) ;
#9405 = CARTESIAN_POINT ( 'NONE',  ( 27.62808879389202232, 5.849836810644521989, 1.424999999999903677 ) ) ;
#9406 = CARTESIAN_POINT ( 'NONE',  ( -59.49999999999997158, 2.944486372867092250, 1.699999999999800115 ) ) ;
#9407 = VERTEX_POINT ( 'NONE', #27444 ) ;
#9408 = VERTEX_POINT ( 'NONE', #5755 ) ;
#9409 = AXIS2_PLACEMENT_3D ( 'NONE', #16950, #12640, #29125 ) ;
#9410 = CARTESIAN_POINT ( 'NONE',  ( 15.22780280894162885, 4.861582133259942928, 2.394243994563265421 ) ) ;
#9411 = ORIENTED_EDGE ( 'NONE', *, *, #4035, .F. ) ;
#9412 = CIRCLE ( 'NONE', #25071, 0.05000000000000012768 ) ;
#9413 = CARTESIAN_POINT ( 'NONE',  ( 51.79853223485510938, 4.577225429117026678, -0.5276849443351092628 ) ) ;
#9414 = CARTESIAN_POINT ( 'NONE',  ( -57.75952994616205416, -4.643455692769894075E-15, 3.599999999999794031 ) ) ;
#9415 = VERTEX_POINT ( 'NONE', #10195 ) ;
#9416 = CARTESIAN_POINT ( 'NONE',  ( -68.01382336603234080, -3.309142602788800391E-16, 2.205138456058669928E-15 ) ) ;
#9417 = EDGE_CURVE ( 'NONE', #11849, #9375, #12476, .T. ) ;
#9418 = DIRECTION ( 'NONE',  ( 1.000000000000000000, 1.786976680021908743E-16, -2.459562394685749209E-16 ) ) ;
#9419 = EDGE_CURVE ( 'NONE', #9917, #8529, #2390, .T. ) ;
#9420 = CIRCLE ( 'NONE', #12913, 4.849999999999999645 ) ;
#9421 = DIRECTION ( 'NONE',  ( 1.000000000000000000, 0.000000000000000000, 0.000000000000000000 ) ) ;
#9422 = ORIENTED_EDGE ( 'NONE', *, *, #5955, .T. ) ;
#9423 = VECTOR ( 'NONE', #30582, 1000.000000000000000 ) ;
#9424 = AXIS2_PLACEMENT_3D ( 'NONE', #21755, #23650, #11606 ) ;
#9425 = CARTESIAN_POINT ( 'NONE',  ( 52.06628335902946247, -0.5434431642975677823, -1.718465885608440713 ) ) ;
#9426 = STYLED_ITEM ( 'NONE', ( #27772 ), #25333 ) ;
#9427 = CARTESIAN_POINT ( 'NONE',  ( 57.05000000000001847, -0.7500000000000000000, 2.489477856900920383 ) ) ;
#9428 = CARTESIAN_POINT ( 'NONE',  ( 58.65000000000002700, -0.8495817349395322626, -1.671477153794241444 ) ) ;
#9429 = ORIENTED_EDGE ( 'NONE', *, *, #1829, .F. ) ;
#9430 = CARTESIAN_POINT ( 'NONE',  ( -54.46614378277664059, -2.255560380866761250, -2.805788190199900889 ) ) ;
#9431 = DIRECTION ( 'NONE',  ( 0.000000000000000000, 0.000000000000000000, 1.000000000000000000 ) ) ;
#9432 = EDGE_CURVE ( 'NONE', #9911, #17666, #10738, .T. ) ;
#9433 = TOROIDAL_SURFACE ( 'NONE', #27105, 0.3000000000000000444, 0.05000000000000000278 ) ;
#9434 = CARTESIAN_POINT ( 'NONE',  ( 56.95000000000001705, 0.000000000000000000, 0.000000000000000000 ) ) ;
#9436 = DIRECTION ( 'NONE',  ( -1.000000000000000000, -1.047444401652940007E-14, 0.000000000000000000 ) ) ;
#9435 = CARTESIAN_POINT ( 'NONE',  ( 58.75000000000002132, -0.5933779550749339604, -1.867062706145875772 ) ) ;
#9437 = TOROIDAL_SURFACE ( 'NONE', #26595, 2.525000000001608846, 0.1000000000000000056 ) ;
#9438 = CARTESIAN_POINT ( 'NONE',  ( 58.73794315689227830, -0.4999999999993849364, 1.843373610711628974 ) ) ;
#9439 = CARTESIAN_POINT ( 'NONE',  ( 46.92031786090804957, -4.254331549871407603, 1.021189760102710231 ) ) ;
#9440 = CONICAL_SURFACE ( 'NONE', #20065, 1.487500000000000933, 0.7853981633974481680 ) ;
#9441 = EDGE_LOOP ( 'NONE', ( #16704, #8828, #23110, #663, #15315, #5377, #7108, #18670 ) ) ;
#9443 = EDGE_CURVE ( 'NONE', #24785, #4566, #6435, .T. ) ;
#9442 = AXIS2_PLACEMENT_3D ( 'NONE', #29666, #27295, #16043 ) ;
#9444 = AXIS2_PLACEMENT_3D ( 'NONE', #19439, #24190, #2497 ) ;
#9445 = ORIENTED_EDGE ( 'NONE', *, *, #19784, .F. ) ;
#9446 = CIRCLE ( 'NONE', #24085, 1.375000000000001332 ) ;
#9447 = CARTESIAN_POINT ( 'NONE',  ( -59.09999999999998010, -2.331118226142294247, 1.260312586522342349 ) ) ;
#9448 =( BOUNDED_CURVE ( )  B_SPLINE_CURVE ( 2, ( #18382, #2060, #4118, #25654, #19016, #21400, #31026, #28670, #3961 ),
 .UNSPECIFIED., .F., .T. ) 
 B_SPLINE_CURVE_WITH_KNOTS ( ( 3, 2, 2, 2, 3 ),
 ( 0.1388888888888888951, 0.1481481481481481399, 0.1666666666666666574, 0.1851851851851851749, 0.1944444444444444475 ),
 .UNSPECIFIED. ) 
 CURVE ( )  GEOMETRIC_REPRESENTATION_ITEM ( )  RATIONAL_B_SPLINE_CURVE ( ( 0.9330127018922192983, 0.9330127018922194093, 1.000000000000000000, 0.8660254037844387076, 1.000000000000000000, 0.8660254037844387076, 1.000000000000000000, 0.9330127018922191873, 0.9330127018922192983 ) ) 
 REPRESENTATION_ITEM ( '' )  );
#9449 = ORIENTED_EDGE ( 'NONE', *, *, #22977, .T. ) ;
#9450 = CIRCLE ( 'NONE', #4863, 0.1000000000000000472 ) ;
#9451 = EDGE_CURVE ( 'NONE', #8146, #24802, #7713, .T. ) ;
#9452 = DIRECTION ( 'NONE',  ( 1.000000000000000000, 0.000000000000000000, 0.000000000000000000 ) ) ;
#9453 = CARTESIAN_POINT ( 'NONE',  ( -55.17292740578361077, 2.256877952708269408, -2.542931754211925632 ) ) ;
#9454 = CARTESIAN_POINT ( 'NONE',  ( -36.58361892166060869, 3.265074799938700867, 4.311675893545017679 ) ) ;
#9455 = ORIENTED_EDGE ( 'NONE', *, *, #11244, .F. ) ;
#9456 = ORIENTED_EDGE ( 'NONE', *, *, #14437, .T. ) ;
#9457 = FACE_OUTER_BOUND ( 'NONE', #1741, .T. ) ;
#9458 = VERTEX_POINT ( 'NONE', #8592 ) ;
#9459 = FACE_OUTER_BOUND ( 'NONE', #23933, .T. ) ;
#9460 = ORIENTED_EDGE ( 'NONE', *, *, #26462, .F. ) ;
#9462 = PLANE ( 'NONE',  #886 ) ;
#9461 = CARTESIAN_POINT ( 'NONE',  ( -67.36397038208805554, -4.395200732636863594E-16, 3.272898199462452353E-15 ) ) ;
#9463 = ADVANCED_FACE ( 'NONE', ( #20494 ), #10478, .T. ) ;
#9464 = ORIENTED_EDGE ( 'NONE', *, *, #16414, .F. ) ;
#9465 = DIRECTION ( 'NONE',  ( -1.000000000000000000, 0.000000000000000000, 0.000000000000000000 ) ) ;
#9466 = ADVANCED_FACE ( 'NONE', ( #20801 ), #18583, .T. ) ;
#9467 = AXIS2_PLACEMENT_3D ( 'NONE', #27879, #10778, #25493 ) ;
#9468 = CARTESIAN_POINT ( 'NONE',  ( -59.29999999999997584, 2.330309927981285032E-15, 4.253626757584724400E-16 ) ) ;
#9469 = AXIS2_PLACEMENT_3D ( 'NONE', #14405, #9359, #31208 ) ;
#9470 = CARTESIAN_POINT ( 'NONE',  ( 58.75000000000002132, 6.153735859711025284E-13, 3.111507638930570854E-58 ) ) ;
#9471 = AXIS2_PLACEMENT_3D ( 'NONE', #11726, #3967, #13607 ) ;
#9472 = CARTESIAN_POINT ( 'NONE',  ( 61.25000000000003553, -1.106298139389688462, -1.666164585742599513 ) ) ;
#9473 = CARTESIAN_POINT ( 'NONE',  ( -57.13452994616205416, 3.117691453623979481, 1.799999999999809086 ) ) ;
#9474 = CIRCLE ( 'NONE', #27645, 0.04999999999999988481 ) ;
#9475 = CARTESIAN_POINT ( 'NONE',  ( 51.81792662072884781, 0.6442955068957180176, 4.286808768127969849 ) ) ;
#9476 = PRESENTATION_LAYER_ASSIGNMENT (  '', '', ( #17530 ) ) ;
#9478 = AXIS2_PLACEMENT_3D ( 'NONE', #22719, #852, #20193 ) ;
#9477 = CARTESIAN_POINT ( 'NONE',  ( -58.68749999999998579, 1.962990915244717138, 3.399999999999802291 ) ) ;
#9479 = DIRECTION ( 'NONE',  ( 0.000000000000000000, -1.000000000000000000, 0.000000000000000000 ) ) ;
#9480 = CARTESIAN_POINT ( 'NONE',  ( -59.69999999999997442, -3.399999999999991473, -2.235080921937235780E-13 ) ) ;
#9481 = VERTEX_POINT ( 'NONE', #3999 ) ;
#9482 = DIRECTION ( 'NONE',  ( 1.000000000000000000, -1.219044193948983948E-29, 3.491481338843133355E-15 ) ) ;
#9483 = ORIENTED_EDGE ( 'NONE', *, *, #12450, .F. ) ;
#9484 = ADVANCED_FACE ( 'NONE', ( #10666 ), #15871, .T. ) ;
#9485 = DIRECTION ( 'NONE',  ( 1.000000000000000000, 1.047444401652940007E-14, 0.000000000000000000 ) ) ;
#9486 = AXIS2_PLACEMENT_3D ( 'NONE', #9135, #8962, #4208 ) ;
#9487 = CARTESIAN_POINT ( 'NONE',  ( -36.43290890416756866, -0.4851603899458980518, 5.391500295856537228 ) ) ;
#9488 = DIRECTION ( 'NONE',  ( 0.000000000000000000, 0.000000000000000000, 1.000000000000000000 ) ) ;
#9489 = EDGE_CURVE ( 'NONE', #1785, #10286, #23619, .T. ) ;
#9490 = VERTEX_POINT ( 'NONE', #1611 ) ;
#9491 = CARTESIAN_POINT ( 'NONE',  ( -54.48779575765000516, 1.517266520141196118, 4.041867453639656382 ) ) ;
#9492 = CIRCLE ( 'NONE', #29694, 0.05000000000000012768 ) ;
#9493 = ORIENTED_EDGE ( 'NONE', *, *, #29244, .T. ) ;
#9494 = EDGE_CURVE ( 'NONE', #10675, #10424, #20951, .T. ) ;
#9495 = CARTESIAN_POINT ( 'NONE',  ( 15.76623786017542272, 0.1071614981650652471, -5.407381887150171984 ) ) ;
#9497 = DIRECTION ( 'NONE',  ( 0.000000000000000000, 0.000000000000000000, 1.000000000000000000 ) ) ;
#9496 = CARTESIAN_POINT ( 'NONE',  ( 58.74999981196284438, 1.050519579373341506, -1.649561145037804266 ) ) ;
#9498 = ORIENTED_EDGE ( 'NONE', *, *, #25165, .T. ) ;
#9499 = ORIENTED_EDGE ( 'NONE', *, *, #8510, .T. ) ;
#9500 = CARTESIAN_POINT ( 'NONE',  ( 50.78793970012935688, -0.4223115601891289650, 0.9680023493207207119 ) ) ;
#9501 = AXIS2_PLACEMENT_3D ( 'NONE', #3129, #20719, #15162 ) ;
#9502 = CARTESIAN_POINT ( 'NONE',  ( -44.59999999999998721, -1.600000000000004530, 3.363870538531271936 ) ) ;
#9503 = AXIS2_PLACEMENT_3D ( 'NONE', #7138, #9525, #10387 ) ;
#9505 = LINE ( 'NONE', #28484, #16582 ) ;
#9504 = LINE ( 'NONE', #141, #2404 ) ;
#9506 = AXIS2_PLACEMENT_3D ( 'NONE', #28383, #19369, #16986 ) ;
#9507 = EDGE_LOOP ( 'NONE', ( #297, #8512, #21483, #28222, #1135, #1598, #23229 ) ) ;
#9508 = CARTESIAN_POINT ( 'NONE',  ( -55.62499999999997158, -3.673546848079173976, -0.7533615035078066180 ) ) ;
#9509 = CYLINDRICAL_SURFACE ( 'NONE', #632, 0.1000000000000000472 ) ;
#9510 = CARTESIAN_POINT ( 'NONE',  ( 51.80000000000002558, -3.637377585518695611, 2.099877210782855830 ) ) ;
#9511 = DIRECTION ( 'NONE',  ( 1.000000000000000000, 1.047444401652940007E-14, 0.000000000000000000 ) ) ;
#9512 = CONTEXT_DEPENDENT_SHAPE_REPRESENTATION ( #29016, #27779 ) ;
#9513 = CARTESIAN_POINT ( 'NONE',  ( 50.56948141424500420, 0.1019060742265078534, -1.190674082256531818 ) ) ;
#9514 = CARTESIAN_POINT ( 'NONE',  ( 51.70000000000003837, 6.982261990806648555E-14, 4.499999999999857003 ) ) ;
#9515 = CARTESIAN_POINT ( 'NONE',  ( 51.25000000000002842, -1.099999999999462963, 1.196087371390569087 ) ) ;
#9516 = AXIS2_PLACEMENT_3D ( 'NONE', #17381, #24360, #29557 ) ;
#9517 = VERTEX_POINT ( 'NONE', #23013 ) ;
#9518 = AXIS2_PLACEMENT_3D ( 'NONE', #9011, #3778, #6637 ) ;
#9519 = LINE ( 'NONE', #25956, #24616 ) ;
#9520 = VECTOR ( 'NONE', #14728, 1000.000000000000000 ) ;
#9521 = CARTESIAN_POINT ( 'NONE',  ( 16.10624235918717773, -3.309998894527983904, 4.278958290368447770 ) ) ;
#9522 = LINE ( 'NONE', #7843, #26788 ) ;
#9523 = CARTESIAN_POINT ( 'NONE',  ( 24.97556103306002839, 5.351466982482016022, -1.950000000000086553 ) ) ;
#9524 = DIRECTION ( 'NONE',  ( 1.000000000000000000, -0.000000000000000000, -0.000000000000000000 ) ) ;
#9526 = CYLINDRICAL_SURFACE ( 'NONE', #27584, 0.9999999999999997780 ) ;
#9525 = DIRECTION ( 'NONE',  ( -3.491481338843133355E-15, -3.491481338843133355E-15, 1.000000000000000000 ) ) ;
#9527 = EDGE_CURVE ( 'NONE', #26147, #1670, #20703, .T. ) ;
#9528 = CARTESIAN_POINT ( 'NONE',  ( -62.06710100716626499, -2.624587610216423172, -0.3274367013645040903 ) ) ;
#9530 = LINE ( 'NONE', #6811, #7418 ) ;
#9529 = CARTESIAN_POINT ( 'NONE',  ( 50.91813586553376325, -3.908336260473453727, 1.238913909465742202 ) ) ;
#9531 = ADVANCED_FACE ( 'NONE', ( #8734 ), #25227, .T. ) ;
#9532 = ORIENTED_EDGE ( 'NONE', *, *, #2584, .F. ) ;
#9533 = CARTESIAN_POINT ( 'NONE',  ( 58.72204580543434105, -1.805265037611284873, 0.5070891929461229797 ) ) ;
#9534 = UNCERTAINTY_MEASURE_WITH_UNIT (LENGTH_MEASURE( 1.000000000000000082E-05 ), #24603, 'distance_accuracy_value', 'NONE');
#9535 = CARTESIAN_POINT ( 'NONE',  ( 33.47623932017462778, -5.407411300779132013, 6.622168941172392137E-16 ) ) ;
#9537 = CARTESIAN_POINT ( 'NONE',  ( -36.22818246778579976, 5.326563020867125964, 0.9981196555233160517 ) ) ;
#9536 = CARTESIAN_POINT ( 'NONE',  ( -59.15835481156722864, -0.7533615035078041755, 3.673546848079178861 ) ) ;
#9538 = CARTESIAN_POINT ( 'NONE',  ( 15.03925126672133139, -4.804073783693453947, 2.042134687550334338 ) ) ;
#9539 = VERTEX_POINT ( 'NONE', #18123 ) ;
#9540 = ORIENTED_EDGE ( 'NONE', *, *, #31164, .T. ) ;
#9541 = CARTESIAN_POINT ( 'NONE',  ( 51.43640408064043612, -0.9729063086537432792, -1.446762274037361573 ) ) ;
#9542 = CIRCLE ( 'NONE', #27213, 2.374999999999998668 ) ;
#9543 = ORIENTED_EDGE ( 'NONE', *, *, #14805, .T. ) ;
#9544 = FACE_OUTER_BOUND ( 'NONE', #3111, .T. ) ;
#9545 = DIRECTION ( 'NONE',  ( 1.000000000000000000, -0.000000000000000000, -0.000000000000000000 ) ) ;
#9546 = ORIENTED_EDGE ( 'NONE', *, *, #14078, .F. ) ;
#9547 = CARTESIAN_POINT ( 'NONE',  ( 58.74999981196283017, 1.953821646385494715, 0.08499607039126413910 ) ) ;
#9548 = ORIENTED_EDGE ( 'NONE', *, *, #30619, .T. ) ;
#9549 = DIRECTION ( 'NONE',  ( 0.000000000000000000, 0.000000000000000000, 1.000000000000000000 ) ) ;
#9550 = EDGE_CURVE ( 'NONE', #5992, #3096, #15580, .T. ) ;
#9551 = CARTESIAN_POINT ( 'NONE',  ( 51.30615523877534656, -3.992023072242621318, -1.294577227648917805 ) ) ;
#9552 = ORIENTED_EDGE ( 'NONE', *, *, #24207, .F. ) ;
#9553 = SURFACE_STYLE_USAGE ( .BOTH. , #18733 ) ;
#9554 = ORIENTED_EDGE ( 'NONE', *, *, #2235, .T. ) ;
#9555 = ORIENTED_EDGE ( 'NONE', *, *, #18781, .F. ) ;
#9556 = CARTESIAN_POINT ( 'NONE',  ( -54.57202994616205416, -4.156921938165296204, -2.089175772356712570E-13 ) ) ;
#9557 = CARTESIAN_POINT ( 'NONE',  ( 53.66601923242428995, 4.681126589747570677, -2.050000000000186784 ) ) ;
#9558 = DIRECTION ( 'NONE',  ( 1.000000000000000000, 0.000000000000000000, 4.738179285253022937E-16 ) ) ;
#9559 = PRODUCT_RELATED_PRODUCT_CATEGORY ( 'part', '', ( #15367 ) ) ;
#9560 = DIRECTION ( 'NONE',  ( -1.000000000000000000, 0.000000000000000000, 1.047444401652940007E-14 ) ) ;
#9561 = CIRCLE ( 'NONE', #27726, 4.600000000000036948 ) ;
#9562 = CARTESIAN_POINT ( 'NONE',  ( -58.22085481156723574, -3.673546848079176197, -0.7533615035078065070 ) ) ;
#9563 = AXIS2_PLACEMENT_3D ( 'NONE', #11117, #8271, #13634 ) ;
#9565 = CARTESIAN_POINT ( 'NONE',  ( -57.68749999999996447, 0.7533615035078072841, -3.673546848079177085 ) ) ;
#9564 = LINE ( 'NONE', #12225, #2368 ) ;
#9566 = CARTESIAN_POINT ( 'NONE',  ( 51.80000000000003268, 2.428612866367529932E-14, 4.099999999999811351 ) ) ;
#9567 = CARTESIAN_POINT ( 'NONE',  ( 51.80000000000001847, 2.428612866367529932E-14, -1.808587333520743709E-13 ) ) ;
#9568 = CARTESIAN_POINT ( 'NONE',  ( -35.85663232820584057, -4.018128179617548312, -3.618665901676662244 ) ) ;
#9569 = EDGE_CURVE ( 'NONE', #8368, #11984, #6538, .T. ) ;
#9570 = VERTEX_POINT ( 'NONE', #1156 ) ;
#9571 = CARTESIAN_POINT ( 'NONE',  ( -62.09999999999997300, 1.168016602258162478E-15, 2.197726754101795588E-15 ) ) ;
#9572 = CARTESIAN_POINT ( 'NONE',  ( 53.46818089146800901, 8.044765782148928679, 2.049999999999813749 ) ) ;
#9574 = CARTESIAN_POINT ( 'NONE',  ( 48.40000000000001279, -0.7619326981554292999, -3.939508824314740032 ) ) ;
#9573 = CARTESIAN_POINT ( 'NONE',  ( 48.44629147628577215, -1.309359793766436519, 3.864871860988134955 ) ) ;
#9575 = CARTESIAN_POINT ( 'NONE',  ( 58.45000000000001705, 0.8000000000000000444, -2.421260002560649660 ) ) ;
#9576 = CARTESIAN_POINT ( 'NONE',  ( 51.58656643569684519, -3.755435527867144962, -1.648753881545417022 ) ) ;
#9577 = ORIENTED_EDGE ( 'NONE', *, *, #21026, .T. ) ;
#9578 = CARTESIAN_POINT ( 'NONE',  ( 60.75000000000001421, 0.5000000000006329381, -1.554802467931481580 ) ) ;
#9579 = CARTESIAN_POINT ( 'NONE',  ( -60.62499999999995737, -2.944486372867076707, -1.700000000000225775 ) ) ;
#9580 = ORIENTED_EDGE ( 'NONE', *, *, #11524, .F. ) ;
#9581 = EDGE_LOOP ( 'NONE', ( #22919, #3498, #7972, #9874 ) ) ;
#9582 = CARTESIAN_POINT ( 'NONE',  ( 15.68751737981905592, 5.024465639092023928, 2.007392901578218147 ) ) ;
#9583 = MECHANICAL_DESIGN_GEOMETRIC_PRESENTATION_REPRESENTATION (  '', ( #21721 ), #27250 ) ;
#9584 = ORIENTED_EDGE ( 'NONE', *, *, #14044, .F. ) ;
#9585 = CARTESIAN_POINT ( 'NONE',  ( -62.09999999999997300, 1.168016602258162478E-15, 2.197726754101795588E-15 ) ) ;
#9586 = AXIS2_PLACEMENT_3D ( 'NONE', #1479, #20506, #13800 ) ;
#9587 = EDGE_CURVE ( 'NONE', #7615, #11967, #27911, .T. ) ;
#9588 = CARTESIAN_POINT ( 'NONE',  ( -58.50952994616205416, -4.643455692769885398E-15, 3.599999999999791367 ) ) ;
#9589 = ORIENTED_EDGE ( 'NONE', *, *, #17593, .F. ) ;
#9590 = DIRECTION ( 'NONE',  ( 1.168655815394902336E-14, 0.000000000000000000, 1.000000000000000000 ) ) ;
#9591 = DIRECTION ( 'NONE',  ( 1.000000000000000000, 3.053848253006669023E-16, -2.042510438544995415E-16 ) ) ;
#9592 = CARTESIAN_POINT ( 'NONE',  ( 33.97298909694674762, 8.288184271125778935, 2.049999999999881251 ) ) ;
#9593 = VERTEX_POINT ( 'NONE', #6224 ) ;
#9594 = CARTESIAN_POINT ( 'NONE',  ( 52.20711756518984004, -0.4999999999994533817, -1.807104036850122109 ) ) ;
#9595 = CARTESIAN_POINT ( 'NONE',  ( -62.09999999999997300, -2.696106776338097699, 0.1686925953295615732 ) ) ;
#9596 = CARTESIAN_POINT ( 'NONE',  ( 58.65266784251154064, -0.8793208749730293539, -1.656109637135622981 ) ) ;
#9597 = VERTEX_POINT ( 'NONE', #4152 ) ;
#9598 = AXIS2_PLACEMENT_3D ( 'NONE', #18164, #27803, #15449 ) ;
#9599 = CARTESIAN_POINT ( 'NONE',  ( -59.19999999999997442, -3.222669219888746550, 1.250136525132528931 ) ) ;
#9600 = LINE ( 'NONE', #21471, #17050 ) ;
#9601 = VECTOR ( 'NONE', #9327, 1000.000000000000000 ) ;
#9603 = CARTESIAN_POINT ( 'NONE',  ( 58.74999999999980815, -0.8495817349408062436, 1.671477153793593740 ) ) ;
#9602 = CARTESIAN_POINT ( 'NONE',  ( -36.68133364217528225, -2.563573972737447360, 4.761506352252311558 ) ) ;
#9604 =( GEOMETRIC_REPRESENTATION_CONTEXT ( 3 ) GLOBAL_UNCERTAINTY_ASSIGNED_CONTEXT ( ( #26602 ) ) GLOBAL_UNIT_ASSIGNED_CONTEXT ( ( #7468, #4461, #28695 ) ) REPRESENTATION_CONTEXT ( 'NONE', 'WORKASPACE' ) );
#9605 = CARTESIAN_POINT ( 'NONE',  ( -59.60604010435355349, 3.187076279294280390, -1.184290838417780600 ) ) ;
#9606 = DIRECTION ( 'NONE',  ( -1.000000000000000000, 1.219044193948983948E-29, -3.491481338843133355E-15 ) ) ;
#9607 = CIRCLE ( 'NONE', #13101, 0.1000000000000021150 ) ;
#9608 = EDGE_CURVE ( 'NONE', #13576, #17229, #20621, .T. ) ;
#9609 = CARTESIAN_POINT ( 'NONE',  ( 53.87827693845233057, 5.944250707180074755, 2.049999999999811973 ) ) ;
#9610 = ORIENTED_EDGE ( 'NONE', *, *, #13915, .T. ) ;
#9611 = ADVANCED_FACE ( 'NONE', ( #25997 ), #11501, .T. ) ;
#9612 = CIRCLE ( 'NONE', #13126, 1.000000000000000000 ) ;
#9613 = CARTESIAN_POINT ( 'NONE',  ( 58.71182503183384682, 0.5000000000006149525, -1.820794158165981003 ) ) ;
#9614 = EDGE_LOOP ( 'NONE', ( #6709, #21412, #26340, #7202 ) ) ;
#9615 = DIRECTION ( 'NONE',  ( 0.000000000000000000, 0.000000000000000000, -1.000000000000000000 ) ) ;
#9616 = CARTESIAN_POINT ( 'NONE',  ( -55.54792740578360366, -2.256877952708263191, 2.542931754211924300 ) ) ;
#9618 = CARTESIAN_POINT ( 'NONE',  ( -35.85663232820596846, 2.525801270006243548, 4.794550352686347772 ) ) ;
#9617 = CARTESIAN_POINT ( 'NONE',  ( 48.50000000000002132, -1.391941090707485396, 3.850000000000022737 ) ) ;
#9619 = ORIENTED_EDGE ( 'NONE', *, *, #5551, .F. ) ;
#9620 = EDGE_LOOP ( 'NONE', ( #16962, #17829, #7459, #25452 ) ) ;
#9621 = DIRECTION ( 'NONE',  ( -0.000000000000000000, -0.9333474217026306308, 0.3589743589743588648 ) ) ;
#9622 = ORIENTED_EDGE ( 'NONE', *, *, #12914, .F. ) ;
#9623 = DIRECTION ( 'NONE',  ( -1.144559819201192819E-14, 0.000000000000000000, -1.000000000000000000 ) ) ;
#9624 = EDGE_CURVE ( 'NONE', #7081, #28342, #26325, .T. ) ;
#9625 = ORIENTED_EDGE ( 'NONE', *, *, #5209, .T. ) ;
#9626 = CARTESIAN_POINT ( 'NONE',  ( 47.00000000000002132, 2.428612866367529932E-14, 0.000000000000000000 ) ) ;
#9627 = ORIENTED_EDGE ( 'NONE', *, *, #25003, .F. ) ;
#9628 = CARTESIAN_POINT ( 'NONE',  ( -59.53056271719990633, 2.463209972446164908, -1.140713948626884244 ) ) ;
#9629 = CARTESIAN_POINT ( 'NONE',  ( 68.04999999999998295, 4.837354856632045057E-16, -3.950000000000713385 ) ) ;
#9630 = VECTOR ( 'NONE', #12617, 1000.000000000000000 ) ;
#9631 = CIRCLE ( 'NONE', #27299, 3.624999999999996447 ) ;
#9632 = DIRECTION ( 'NONE',  ( 1.000000000000000000, 1.047444401652940007E-14, 0.000000000000000000 ) ) ;
#9633 = CARTESIAN_POINT ( 'NONE',  ( -55.76905989232411542, 2.023778652682505897E-14, -3.400000000000197975 ) ) ;
#9634 = EDGE_CURVE ( 'NONE', #14659, #24201, #26675, .T. ) ;
#9635 = CARTESIAN_POINT ( 'NONE',  ( -59.09999999999997300, -2.465712773623968790, -0.9709585562669303949 ) ) ;
#9636 = CIRCLE ( 'NONE', #10126, 0.1000000000000001166 ) ;
#9637 = B_SPLINE_CURVE_WITH_KNOTS ( 'NONE', 3,
 ( #14416, #2228, #2078, #24089, #28368, #28520, #4457, #31045, #6672, #12064, #26308, #4610, #25981 ),
 .UNSPECIFIED., .F., .F.,
 ( 4, 3, 3, 3, 4 ),
 ( 0.000000000000000000, 3.315084464040651867E-05, 6.626473632996253958E-05, 9.991171812043499688E-05, 0.0001104636331268446688 ),
 .UNSPECIFIED. ) ;
#9638 = CARTESIAN_POINT ( 'NONE',  ( -44.49999999999997868, -0.7497673985144445163, -0.01867747640535983439 ) ) ;
#9639 = FACE_OUTER_BOUND ( 'NONE', #19306, .T. ) ;
#9640 = ADVANCED_FACE ( 'NONE', ( #4774 ), #4504, .T. ) ;
#9641 =( BOUNDED_SURFACE ( )  B_SPLINE_SURFACE ( 3, 2, ( 
 ( #23783, #26739, #22150 ),
 ( #438, #10100, #28517 ),
 ( #9786, #6822, #2516 ),
 ( #16486, #16332, #2664 ),
 ( #12167, #4283, #26144 ),
 ( #21847, #21103, #19769 ),
 ( #14691, #19454, #13930 ),
 ( #29401, #29100, #23626 ),
 ( #7414, #5033, #16176 ),
 ( #12301, #21986, #30741 ),
 ( #25824, #279, #18721 ),
 ( #28364, #6669, #30898 ),
 ( #25282, #27345, #20244 ),
 ( #24955, #10714, #8188 ),
 ( #27020, #15309, #7712 ),
 ( #5328, #15466, #20553 ) ),
 .UNSPECIFIED., .F., .F., .F. ) 
 B_SPLINE_SURFACE_WITH_KNOTS ( ( 4, 2, 2, 2, 2, 2, 2, 4 ),
 ( 3, 3 ),
 ( 0.001780502285214263011, 0.002558945925323794120, 0.002753556835351177005, 0.002948167745378559457, 0.003337389565433324795, 0.003726611385488090566, 0.004115833205542856338, 0.004894276845652387013 ),
 ( 0.000000000000000000, 1.000000000000000000 ),
 .UNSPECIFIED. ) 
 GEOMETRIC_REPRESENTATION_ITEM ( )  RATIONAL_B_SPLINE_SURFACE ( (
 ( 1.000000000000000000, 0.9418517008537224955, 1.000000000000000000),
 ( 1.000000000000000000, 0.9417987965884832002, 1.000000000000000000),
 ( 1.000000000000000000, 0.9418198861734355942, 1.000000000000000000),
 ( 1.000000000000000000, 0.9434060303845482887, 1.000000000000000000),
 ( 1.000000000000000000, 0.9437939819948070186, 1.000000000000000000),
 ( 1.000000000000000000, 0.9445989566712852392, 1.000000000000000000),
 ( 1.000000000000000000, 0.9450169930049781009, 1.000000000000000000),
 ( 1.000000000000000000, 0.9461610507673672288, 1.000000000000000000),
 ( 1.000000000000000000, 0.9467217966427039499, 1.000000000000000000),
 ( 1.000000000000000000, 0.9467345476124477965, 1.000000000000000000),
 ( 1.000000000000000000, 0.9461964028052843867, 1.000000000000000000),
 ( 1.000000000000000000, 0.9446801822473894772, 1.000000000000000000),
 ( 1.000000000000000000, 0.9437582546537259809, 1.000000000000000000),
 ( 1.000000000000000000, 0.9418129560294213887, 1.000000000000000000),
 ( 1.000000000000000000, 0.9418016889778539902, 1.000000000000000000),
 ( 1.000000000000000000, 0.9418517008537212742, 1.000000000000000000) ) ) 
 REPRESENTATION_ITEM ( '' )  SURFACE ( )  );
#9642 = VECTOR ( 'NONE', #20055, 1000.000000000000000 ) ;
#9643 = CARTESIAN_POINT ( 'NONE',  ( -60.49999999999997868, 1.656632322739229403E-15, 1.870925083934595927E-15 ) ) ;
#9644 = ADVANCED_FACE ( 'NONE', ( #13951 ), #16683, .T. ) ;
#9645 = ORIENTED_EDGE ( 'NONE', *, *, #24321, .F. ) ;
#9646 = EDGE_CURVE ( 'NONE', #489, #21323, #19218, .T. ) ;
#9647 = CARTESIAN_POINT ( 'NONE',  ( 61.25000000000000000, 2.008165151418627836, 0.5380862305919300592 ) ) ;
#9648 = CARTESIAN_POINT ( 'NONE',  ( -54.45996984137642727, 1.500763111530253990, 3.300586169551324556 ) ) ;
#9649 = CARTESIAN_POINT ( 'NONE',  ( 22.07280086217093640, 8.086143481909148889, -1.950000000000076339 ) ) ;
#9650 = ORIENTED_EDGE ( 'NONE', *, *, #14084, .F. ) ;
#9651 = CARTESIAN_POINT ( 'NONE',  ( -54.49131719536980967, 1.521332553059528081, 4.044684194243341580 ) ) ;
#9652 = ORIENTED_EDGE ( 'NONE', *, *, #14612, .F. ) ;
#9654 = CARTESIAN_POINT ( 'NONE',  ( -61.34573544359366082, -2.573773108005611210, -0.5888079060821346244 ) ) ;
#9653 = DIRECTION ( 'NONE',  ( -1.000000000000000000, 0.000000000000000000, 3.435095992031092083E-15 ) ) ;
#9655 = ORIENTED_EDGE ( 'NONE', *, *, #14738, .T. ) ;
#9656 = DIRECTION ( 'NONE',  ( 9.337490065241209392E-15, -0.8914544820236761646, -0.4531102586345839844 ) ) ;
#9657 = AXIS2_PLACEMENT_3D ( 'NONE', #23433, #1569, #16309 ) ;
#9658 = CARTESIAN_POINT ( 'NONE',  ( 15.03925126672132961, 1.793057972834833924, -4.026191436120374334 ) ) ;
#9660 = CARTESIAN_POINT ( 'NONE',  ( 58.75000018803718405, 0.9251739982205126056, 1.701355787207728509 ) ) ;
#9659 = CARTESIAN_POINT ( 'NONE',  ( -61.39999999999998437, 1.381785979968628826E-15, 2.054751023403646402E-15 ) ) ;
#9661 = ORIENTED_EDGE ( 'NONE', *, *, #20992, .F. ) ;
#9662 = CARTESIAN_POINT ( 'NONE',  ( -56.31249999999997868, -3.238593381231840151, -2.874284765127021579 ) ) ;
#9663 = CARTESIAN_POINT ( 'NONE',  ( -44.59999999999999432, 1.399999999999995692, 4.029888335921785192 ) ) ;
#9664 = CARTESIAN_POINT ( 'NONE',  ( 15.32752150720754081, -3.997744010329692177, -3.641645661657128219 ) ) ;
#9665 = CYLINDRICAL_SURFACE ( 'NONE', #10399, 3.399999999999999911 ) ;
#9666 = DIRECTION ( 'NONE',  ( 0.000000000000000000, -1.000000000000000000, 0.000000000000000000 ) ) ;
#9667 = EDGE_CURVE ( 'NONE', #25173, #28320, #16059, .T. ) ;
#9668 = ORIENTED_EDGE ( 'NONE', *, *, #14371, .F. ) ;
#9669 = CARTESIAN_POINT ( 'NONE',  ( 51.87968213909199733, -4.254331549871407603, -1.021189760102710675 ) ) ;
#9670 = EDGE_CURVE ( 'NONE', #8110, #25975, #21593, .T. ) ;
#9671 = DIRECTION ( 'NONE',  ( 0.000000000000000000, 1.000000000000000000, 0.000000000000000000 ) ) ;
#9672 = LINE ( 'NONE', #31191, #10906 ) ;
#9673 = CIRCLE ( 'NONE', #23817, 3.524999999999996358 ) ;
#9674 = DIRECTION ( 'NONE',  ( 0.000000000000000000, -0.8740818021021516948, 0.4857787595540328796 ) ) ;
#9676 = CARTESIAN_POINT ( 'NONE',  ( 52.83066426478726640, 8.351255136974236493, -1.927137645301873814 ) ) ;
#9675 = CARTESIAN_POINT ( 'NONE',  ( -62.08893835062482935, -2.688756313659543817, 0.2461493159769948258 ) ) ;
#9677 = CARTESIAN_POINT ( 'NONE',  ( -56.81249999999997158, 4.108500314926514463, -1.367561758111402348 ) ) ;
#9679 = DIRECTION ( 'NONE',  ( 0.000000000000000000, -1.000000000000000000, 1.224646799147352961E-16 ) ) ;
#9678 = LINE ( 'NONE', #28830, #18573 ) ;
#9680 = ORIENTED_EDGE ( 'NONE', *, *, #22072, .T. ) ;
#9681 = DIRECTION ( 'NONE',  ( -1.000000000000000000, -3.053848253006669023E-16, 2.042510438544995415E-16 ) ) ;
#9682 = LINE ( 'NONE', #12053, #11557 ) ;
#9684 = CARTESIAN_POINT ( 'NONE',  ( -35.85663232820596136, 4.861582140531585772, 2.394243978978369825 ) ) ;
#9683 = CARTESIAN_POINT ( 'NONE',  ( 15.41217651307626291, -2.840625797034020295, -4.363718033548148689 ) ) ;
#9685 = CARTESIAN_POINT ( 'NONE',  ( 50.25000000000000000, 1.666164585743128423, -1.106298139389324975 ) ) ;
#9686 = ORIENTED_EDGE ( 'NONE', *, *, #17336, .T. ) ;
#9687 = ORIENTED_EDGE ( 'NONE', *, *, #26658, .F. ) ;
#9688 = AXIS2_PLACEMENT_3D ( 'NONE', #14059, #6309, #18513 ) ;
#9689 = CARTESIAN_POINT ( 'NONE',  ( 51.59739104186229497, -1.010292945602101256, -1.272765950230260623 ) ) ;
#9690 = ORIENTED_EDGE ( 'NONE', *, *, #1875, .T. ) ;
#9691 = DIRECTION ( 'NONE',  ( 1.000000000000000000, 0.000000000000000000, 0.000000000000000000 ) ) ;
#9692 = DIRECTION ( 'NONE',  ( -1.000000000000000000, -3.054025858079668409E-16, 2.042474015755241579E-16 ) ) ;
#9693 = ORIENTED_EDGE ( 'NONE', *, *, #10815, .T. ) ;
#9694 = CARTESIAN_POINT ( 'NONE',  ( -59.62447745295619939, -2.166872014472563279, 1.529642084025434556 ) ) ;
#9695 = ORIENTED_EDGE ( 'NONE', *, *, #19855, .T. ) ;
#9696 = CARTESIAN_POINT ( 'NONE',  ( -60.24999999999997868, -0.6177564328763985868, 3.012308415424926444 ) ) ;
#9697 = ORIENTED_EDGE ( 'NONE', *, *, #13505, .T. ) ;
#9698 = VERTEX_POINT ( 'NONE', #24107 ) ;
#9699 = EDGE_CURVE ( 'NONE', #8227, #20392, #20125, .T. ) ;
#9700 = EDGE_LOOP ( 'NONE', ( #17536, #25438, #26531, #8843 ) ) ;
#9701 = EDGE_CURVE ( 'NONE', #709, #12762, #16637, .T. ) ;
#9702 = CARTESIAN_POINT ( 'NONE',  ( -56.32202994616206126, 2.078460969082646770, 3.599999999999807354 ) ) ;
#9703 = EDGE_CURVE ( 'NONE', #5737, #3048, #9232, .T. ) ;
#9704 = CARTESIAN_POINT ( 'NONE',  ( 50.42215036618306812, 1.308847734660516071, 3.885629509820973659 ) ) ;
#9705 = DIRECTION ( 'NONE',  ( 0.000000000000000000, 1.000000000000000000, 0.000000000000000000 ) ) ;
#9706 = CARTESIAN_POINT ( 'NONE',  ( -54.48167032960165557, -1.510995100284906023, 3.307167554963765799 ) ) ;
#9707 = CARTESIAN_POINT ( 'NONE',  ( -58.40835481156724285, -0.7533615035077920741, 3.673546848079180638 ) ) ;
#9708 = AXIS2_PLACEMENT_3D ( 'NONE', #757, #454, #20102 ) ;
#9710 = CARTESIAN_POINT ( 'NONE',  ( -36.11122220296835650, -0.3980941177579191970, -5.199999998461563244 ) ) ;
#9709 = DIRECTION ( 'NONE',  ( -8.778969181342580612E-15, 0.8381322357051846916, -0.5454670984320033611 ) ) ;
#9711 = CARTESIAN_POINT ( 'NONE',  ( -54.49999999999997868, -0.7533615035078020661, 3.673546848079177085 ) ) ;
#9712 = CYLINDRICAL_SURFACE ( 'NONE', #323, 0.1000000000000000472 ) ;
#9714 = CARTESIAN_POINT ( 'NONE',  ( 47.00000000000002132, -3.726179070414207928, 1.000000000000002220 ) ) ;
#9713 = CARTESIAN_POINT ( 'NONE',  ( 54.41118797001386298, 1.001877184765262739E-15, -4.375000000000000888 ) ) ;
#9715 = EDGE_CURVE ( 'NONE', #585, #7031, #5264, .T. ) ;
#9716 = ORIENTED_EDGE ( 'NONE', *, *, #7979, .F. ) ;
#9717 = CARTESIAN_POINT ( 'NONE',  ( 51.88812122917400416, 8.998461838226445408, -2.050000000000180123 ) ) ;
#9718 = CARTESIAN_POINT ( 'NONE',  ( 51.70000000000002416, 3.851905453475163110, 1.404572667215161053 ) ) ;
#9720 = CARTESIAN_POINT ( 'NONE',  ( -54.39999999999999147, -1.400000000000006795, 3.959797974644449603 ) ) ;
#9719 = CARTESIAN_POINT ( 'NONE',  ( 48.46694841591348535, -1.365427245289796199, 3.854926352964885172 ) ) ;
#9721 = ORIENTED_EDGE ( 'NONE', *, *, #2137, .T. ) ;
#9722 = DIRECTION ( 'NONE',  ( 1.000000000000000000, 3.053848253006669023E-16, -2.042510438544995415E-16 ) ) ;
#9723 = ORIENTED_EDGE ( 'NONE', *, *, #15195, .T. ) ;
#9724 = AXIS2_PLACEMENT_3D ( 'NONE', #19599, #256, #24471 ) ;
#9725 = DIRECTION ( 'NONE',  ( 1.000000000000000000, -0.000000000000000000, -1.047444401652940007E-14 ) ) ;
#9726 = CARTESIAN_POINT ( 'NONE',  ( -58.50952994616205416, -4.643455692769885398E-15, 3.599999999999791367 ) ) ;
#9727 = ORIENTED_EDGE ( 'NONE', *, *, #14651, .T. ) ;
#9728 = ORIENTED_EDGE ( 'NONE', *, *, #3684, .T. ) ;
#9729 = CARTESIAN_POINT ( 'NONE',  ( 15.56274145962601274, 4.735538777079207229, 2.618062770414690821 ) ) ;
#9730 = ORIENTED_EDGE ( 'NONE', *, *, #12546, .F. ) ;
#9731 = CARTESIAN_POINT ( 'NONE',  ( 48.45862863613069749, -1.344608935533137206, 3.858631320448701718 ) ) ;
#9732 = CARTESIAN_POINT ( 'NONE',  ( -56.19702994616206837, -2.078460969082657872, 3.599999999999791811 ) ) ;
#9733 = VERTEX_POINT ( 'NONE', #26167 ) ;
#9734 = CARTESIAN_POINT ( 'NONE',  ( 58.45000000000001705, -0.8000000000000000444, -2.421260002560650104 ) ) ;
#9735 = CYLINDRICAL_SURFACE ( 'NONE', #17732, 0.1500000000000000777 ) ;
#9736 = CARTESIAN_POINT ( 'NONE',  ( 34.56702326949726256, 8.213851659285209550, 2.049999999999878586 ) ) ;
#9737 = EDGE_LOOP ( 'NONE', ( #6073, #2268, #1328, #24117, #2143, #16536 ) ) ;
#9738 = EDGE_CURVE ( 'NONE', #590, #23750, #23801, .T. ) ;
#9739 = DIRECTION ( 'NONE',  ( 0.000000000000000000, -0.2008964009354147484, 0.9796124928211139560 ) ) ;
#9740 = CARTESIAN_POINT ( 'NONE',  ( -54.49131719536980967, -1.521332553059527859, 4.044684194243341580 ) ) ;
#9741 = CARTESIAN_POINT ( 'NONE',  ( 58.75000018803719826, -0.9251739982198918799, -1.701355787207161852 ) ) ;
#9742 = CYLINDRICAL_SURFACE ( 'NONE', #14472, 0.1500000000000001887 ) ;
#9743 = CARTESIAN_POINT ( 'NONE',  ( 52.20711756518984714, -0.7499999999994533262, -1.718465885608440713 ) ) ;
#9745 = CYLINDRICAL_SURFACE ( 'NONE', #29567, 2.000000000000000000 ) ;
#9744 = PRESENTATION_STYLE_ASSIGNMENT (( #28898 ) ) ;
#9746 = CARTESIAN_POINT ( 'NONE',  ( 51.50435016707358926, 0.9265794315412880788, 1.339215852266871565 ) ) ;
#9747 = CARTESIAN_POINT ( 'NONE',  ( 50.87477060347374902, 8.633605004118187765, 1.949999999999822320 ) ) ;
#9748 = ADVANCED_FACE ( 'NONE', ( #344 ), #5941, .T. ) ;
#9749 = CARTESIAN_POINT ( 'NONE',  ( 51.68129744678917348, 4.333300462208747206, 1.549999999999819300 ) ) ;
#9750 = VERTEX_POINT ( 'NONE', #24265 ) ;
#9751 = ORIENTED_EDGE ( 'NONE', *, *, #24073, .F. ) ;
#9752 = LINE ( 'NONE', #14494, #17887 ) ;
#9753 = ORIENTED_EDGE ( 'NONE', *, *, #24882, .T. ) ;
#9754 = DIRECTION ( 'NONE',  ( 1.000000000000000000, -0.000000000000000000, -1.047444401652940007E-14 ) ) ;
#9755 = CARTESIAN_POINT ( 'NONE',  ( -54.98542740578361077, 2.936324665650207333, 2.606018187048498191 ) ) ;
#9756 = CARTESIAN_POINT ( 'NONE',  ( 15.59055531549693541, 5.360541651686752118, 0.7128348320084746392 ) ) ;
#9757 = ORIENTED_EDGE ( 'NONE', *, *, #12510, .T. ) ;
#9758 = VERTEX_POINT ( 'NONE', #2577 ) ;
#9759 = EDGE_CURVE ( 'NONE', #11263, #3318, #5351, .T. ) ;
#9760 = CARTESIAN_POINT ( 'NONE',  ( -71.44999999999998863, -1.380331489585512972E-15, 2.906968604901091669E-15 ) ) ;
#9761 = VERTEX_POINT ( 'NONE', #29317 ) ;
#9762 = DIRECTION ( 'NONE',  ( 1.000000000000000000, -0.000000000000000000, -1.047444401652940007E-14 ) ) ;
#9763 = ORIENTED_EDGE ( 'NONE', *, *, #9417, .T. ) ;
#9764 = CARTESIAN_POINT ( 'NONE',  ( 58.66107449606931823, -1.640741681269791030, 0.9081280691417603634 ) ) ;
#9765 = B_SPLINE_CURVE_WITH_KNOTS ( 'NONE', 3,
 ( #3897, #13544, #23227, #14907 ),
 .UNSPECIFIED., .F., .F.,
 ( 4, 4 ),
 ( 0.3274566953765374877, 0.3970257546597420473 ),
 .UNSPECIFIED. ) ;
#9766 = ORIENTED_EDGE ( 'NONE', *, *, #28456, .T. ) ;
#9767 = CARTESIAN_POINT ( 'NONE',  ( -71.49999999999998579, -1.395601618875910821E-15, 2.917180974979867506E-15 ) ) ;
#9768 = FACE_OUTER_BOUND ( 'NONE', #26838, .T. ) ;
#9769 = ADVANCED_FACE ( 'NONE', ( #24861 ), #18849, .T. ) ;
#9770 = CARTESIAN_POINT ( 'NONE',  ( -56.95655989232412963, 1.962990915244722245, 3.399999999999804956 ) ) ;
#9771 = CARTESIAN_POINT ( 'NONE',  ( 53.21917409580258607, 8.083376426877340037, -2.050000000000185008 ) ) ;
#9772 = CARTESIAN_POINT ( 'NONE',  ( 33.05069135236685440, 8.148093138862860130, 1.549999999999884803 ) ) ;
#9773 = CARTESIAN_POINT ( 'NONE',  ( 58.64999999999999858, 1.760622601997808845, -0.8948927608024527247 ) ) ;
#9774 = AXIS2_PLACEMENT_3D ( 'NONE', #10131, #19796, #29430 ) ;
#9775 = CYLINDRICAL_SURFACE ( 'NONE', #11942, 0.2500000000000000000 ) ;
#9776 = ADVANCED_FACE ( 'NONE', ( #7938 ), #12360, .F. ) ;
#9777 = DIRECTION ( 'NONE',  ( 0.000000000000000000, -0.9996898646859344595, -0.02490330187381124480 ) ) ;
#9778 = ORIENTED_EDGE ( 'NONE', *, *, #24665, .T. ) ;
#9779 = CARTESIAN_POINT ( 'NONE',  ( 51.80000000000001847, 2.428612866367529932E-14, -4.100000000000022737 ) ) ;
#9781 = CARTESIAN_POINT ( 'NONE',  ( -54.49999999999997868, 1.549582583372307809, 3.331868970650947226 ) ) ;
#9780 = CARTESIAN_POINT ( 'NONE',  ( -36.31414349454748702, -3.102491976071088065, -4.173461118157653971 ) ) ;
#9782 = CARTESIAN_POINT ( 'NONE',  ( 53.90845421530191572, 6.078720411350368558, -0.8364387603671682436 ) ) ;
#9783 = ORIENTED_EDGE ( 'NONE', *, *, #23524, .T. ) ;
#9784 = CARTESIAN_POINT ( 'NONE',  ( -36.81959771849335539, -5.295593823078834639, 1.114646847977607935 ) ) ;
#9785 = VERTEX_POINT ( 'NONE', #7628 ) ;
#9786 = CARTESIAN_POINT ( 'NONE',  ( -36.38012252111052902, -4.735538777079435491, 2.618062770414280926 ) ) ;
#9788 = CARTESIAN_POINT ( 'NONE',  ( 47.76581851340797868, -3.901693722832459521, -1.260438308020617404 ) ) ;
#9787 = CARTESIAN_POINT ( 'NONE',  ( 58.74154451056412540, 1.017012227666128643, -1.575232816092163590 ) ) ;
#9789 = EDGE_CURVE ( 'NONE', #30371, #10647, #23646, .T. ) ;
#9790 = ORIENTED_EDGE ( 'NONE', *, *, #25669, .T. ) ;
#9791 = FACE_OUTER_BOUND ( 'NONE', #24086, .T. ) ;
#9792 = CARTESIAN_POINT ( 'NONE',  ( 49.00000000000004263, 0.6617647058823536987, 1.754335336828920955 ) ) ;
#9794 = CARTESIAN_POINT ( 'NONE',  ( -54.44999999999997442, -1.499999999999999556, -4.029888335921975262 ) ) ;
#9793 = DIRECTION ( 'NONE',  ( 1.000000000000000000, 5.570239943078568709E-15, -9.650165233619991632E-15 ) ) ;
#9795 = ORIENTED_EDGE ( 'NONE', *, *, #1150, .T. ) ;
#9796 = CARTESIAN_POINT ( 'NONE',  ( -58.74999999999997158, -2.489203624310586171, 2.804704140674917134 ) ) ;
#9797 = AXIS2_PLACEMENT_3D ( 'NONE', #12454, #736, #7568 ) ;
#9798 = CARTESIAN_POINT ( 'NONE',  ( -44.59999999999999432, 1.399999999999995914, 3.959797974644454044 ) ) ;
#9799 = CARTESIAN_POINT ( 'NONE',  ( -56.15835481156722864, -0.7533615035077977362, 3.673546848079179750 ) ) ;
#9800 = DIRECTION ( 'NONE',  ( 0.000000000000000000, 0.000000000000000000, 1.000000000000000000 ) ) ;
#9801 = CONTEXT_DEPENDENT_SHAPE_REPRESENTATION ( #19915, #4551 ) ;
#9802 = ADVANCED_FACE ( 'NONE', ( #29167 ), #899, .T. ) ;
#9803 = DIRECTION ( 'NONE',  ( 1.000000000000000000, -0.000000000000000000, -1.047444401652940007E-14 ) ) ;
#9804 = CARTESIAN_POINT ( 'NONE',  ( -54.44999999999997442, 0.000000000000000000, 0.000000000000000000 ) ) ;
#9805 = DIRECTION ( 'NONE',  ( 1.000000000000000000, 1.047444401652940007E-14, 0.000000000000000000 ) ) ;
#9806 = ORIENTED_EDGE ( 'NONE', *, *, #6268, .T. ) ;
#9807 =( BOUNDED_SURFACE ( )  B_SPLINE_SURFACE ( 3, 2, ( 
 ( #29782, #8098, #3650 ),
 ( #13285, #13148, #17765 ),
 ( #10771, #27406, #20454 ),
 ( #30079, #15366, #25016 ),
 ( #978, #8398, #3346 ),
 ( #22682, #10630, #29936 ),
 ( #8245, #28503, #18707 ),
 ( #16319, #4268, #20915 ),
 ( #21555, #6656, #3962 ),
 ( #13914, #21087, #25962 ) ),
 .UNSPECIFIED., .F., .F., .T. ) 
 B_SPLINE_SURFACE_WITH_KNOTS ( ( 4, 2, 2, 2, 4 ),
 ( 3, 3 ),
 ( 0.0001706658715699975362, 0.0002229276920781214167, 0.0002751895125862452701, 0.0003274513330943691234, 0.0003797131536024929768 ),
 ( 0.000000000000000000, 1.000000000000000000 ),
 .UNSPECIFIED. ) 
 GEOMETRIC_REPRESENTATION_ITEM ( )  RATIONAL_B_SPLINE_SURFACE ( (
 ( 1.000000000000000000, 0.7071067811873480435, 1.000000000000000000),
 ( 1.000000000000000000, 0.7375607040708425099, 1.000000000000000000),
 ( 1.000000000000000000, 0.7730431127430062999, 1.000000000000000000),
 ( 1.000000000000000000, 0.8321012486976929745, 1.000000000000000000),
 ( 1.000000000000000000, 0.8541932017391521414, 1.000000000000000000),
 ( 1.000000000000000000, 0.8545723906038292794, 1.000000000000000000),
 ( 1.000000000000000000, 0.8327032135030432158, 1.000000000000000000),
 ( 1.000000000000000000, 0.7734559727055867473, 1.000000000000000000),
 ( 1.000000000000000000, 0.7377766653993185209, 1.000000000000000000),
 ( 1.000000000000000000, 0.7071067811865511255, 1.000000000000000000) ) ) 
 REPRESENTATION_ITEM ( '' )  SURFACE ( )  );
#9808 = CARTESIAN_POINT ( 'NONE',  ( 36.55000000000001847, 0.000000000000000000, 0.000000000000000000 ) ) ;
#9809 = LINE ( 'NONE', #24229, #28619 ) ;
#9810 = CARTESIAN_POINT ( 'NONE',  ( -54.49999999999997868, 0.000000000000000000, 0.000000000000000000 ) ) ;
#9811 = EDGE_CURVE ( 'NONE', #30937, #8932, #14, .T. ) ;
#9812 = CARTESIAN_POINT ( 'NONE',  ( -59.38710602098247193, 3.262177753127958102, -1.057889186448619512 ) ) ;
#9813 = AXIS2_PLACEMENT_3D ( 'NONE', #21885, #12502, #24534 ) ;
#9814 = CARTESIAN_POINT ( 'NONE',  ( 58.75000000000003553, -1.791164585742988757, 0.8897917884442223535 ) ) ;
#9816 = CARTESIAN_POINT ( 'NONE',  ( 58.65000000000000568, 1.077297519405725046, -1.655311165516502925 ) ) ;
#9815 = DIRECTION ( 'NONE',  ( -1.000000000000000000, -1.047444401652940007E-14, -0.000000000000000000 ) ) ;
#9817 = VERTEX_POINT ( 'NONE', #2675 ) ;
#9818 = CARTESIAN_POINT ( 'NONE',  ( 58.74999999999981526, -1.782657835994365003, 0.5811678240970542531 ) ) ;
#9819 = PRODUCT_DEFINITION_CONTEXT ( 'detailed design', #26389, 'design' ) ;
#9820 = CARTESIAN_POINT ( 'NONE',  ( 51.80000000000001137, 4.175664755576646847, -1.929721184274108436 ) ) ;
#9822 = CARTESIAN_POINT ( 'NONE',  ( 58.72219294808299139, -0.4999999999993851585, -1.828782891498922369 ) ) ;
#9821 = CARTESIAN_POINT ( 'NONE',  ( 15.56274145962692046, -2.292272662153287399, -4.901537128431941781 ) ) ;
#9823 = CARTESIAN_POINT ( 'NONE',  ( 58.50000000000001421, 0.000000000000000000, 0.000000000000000000 ) ) ;
#9824 = ADVANCED_FACE ( 'NONE', ( #19171 ), #14703, .F. ) ;
#9825 = ORIENTED_EDGE ( 'NONE', *, *, #22984, .F. ) ;
#9826 = AXIS2_PLACEMENT_3D ( 'NONE', #6699, #7030, #16359 ) ;
#9827 = VERTEX_POINT ( 'NONE', #24364 ) ;
#9828 = CARTESIAN_POINT ( 'NONE',  ( 69.20000000000003126, 3.252606517456513302E-16, -7.248315259438346108E-13 ) ) ;
#9829 = ORIENTED_EDGE ( 'NONE', *, *, #19425, .F. ) ;
#9830 = EDGE_CURVE ( 'NONE', #31046, #4702, #19647, .T. ) ;
#9831 = CARTESIAN_POINT ( 'NONE',  ( 51.71945504228668966, -4.178364716350985830, 1.001910748144234864 ) ) ;
#9832 = FACE_OUTER_BOUND ( 'NONE', #14252, .T. ) ;
#9833 = ORIENTED_EDGE ( 'NONE', *, *, #29184, .F. ) ;
#9834 = CARTESIAN_POINT ( 'NONE',  ( -36.76447480099743359, -5.297368390263450522, -1.087079755157686289 ) ) ;
#9835 = ORIENTED_EDGE ( 'NONE', *, *, #20469, .F. ) ;
#9836 =( LENGTH_UNIT ( ) NAMED_UNIT ( * ) SI_UNIT ( .MILLI., .METRE. ) );
#9837 = CARTESIAN_POINT ( 'NONE',  ( 58.65000000000003411, -1.394635017527474430, -1.253243060178046875 ) ) ;
#9838 = ORIENTED_EDGE ( 'NONE', *, *, #6125, .F. ) ;
#9839 = EDGE_CURVE ( 'NONE', #13554, #5591, #3410, .T. ) ;
#9840 = TOROIDAL_SURFACE ( 'NONE', #21969, 3.524999999999996358, 0.1000000000000000056 ) ;
#9841 = EDGE_CURVE ( 'NONE', #13311, #20255, #15540, .T. ) ;
#9842 = ORIENTED_EDGE ( 'NONE', *, *, #3822, .T. ) ;
#9843 = CARTESIAN_POINT ( 'NONE',  ( -59.57202994616203995, 2.078460969082674747, -3.600000000000202593 ) ) ;
#9844 = DIRECTION ( 'NONE',  ( 0.9992009587217894895, 0.008029435056737248277, -0.03915318968010821771 ) ) ;
#9845 = DIRECTION ( 'NONE',  ( 1.047444401652940007E-14, 0.000000000000000000, 1.000000000000000000 ) ) ;
#9846 = CARTESIAN_POINT ( 'NONE',  ( 56.95000000000001705, 0.000000000000000000, 0.000000000000000000 ) ) ;
#9847 = CARTESIAN_POINT ( 'NONE',  ( 51.75323112273434845, -4.276948283761179859, -0.9210528638641413135 ) ) ;
#9849 = CARTESIAN_POINT ( 'NONE',  ( -35.98952425903316055, -0.4576450703117335150, -5.200000005133903258 ) ) ;
#9848 = CARTESIAN_POINT ( 'NONE',  ( 58.64999999999992752, -1.932246131436387682, -0.4087173687853297710 ) ) ;
#9850 = CIRCLE ( 'NONE', #30066, 4.300000000000016698 ) ;
#9851 = VECTOR ( 'NONE', #27599, 999.9999999999998863 ) ;
#9852 = CARTESIAN_POINT ( 'NONE',  ( 58.75000000000002132, 6.153735859711025284E-13, 3.111507638930570854E-58 ) ) ;
#9853 = CARTESIAN_POINT ( 'NONE',  ( 15.32766723174652945, -3.997758138077576628, 3.641634024966071692 ) ) ;
#9855 = DIRECTION ( 'NONE',  ( 1.000000000000000000, 1.047444401652940007E-14, 0.000000000000000000 ) ) ;
#9854 = CARTESIAN_POINT ( 'NONE',  ( 15.29449157529478320, 4.822464347458993217, -1.985534350301433326 ) ) ;
#9856 = VERTEX_POINT ( 'NONE', #5050 ) ;
#9857 = CARTESIAN_POINT ( 'NONE',  ( -54.49999999999998579, 1.514093959731539263, 3.183260039818149423 ) ) ;
#9858 = AXIS2_PLACEMENT_3D ( 'NONE', #2310, #2001, #2482 ) ;
#9859 = FACE_OUTER_BOUND ( 'NONE', #2051, .T. ) ;
#9861 = DIRECTION ( 'NONE',  ( -0.3180732113053867383, -0.9480661539417379879, -0.000000000000000000 ) ) ;
#9860 = DIRECTION ( 'NONE',  ( 1.000000000000000000, 2.586136946169074517E-16, -0.000000000000000000 ) ) ;
#9862 = CARTESIAN_POINT ( 'NONE',  ( 47.37886355347654899, -4.356776102639407178, 1.481376528583874252 ) ) ;
#9863 = EDGE_CURVE ( 'NONE', #20313, #4537, #18661, .T. ) ;
#9864 = VERTEX_POINT ( 'NONE', #9799 ) ;
#9865 = DIRECTION ( 'NONE',  ( 0.7071067811865404673, 0.7071067811865546782, 0.000000000000000000 ) ) ;
#9866 = ADVANCED_FACE ( 'NONE', ( #4887 ), #9986, .T. ) ;
#9867 = ORIENTED_EDGE ( 'NONE', *, *, #30812, .F. ) ;
#9868 = AXIS2_PLACEMENT_3D ( 'NONE', #17931, #27571, #21106 ) ;
#9869 = ADVANCED_FACE ( 'NONE', ( #28954 ), #4579, .T. ) ;
#9870 = CARTESIAN_POINT ( 'NONE',  ( -59.96464466094062828, -0.9714054848608590920, 4.736774497371793125 ) ) ;
#9871 = ORIENTED_EDGE ( 'NONE', *, *, #12025, .T. ) ;
#9872 = ORIENTED_EDGE ( 'NONE', *, *, #13093, .F. ) ;
#9873 = CARTESIAN_POINT ( 'NONE',  ( 15.59055531549693363, 4.755763096844290772, -2.574151833883746576 ) ) ;
#9874 = ORIENTED_EDGE ( 'NONE', *, *, #12813, .T. ) ;
#9875 = CARTESIAN_POINT ( 'NONE',  ( 48.40000000000001990, -0.7618928438396727065, 3.939512004971702730 ) ) ;
#9876 = CARTESIAN_POINT ( 'NONE',  ( -56.13452994616205416, -3.117691453623976816, 1.799999999999788436 ) ) ;
#9877 = ORIENTED_EDGE ( 'NONE', *, *, #1624, .F. ) ;
#9878 = CARTESIAN_POINT ( 'NONE',  ( -56.43749999999998579, 1.962990915244719803, 3.399999999999808509 ) ) ;
#9879 = CARTESIAN_POINT ( 'NONE',  ( -64.32138495697122949, 4.896393452479652361E-16, 2.651446950365857792E-15 ) ) ;
#9880 = AXIS2_PLACEMENT_3D ( 'NONE', #13442, #12823, #22506 ) ;
#9881 = CARTESIAN_POINT ( 'NONE',  ( 27.54696499484943217, 5.363421040470448986, 2.049999999999772893 ) ) ;
#9882 = ORIENTED_EDGE ( 'NONE', *, *, #12606, .F. ) ;
#9883 = CIRCLE ( 'NONE', #21034, 1.000000000000000000 ) ;
#9884 = CARTESIAN_POINT ( 'NONE',  ( -55.06249999999997158, 3.925981830489463142, -1.814330073843579337E-13 ) ) ;
#9885 = CARTESIAN_POINT ( 'NONE',  ( 52.48761841068137812, 8.622213116012012790, -2.050000000000182343 ) ) ;
#9886 = CARTESIAN_POINT ( 'NONE',  ( 50.56924445453658024, 0.1015585333208254837, -0.8011027422770338191 ) ) ;
#9887 = CARTESIAN_POINT ( 'NONE',  ( 48.50000000000002132, 1.426739617975221641, -3.843750000000023093 ) ) ;
#9888 = DIRECTION ( 'NONE',  ( -1.000000000000000000, -1.047444401652940007E-14, -0.000000000000000000 ) ) ;
#9889 = VECTOR ( 'NONE', #28421, 1000.000000000000000 ) ;
#9890 = AXIS2_PLACEMENT_3D ( 'NONE', #7010, #2568, #16672 ) ;
#9892 = CARTESIAN_POINT ( 'NONE',  ( 58.65000000000001990, 6.143261415694495821E-13, 3.111507638930570854E-58 ) ) ;
#9891 = CARTESIAN_POINT ( 'NONE',  ( -36.89250464418362441, -3.430438802933830189, 4.182416543699121192 ) ) ;
#9893 = CARTESIAN_POINT ( 'NONE',  ( 51.31802667458094902, 1.005866567097610575, 1.281163073955430720 ) ) ;
#9894 = DIRECTION ( 'NONE',  ( -1.000000000000000000, 1.219044193948983948E-29, -3.491481338843133355E-15 ) ) ;
#9895 = DIRECTION ( 'NONE',  ( 0.000000000000000000, 0.000000000000000000, 1.000000000000000000 ) ) ;
#9896 = ORIENTED_EDGE ( 'NONE', *, *, #25422, .F. ) ;
#9897 = AXIS2_PLACEMENT_3D ( 'NONE', #13561, #3745, #27832 ) ;
#9898 = AXIS2_PLACEMENT_3D ( 'NONE', #13756, #1729, #11397 ) ;
#9899 = EDGE_CURVE ( 'NONE', #31290, #21780, #28705, .T. ) ;
#9900 = AXIS2_PLACEMENT_3D ( 'NONE', #16197, #28056, #25845 ) ;
#9901 = VERTEX_POINT ( 'NONE', #6794 ) ;
#9902 = ORIENTED_EDGE ( 'NONE', *, *, #10374, .T. ) ;
#9903 = CYLINDRICAL_SURFACE ( 'NONE', #8813, 0.2500000000000002220 ) ;
#9904 = CARTESIAN_POINT ( 'NONE',  ( -60.34585481156722864, -1.184343223768586695, -3.558065644182724974 ) ) ;
#9906 = DIRECTION ( 'NONE',  ( 0.9992009587217894895, -0.008029435056736641124, 0.03915318968010780831 ) ) ;
#9905 = CARTESIAN_POINT ( 'NONE',  ( 15.32752150720753725, 5.374748457514294309, 0.5963382560600952731 ) ) ;
#9907 = ORIENTED_EDGE ( 'NONE', *, *, #26129, .F. ) ;
#9908 = PRESENTATION_LAYER_ASSIGNMENT (  '', '', ( #21567 ) ) ;
#9909 = ORIENTED_EDGE ( 'NONE', *, *, #17370, .T. ) ;
#9910 = CARTESIAN_POINT ( 'NONE',  ( 22.49424290799312942, 6.943762543480787031, -2.050000000000077538 ) ) ;
#9911 = VERTEX_POINT ( 'NONE', #2360 ) ;
#9912 = AXIS2_PLACEMENT_3D ( 'NONE', #9382, #16508, #23948 ) ;
#9913 = DIRECTION ( 'NONE',  ( 0.000000000000000000, 0.000000000000000000, 1.000000000000000000 ) ) ;
#9914 = ORIENTED_EDGE ( 'NONE', *, *, #17649, .T. ) ;
#9915 = CARTESIAN_POINT ( 'NONE',  ( 31.86617018594280282, 7.736336509539960105, -2.050000000000112177 ) ) ;
#9916 = VECTOR ( 'NONE', #9803, 1000.000000000000000 ) ;
#9917 = VERTEX_POINT ( 'NONE', #21705 ) ;
#9918 = DIRECTION ( 'NONE',  ( 0.000000000000000000, -1.000000000000000000, -1.715124499442879341E-15 ) ) ;
#9919 = CYLINDRICAL_SURFACE ( 'NONE', #2642, 3.399999999999999911 ) ;
#9920 = ADVANCED_FACE ( 'NONE', ( #7263 ), #27681, .T. ) ;
#9921 = TOROIDAL_SURFACE ( 'NONE', #14966, 4.800000000000000711, 0.05000000000000000278 ) ;
#9922 = LINE ( 'NONE', #26856, #28410 ) ;
#9923 = CARTESIAN_POINT ( 'NONE',  ( -55.89405989232412253, -2.944486372867076263, -1.700000000000208900 ) ) ;
#9924 = CARTESIAN_POINT ( 'NONE',  ( 53.74478519188839698, 7.379842749953129832, -1.837855077339860976 ) ) ;
#9925 = AXIS2_PLACEMENT_3D ( 'NONE', #26480, #13541, #25573 ) ;
#9926 = AXIS2_PLACEMENT_3D ( 'NONE', #13643, #6687, #16348 ) ;
#9927 = CIRCLE ( 'NONE', #25073, 0.09999999999999986677 ) ;
#9928 = DIRECTION ( 'NONE',  ( -0.000000000000000000, -0.000000000000000000, -1.000000000000000000 ) ) ;
#9929 = DIRECTION ( 'NONE',  ( 0.000000000000000000, 0.000000000000000000, 1.000000000000000000 ) ) ;
#9930 = AXIS2_PLACEMENT_3D ( 'NONE', #2645, #22133, #2330 ) ;
#9931 = SURFACE_SIDE_STYLE ('',( #28784 ) ) ;
#9932 = VECTOR ( 'NONE', #28865, 1000.000000000000000 ) ;
#9933 = CIRCLE ( 'NONE', #31150, 0.1500000000000001887 ) ;
#9934 = CARTESIAN_POINT ( 'NONE',  ( -58.95655989232411542, -3.399999999999991029, -2.281093130107142867E-13 ) ) ;
#9935 = ORIENTED_EDGE ( 'NONE', *, *, #16589, .F. ) ;
#9936 = DIRECTION ( 'NONE',  ( 0.9957419851083220141, 0.09218405009836627695, -2.168404344971037661E-15 ) ) ;
#9937 = CARTESIAN_POINT ( 'NONE',  ( -36.25997906085250122, -3.232943006030368327, -4.078682900256746180 ) ) ;
#9938 = CARTESIAN_POINT ( 'NONE',  ( 54.40000000000001990, 3.918869757271530460E-16, 3.200000000000000178 ) ) ;
#9939 = ORIENTED_EDGE ( 'NONE', *, *, #25683, .T. ) ;
#9940 = EDGE_CURVE ( 'NONE', #26028, #27144, #16452, .T. ) ;
#9941 = CARTESIAN_POINT ( 'NONE',  ( -54.48118151432741030, 1.510613940323803916, 4.037256667234631280 ) ) ;
#9942 = ORIENTED_EDGE ( 'NONE', *, *, #24706, .F. ) ;
#9943 = CIRCLE ( 'NONE', #12034, 4.375000000000000000 ) ;
#9944 = EDGE_CURVE ( 'NONE', #25442, #7031, #2529, .T. ) ;
#9945 = CARTESIAN_POINT ( 'NONE',  ( 16.10624235918717417, 0.1627367787820844514, -5.407318510437580272 ) ) ;
#9946 = LINE ( 'NONE', #29260, #3184 ) ;
#9948 = CARTESIAN_POINT ( 'NONE',  ( 50.50000000000002132, 2.428612866367529932E-14, 0.000000000000000000 ) ) ;
#9947 = CARTESIAN_POINT ( 'NONE',  ( -35.85663232820584057, 2.686240680702182804, -4.475885388010699018 ) ) ;
#9949 = ORIENTED_EDGE ( 'NONE', *, *, #24930, .F. ) ;
#9950 = AXIS2_PLACEMENT_3D ( 'NONE', #30254, #18242, #3968 ) ;
#9951 = CARTESIAN_POINT ( 'NONE',  ( -67.33025350686975230, -4.292234512154642818E-16, 3.266011492503604425E-15 ) ) ;
#9952 = CARTESIAN_POINT ( 'NONE',  ( 59.00000000000000000, 1.401298464324817071E-42, -2.875000000000617284 ) ) ;
#9953 = AXIS2_PLACEMENT_3D ( 'NONE', #3351, #13289, #25020 ) ;
#9955 = CARTESIAN_POINT ( 'NONE',  ( 69.25000000000000000, 0.8558823529411767606, -2.268940368966791965 ) ) ;
#9954 = CARTESIAN_POINT ( 'NONE',  ( 52.38143600039783365, 3.988258350863520096, 2.045676845274237543 ) ) ;
#9956 = ORIENTED_EDGE ( 'NONE', *, *, #13610, .T. ) ;
#9957 = CARTESIAN_POINT ( 'NONE',  ( -57.56249999999997868, 4.108500314926511798, -1.367561758111407455 ) ) ;
#9958 = CARTESIAN_POINT ( 'NONE',  ( 15.03925126672132961, 3.426725943139508512, 3.937891353488783164 ) ) ;
#9959 = CARTESIAN_POINT ( 'NONE',  ( 57.02478278053006022, -0.7769964508979760875, 1.733862565638740305 ) ) ;
#9960 = VECTOR ( 'NONE', #19223, 1000.000000000000000 ) ;
#9961 = CARTESIAN_POINT ( 'NONE',  ( 63.50000000000002842, 1.401298464324817071E-42, -6.651271950496169736E-13 ) ) ;
#9962 = ADVANCED_FACE ( 'NONE', ( #11858 ), #27095, .T. ) ;
#9963 = CARTESIAN_POINT ( 'NONE',  ( -54.49999999999997868, 0.2900967345938421649, -3.387601494358211340 ) ) ;
#9964 = CARTESIAN_POINT ( 'NONE',  ( -57.93749999999998579, 1.962990915244718026, 3.399999999999803624 ) ) ;
#9965 = AXIS2_PLACEMENT_3D ( 'NONE', #27913, #13491, #13322 ) ;
#9966 = AXIS2_PLACEMENT_3D ( 'NONE', #22868, #20345, #13182 ) ;
#9967 =( BOUNDED_CURVE ( )  B_SPLINE_CURVE ( 3, ( #6482, #16142, #13739, #30702 ),
 .UNSPECIFIED., .F., .T. ) 
 B_SPLINE_CURVE_WITH_KNOTS ( ( 4, 4 ),
 ( 1.454199501120271742, 2.189070931013919807 ),
 .UNSPECIFIED. ) 
 CURVE ( )  GEOMETRIC_REPRESENTATION_ITEM ( )  RATIONAL_B_SPLINE_CURVE ( ( 1.000000000000000000, 0.9555010429016488338, 0.9555010429016488338, 1.000000000000000000 ) ) 
 REPRESENTATION_ITEM ( '' )  );
#9968 = CYLINDRICAL_SURFACE ( 'NONE', #6294, 1.899999999999999911 ) ;
#9969 = ORIENTED_EDGE ( 'NONE', *, *, #26922, .F. ) ;
#9970 = CARTESIAN_POINT ( 'NONE',  ( 15.44259799936805955, -3.232943006030354560, 4.078682900256773713 ) ) ;
#9971 = AXIS2_PLACEMENT_3D ( 'NONE', #28166, #1413, #1563 ) ;
#9972 = CARTESIAN_POINT ( 'NONE',  ( 23.27385761420496735, 6.062155931322325664, -1.950000000000080780 ) ) ;
#9973 = CIRCLE ( 'NONE', #27166, 0.1500000000000001887 ) ;
#9974 = DIRECTION ( 'NONE',  ( -2.964772755551650383E-16, 0.9875000000000001554, 0.1576190026614809614 ) ) ;
#9975 = TOROIDAL_SURFACE ( 'NONE', #14002, 0.3000000000000000444, 0.05000000000000000278 ) ;
#9976 = CARTESIAN_POINT ( 'NONE',  ( -59.29999999999997584, 0.7533615035078071731, -3.673546848079177529 ) ) ;
#9977 = DIRECTION ( 'NONE',  ( -1.000000000000000000, -0.000000000000000000, 1.047444401652940007E-14 ) ) ;
#9979 = CARTESIAN_POINT ( 'NONE',  ( 26.41339658680651326, 5.213169555504943098, 1.424999999999908340 ) ) ;
#9978 = CARTESIAN_POINT ( 'NONE',  ( 58.65000000000001279, 0.5811678240972314446, 1.782657835995122175 ) ) ;
#9980 = VERTEX_POINT ( 'NONE', #17102 ) ;
#9981 = AXIS2_PLACEMENT_3D ( 'NONE', #27025, #26419, #5333 ) ;
#9982 = ADVANCED_FACE ( 'NONE', ( #9334 ), #20099, .F. ) ;
#9983 = CARTESIAN_POINT ( 'NONE',  ( 58.75000000000004263, -1.877732920580553300, 0.6121634413821477327 ) ) ;
#9984 = AXIS2_PLACEMENT_3D ( 'NONE', #28191, #4440, #6806 ) ;
#9985 = ORIENTED_EDGE ( 'NONE', *, *, #12479, .T. ) ;
#9986 = TOROIDAL_SURFACE ( 'NONE', #13510, -24.59258869922086888, 30.00000000000000000 ) ;
#9987 = DIRECTION ( 'NONE',  ( 0.000000000000000000, 0.000000000000000000, 1.000000000000000000 ) ) ;
#9989 = DIRECTION ( 'NONE',  ( 0.000000000000000000, -1.000000000000000000, 2.168404344971008868E-16 ) ) ;
#9988 = CARTESIAN_POINT ( 'NONE',  ( -54.49227792872101617, -2.349139337603836530, -2.680014161610996037 ) ) ;
#9991 = EDGE_CURVE ( 'NONE', #10898, #19112, #20032, .T. ) ;
#9990 = CARTESIAN_POINT ( 'NONE',  ( 58.45000000000001705, -0.7500000000000000000, -2.489477856900920383 ) ) ;
#9992 = ORIENTED_EDGE ( 'NONE', *, *, #3799, .F. ) ;
#9993 = VERTEX_POINT ( 'NONE', #22313 ) ;
#9994 = CARTESIAN_POINT ( 'NONE',  ( 51.45655683570191741, -0.9591657938390835136, -1.468576096419531574 ) ) ;
#9995 = CARTESIAN_POINT ( 'NONE',  ( 22.54717926605048106, 7.740376438784041468, -1.425000000000078204 ) ) ;
#9996 = VERTEX_POINT ( 'NONE', #27504 ) ;
#9997 = CARTESIAN_POINT ( 'NONE',  ( -77.29999999999998295, 0.4498604391086670762, 0.01120648584322036373 ) ) ;
#9998 = FACE_OUTER_BOUND ( 'NONE', #12217, .T. ) ;
#9999 = AXIS2_PLACEMENT_3D ( 'NONE', #2671, #12466, #29269 ) ;
#10000 = DIRECTION ( 'NONE',  ( 1.000000000000000000, 0.000000000000000000, -4.738179285253022937E-16 ) ) ;
#10001 = VERTEX_POINT ( 'NONE', #29273 ) ;
#10002 = SHAPE_REPRESENTATION_RELATIONSHIP ( 'NONE' , 'NONE' ,  #15725, #28934 ) ;
#10003 = AXIS2_PLACEMENT_3D ( 'NONE', #8684, #6317, #4248 ) ;
#10004 = EDGE_CURVE ( 'NONE', #1074, #6162, #14843, .T. ) ;
#10005 = CARTESIAN_POINT ( 'NONE',  ( 58.72427158855720108, -1.357477749119001098, -1.293556822994985422 ) ) ;
#10006 =( BOUNDED_SURFACE ( )  B_SPLINE_SURFACE ( 3, 2, ( 
 ( #14219, #10104, #3283 ),
 ( #12928, #10718, #29553 ),
 ( #2978, #24958, #7717 ),
 ( #22154, #15642, #22450 ),
 ( #27198, #25127, #22620 ),
 ( #8192, #19922, #22778 ) ),
 .UNSPECIFIED., .F., .F., .F. ) 
 B_SPLINE_SURFACE_WITH_KNOTS ( ( 4, 2, 4 ),
 ( 3, 3 ),
 ( -5.854691731421723944E-18, 0.0002091250881941168597, 0.0004182501763882395742 ),
 ( 0.000000000000000000, 1.000000000000000000 ),
 .UNSPECIFIED. ) 
 GEOMETRIC_REPRESENTATION_ITEM ( )  RATIONAL_B_SPLINE_SURFACE ( (
 ( 1.000000000000000000, 0.8366600265340757847, 1.000000000000000000),
 ( 1.000000000000000000, 0.8366252886217447893, 1.000000000000000000),
 ( 1.000000000000000000, 0.8275698663184574144, 1.000000000000000000),
 ( 1.000000000000000000, 0.7855086314083459254, 1.000000000000000000),
 ( 1.000000000000000000, 0.7518972359450074583, 1.000000000000000000),
 ( 1.000000000000000000, 0.7071067811865494601, 1.000000000000000000) ) ) 
 REPRESENTATION_ITEM ( '' )  SURFACE ( )  );
#10007 = AXIS2_PLACEMENT_3D ( 'NONE', #21139, #1777, #8181 ) ;
#10008 = VERTEX_POINT ( 'NONE', #27359 ) ;
#10009 = AXIS2_PLACEMENT_3D ( 'NONE', #29232, #5299, #14957 ) ;
#10010 = CARTESIAN_POINT ( 'NONE',  ( -56.88452994616205416, -3.117691453623976816, 1.799999999999785993 ) ) ;
#10011 = DIRECTION ( 'NONE',  ( 0.000000000000000000, 0.000000000000000000, 1.000000000000000000 ) ) ;
#10012 = CYLINDRICAL_SURFACE ( 'NONE', #15163, 0.2500000000000000000 ) ;
#10013 = CARTESIAN_POINT ( 'NONE',  ( 51.87765138016309407, 8.698644590117595499, 2.049999999999819522 ) ) ;
#10014 = EDGE_CURVE ( 'NONE', #7506, #19797, #15033, .T. ) ;
#10015 = DIRECTION ( 'NONE',  ( 0.000000000000000000, 0.000000000000000000, 1.000000000000000000 ) ) ;
#10016 = CARTESIAN_POINT ( 'NONE',  ( -58.64405989232411542, 2.944486372867117563, -1.700000000000176259 ) ) ;
#10018 = CARTESIAN_POINT ( 'NONE',  ( -36.38139716712170468, 1.027070083876471474, -5.312835761376594412 ) ) ;
#10017 = CARTESIAN_POINT ( 'NONE',  ( 51.13989201884562874, -0.9305404255926473800, -1.499649012356343958 ) ) ;
#10019 = AXIS2_PLACEMENT_3D ( 'NONE', #28565, #12107, #14309 ) ;
#10020 = CARTESIAN_POINT ( 'NONE',  ( 61.25000000000004263, -1.996089927833272881, -0.1249999999999982098 ) ) ;
#10021 = CARTESIAN_POINT ( 'NONE',  ( 54.50000000000002132, -0.003244837758069130020, -4.274998768541101057 ) ) ;
#10023 = DIRECTION ( 'NONE',  ( -1.000000000000000000, -3.054025858079668409E-16, 2.042474015755241579E-16 ) ) ;
#10022 = DIRECTION ( 'NONE',  ( 1.000000000000000000, 1.047444401652940007E-14, 0.000000000000000000 ) ) ;
#10024 = ORIENTED_EDGE ( 'NONE', *, *, #8633, .T. ) ;
#10025 = EDGE_CURVE ( 'NONE', #28152, #24203, #8047, .T. ) ;
#10027 = CARTESIAN_POINT ( 'NONE',  ( -57.77499999999997016, 0.9643027244899933237, -4.702139965541347166 ) ) ;
#10026 = VECTOR ( 'NONE', #4746, 1000.000000000000000 ) ;
#10028 = EDGE_CURVE ( 'NONE', #31243, #26954, #1889, .T. ) ;
#10029 = DIRECTION ( 'NONE',  ( -1.000000000000000000, 1.219044193948983948E-29, -3.491481338843133355E-15 ) ) ;
#10030 = CARTESIAN_POINT ( 'NONE',  ( 52.56231129345008668, 3.962517867693161833, -1.055249607820919699 ) ) ;
#10032 = EDGE_CURVE ( 'NONE', #18916, #10683, #18603, .T. ) ;
#10031 = CARTESIAN_POINT ( 'NONE',  ( 48.00000000000002842, -4.319730106884874132, 1.256953381662069269 ) ) ;
#10033 = EDGE_LOOP ( 'NONE', ( #1515, #8726, #16250, #2271, #6408, #15125, #21452, #29258, #16520 ) ) ;
#10034 = CARTESIAN_POINT ( 'NONE',  ( 51.36685778188466855, 1.002608958138272444, 1.584424273060086152 ) ) ;
#10035 = ORIENTED_EDGE ( 'NONE', *, *, #1434, .T. ) ;
#10036 = ORIENTED_EDGE ( 'NONE', *, *, #14612, .T. ) ;
#10037 = DIRECTION ( 'NONE',  ( -2.117927888850090838E-16, 0.02490330187381123786, -0.9996898646859343485 ) ) ;
#10038 = VERTEX_POINT ( 'NONE', #26885 ) ;
#10039 = CARTESIAN_POINT ( 'NONE',  ( 52.00246240784254326, 4.370935999631933910, 1.433537180069559103 ) ) ;
#10040 = CARTESIAN_POINT ( 'NONE',  ( -54.39405989232412253, -2.944486372867076263, -1.700000000000203793 ) ) ;
#10041 = ORIENTED_EDGE ( 'NONE', *, *, #7588, .F. ) ;
#10042 = DIRECTION ( 'NONE',  ( 0.000000000000000000, 0.000000000000000000, -1.000000000000000000 ) ) ;
#10043 = DIRECTION ( 'NONE',  ( 0.000000000000000000, 0.000000000000000000, 1.000000000000000000 ) ) ;
#10044 = CARTESIAN_POINT ( 'NONE',  ( 25.99900894223690173, 5.212247164669934207, 2.050000000000039790 ) ) ;
#10045 = ORIENTED_EDGE ( 'NONE', *, *, #18205, .T. ) ;
#10046 = CIRCLE ( 'NONE', #7517, 4.199999999999993072 ) ;
#10047 = CARTESIAN_POINT ( 'NONE',  ( -59.23418654921033522, -3.153953023162030078, 1.269874138521803975 ) ) ;
#10048 = CARTESIAN_POINT ( 'NONE',  ( -54.48478889579405404, -1.513794642953540048, 4.039462313877656641 ) ) ;
#10049 = DIRECTION ( 'NONE',  ( 1.047444401652940007E-14, 0.000000000000000000, 1.000000000000000000 ) ) ;
#10050 = DIRECTION ( 'NONE',  ( -1.000000000000000000, -2.586136946169074517E-16, 0.000000000000000000 ) ) ;
#10051 = EDGE_CURVE ( 'NONE', #18759, #25939, #18085, .T. ) ;
#10052 = CARTESIAN_POINT ( 'NONE',  ( 57.00303004862897183, 0.7171412854886025645, 2.441992855427530085 ) ) ;
#10053 = ADVANCED_FACE ( 'NONE', ( #449 ), #8461, .T. ) ;
#10054 = LINE ( 'NONE', #19724, #31092 ) ;
#10055 = CARTESIAN_POINT ( 'NONE',  ( -59.69999999999997442, 3.166389444283797872, -1.238538609462263462 ) ) ;
#10056 = CARTESIAN_POINT ( 'NONE',  ( 15.03925126672133139, -3.817150320980667200, 2.203324261490537062 ) ) ;
#10057 = DIRECTION ( 'NONE',  ( 0.000000000000000000, -1.000000000000000000, -3.491481338843133355E-15 ) ) ;
#10058 = ORIENTED_EDGE ( 'NONE', *, *, #26681, .T. ) ;
#10059 = EDGE_CURVE ( 'NONE', #7802, #1825, #22091, .T. ) ;
#10060 = VERTEX_POINT ( 'NONE', #17385 ) ;
#10061 = AXIS2_PLACEMENT_3D ( 'NONE', #27048, #19337, #5532 ) ;
#10062 = ORIENTED_EDGE ( 'NONE', *, *, #3473, .F. ) ;
#10063 = CYLINDRICAL_SURFACE ( 'NONE', #11863, 0.1000000000000000472 ) ;
#10064 = CARTESIAN_POINT ( 'NONE',  ( -57.79792740578359656, -2.256877952708263635, 2.542931754211924744 ) ) ;
#10066 = CARTESIAN_POINT ( 'NONE',  ( 51.89161117884415120, 9.098400920926795976, 1.949999999999818767 ) ) ;
#10065 = CARTESIAN_POINT ( 'NONE',  ( -54.74999999999997868, -2.944486372867089141, 1.699999999999794342 ) ) ;
#10067 = ORIENTED_EDGE ( 'NONE', *, *, #29901, .T. ) ;
#10068 = ORIENTED_EDGE ( 'NONE', *, *, #13354, .F. ) ;
#10069 = CARTESIAN_POINT ( 'NONE',  ( 53.96114054633191870, 6.379383430131290389, -1.889921144916990592 ) ) ;
#10070 = ORIENTED_EDGE ( 'NONE', *, *, #7666, .T. ) ;
#10071 = CARTESIAN_POINT ( 'NONE',  ( 51.25000000000002842, -1.099999999999462963, -1.996089927833914146 ) ) ;
#10072 = ORIENTED_EDGE ( 'NONE', *, *, #24374, .T. ) ;
#10073 = CARTESIAN_POINT ( 'NONE',  ( 31.37624803156776565, 7.388935656075756420, -2.050000000000107292 ) ) ;
#10074 = VERTEX_POINT ( 'NONE', #5668 ) ;
#10075 = DIRECTION ( 'NONE',  ( -3.491481338843133355E-15, -3.491481338843133355E-15, 1.000000000000000000 ) ) ;
#10076 = AXIS2_PLACEMENT_3D ( 'NONE', #24938, #3719, #29858 ) ;
#10077 = CARTESIAN_POINT ( 'NONE',  ( -59.69999999999997442, 8.366749974758454467E-15, -2.120534355533670266E-13 ) ) ;
#10078 = CARTESIAN_POINT ( 'NONE',  ( 15.57907767661739840, -4.962973169597029610, -2.162832296644437768 ) ) ;
#10079 = CARTESIAN_POINT ( 'NONE',  ( -56.51905989232411542, 2.023778652682506843E-14, -3.400000000000200640 ) ) ;
#10080 = CARTESIAN_POINT ( 'NONE',  ( 51.97945110550962511, 4.337541896208987779, -2.050000000000180567 ) ) ;
#10081 = ADVANCED_FACE ( 'NONE', ( #27031 ), #12495, .F. ) ;
#10082 = MECHANICAL_DESIGN_GEOMETRIC_PRESENTATION_REPRESENTATION (  '', ( #29806 ), #9604 ) ;
#10083 = EDGE_CURVE ( 'NONE', #31077, #14916, #28357, .T. ) ;
#10084 = VECTOR ( 'NONE', #29182, 1000.000000000000000 ) ;
#10085 = ADVANCED_FACE ( 'NONE', ( #16687 ), #2251, .T. ) ;
#10086 = CYLINDRICAL_SURFACE ( 'NONE', #1333, 0.1500000000000001887 ) ;
#10087 = CARTESIAN_POINT ( 'NONE',  ( 58.65000000000001990, 6.143261415694495821E-13, 3.111507638930570854E-58 ) ) ;
#10088 = CARTESIAN_POINT ( 'NONE',  ( 16.10660252424457894, -5.231589534716065693, -1.397536681175223228 ) ) ;
#10089 = CARTESIAN_POINT ( 'NONE',  ( 50.50000000000002132, 0.6304760106459519342, -3.950000000000022826 ) ) ;
#10090 = ORIENTED_EDGE ( 'NONE', *, *, #19886, .F. ) ;
#10091 = DIRECTION ( 'NONE',  ( 0.000000000000000000, 1.776356839400250465E-15, 1.000000000000000000 ) ) ;
#10092 = CARTESIAN_POINT ( 'NONE',  ( -36.30424252565893539, -2.966783028120398846, -4.272059443775234833 ) ) ;
#10093 = FACE_OUTER_BOUND ( 'NONE', #11894, .T. ) ;
#10094 = VERTEX_POINT ( 'NONE', #9390 ) ;
#10095 = EDGE_CURVE ( 'NONE', #20372, #28072, #23806, .T. ) ;
#10096 = CARTESIAN_POINT ( 'NONE',  ( 50.50000000000002132, 0.7901969350670130510, -4.025772098418840983 ) ) ;
#10097 = AXIS2_PLACEMENT_3D ( 'NONE', #16447, #31006, #30861 ) ;
#10098 = ORIENTED_EDGE ( 'NONE', *, *, #1087, .F. ) ;
#10099 = SURFACE_SIDE_STYLE ('',( #2802 ) ) ;
#10100 = CARTESIAN_POINT ( 'NONE',  ( -36.04518387042616467, -4.861582133259191529, 2.394243994563265865 ) ) ;
#10102 = CARTESIAN_POINT ( 'NONE',  ( -62.08887962957128792, -2.673162175134213392, -0.3797419985091401440 ) ) ;
#10101 = CARTESIAN_POINT ( 'NONE',  ( 51.67801394174050955, -4.132863666287244442, 2.022846738276933287 ) ) ;
#10103 = EDGE_LOOP ( 'NONE', ( #17312, #25549, #10036, #26150, #7834, #28688, #21224, #13672 ) ) ;
#10104 = CARTESIAN_POINT ( 'NONE',  ( 60.75000000000002842, -0.4999999999993641198, -1.554802467931445609 ) ) ;
#10105 = AXIS2_PLACEMENT_3D ( 'NONE', #27997, #8532, #18218 ) ;
#10106 = DIRECTION ( 'NONE',  ( 0.000000000000000000, 0.1576190026614809614, 0.9875000000000001554 ) ) ;
#10107 = AXIS2_PLACEMENT_3D ( 'NONE', #31058, #6842, #9845 ) ;
#10109 = DIRECTION ( 'NONE',  ( 0.000000000000000000, 0.000000000000000000, -1.000000000000000000 ) ) ;
#10108 = DIRECTION ( 'NONE',  ( 0.000000000000000000, -0.9996898646859344595, -0.02490330187381131419 ) ) ;
#10110 = DIRECTION ( 'NONE',  ( 0.000000000000000000, -0.9663289263986323263, -0.2573099415204678220 ) ) ;
#10111 = CARTESIAN_POINT ( 'NONE',  ( -59.43749999999997158, -4.108500314926507357, 1.367561758111406789 ) ) ;
#10112 = CARTESIAN_POINT ( 'NONE',  ( -55.84599364905386665, 3.400000000000011902, -0.9110272542660028394 ) ) ;
#10113 = CARTESIAN_POINT ( 'NONE',  ( 15.18463186935388087, -2.199885893005466553, -4.939696249117980997 ) ) ;
#10114 = CIRCLE ( 'NONE', #8079, 1.524417381223824197 ) ;
#10115 = CARTESIAN_POINT ( 'NONE',  ( -61.61493949811855231, -2.643639042166195274, -0.5548158911668893412 ) ) ;
#10116 = CARTESIAN_POINT ( 'NONE',  ( 53.91574522233626965, 6.672251602764244893, -1.774295313897662485 ) ) ;
#10117 = CARTESIAN_POINT ( 'NONE',  ( -61.34999999999997300, -2.574153985709302539, -0.5872647410103332133 ) ) ;
#10118 = CARTESIAN_POINT ( 'NONE',  ( 58.65000000000000568, 1.253243060177670287, 1.394635017528978782 ) ) ;
#10119 = ORIENTED_EDGE ( 'NONE', *, *, #30959, .T. ) ;
#10120 = EDGE_CURVE ( 'NONE', #11926, #21490, #24189, .T. ) ;
#10121 = EDGE_CURVE ( 'NONE', #27460, #21323, #30644, .T. ) ;
#10122 = DIRECTION ( 'NONE',  ( 0.000000000000000000, 0.000000000000000000, 1.000000000000000000 ) ) ;
#10123 = DIRECTION ( 'NONE',  ( 0.000000000000000000, 1.000000000000000000, 3.491481338843130594E-15 ) ) ;
#10124 = DIRECTION ( 'NONE',  ( 0.000000000000000000, 0.000000000000000000, 1.000000000000000000 ) ) ;
#10126 = AXIS2_PLACEMENT_3D ( 'NONE', #23357, #20979, #8162 ) ;
#10125 = DIRECTION ( 'NONE',  ( 1.000000000000000000, 3.053848253006669023E-16, -2.042510438544995415E-16 ) ) ;
#10128 = CARTESIAN_POINT ( 'NONE',  ( 28.86359278493675973, 5.838313002610194147, 1.424999999999899902 ) ) ;
#10127 = CARTESIAN_POINT ( 'NONE',  ( 51.23644008536122385, 1.080112125196981854, 1.214076932077872817 ) ) ;
#10129 = ORIENTED_EDGE ( 'NONE', *, *, #10121, .F. ) ;
#10130 = ADVANCED_FACE ( 'NONE', ( #30921 ), #21601, .T. ) ;
#10131 = CARTESIAN_POINT ( 'NONE',  ( 58.75000000000000711, 1.039502773797200019, -1.800471618823823450 ) ) ;
#10132 = ORIENTED_EDGE ( 'NONE', *, *, #3888, .T. ) ;
#10133 = UNCERTAINTY_MEASURE_WITH_UNIT (LENGTH_MEASURE( 1.000000000000000082E-05 ), #18108, 'distance_accuracy_value', 'NONE');
#10134 = CARTESIAN_POINT ( 'NONE',  ( 51.80000000000001137, 4.350000000000017408, -1.550321101314903194 ) ) ;
#10136 = CARTESIAN_POINT ( 'NONE',  ( -71.44999999999998863, 0.2962051453644842236, -1.444357686279446273 ) ) ;
#10135 = CARTESIAN_POINT ( 'NONE',  ( 57.00174889577907322, 0.7131084301676396953, -2.444403622924161912 ) ) ;
#10137 = CARTESIAN_POINT ( 'NONE',  ( -67.33025350686975230, -4.292234512154642818E-16, 3.266011492503604425E-15 ) ) ;
#10138 = ORIENTED_EDGE ( 'NONE', *, *, #10004, .T. ) ;
#10139 = ORIENTED_EDGE ( 'NONE', *, *, #11711, .T. ) ;
#10140 = CARTESIAN_POINT ( 'NONE',  ( 52.20711756518984714, -0.6499999999994534594, -1.489337100860648189 ) ) ;
#10141 = DIRECTION ( 'NONE',  ( 1.000000000000000000, 1.047444401652940007E-14, 0.000000000000000000 ) ) ;
#10142 = VERTEX_POINT ( 'NONE', #19060 ) ;
#10143 = CARTESIAN_POINT ( 'NONE',  ( -59.18987816865176654, 2.399875262006965215, 1.250136525132548915 ) ) ;
#10144 =( BOUNDED_CURVE ( )  B_SPLINE_CURVE ( 2, ( #5364, #22175, #161, #19792, #19482, #9677, #29426, #15025, #24686 ),
 .UNSPECIFIED., .F., .T. ) 
 B_SPLINE_CURVE_WITH_KNOTS ( ( 3, 2, 2, 2, 3 ),
 ( 0.3055555555555555802, 0.3148148148148148251, 0.3333333333333333148, 0.3518518518518518601, 0.3611111111111111605 ),
 .UNSPECIFIED. ) 
 CURVE ( )  GEOMETRIC_REPRESENTATION_ITEM ( )  RATIONAL_B_SPLINE_CURVE ( ( 0.9330127018922194093, 0.9330127018922195203, 1.000000000000000000, 0.8660254037844387076, 1.000000000000000000, 0.8660254037844387076, 1.000000000000000000, 0.9330127018922189652, 0.9330127018922194093 ) ) 
 REPRESENTATION_ITEM ( '' )  );
#10145 = CARTESIAN_POINT ( 'NONE',  ( 58.45000000000001705, -0.8000000000000000444, -2.471260002560650371 ) ) ;
#10146 = CARTESIAN_POINT ( 'NONE',  ( -36.58361892166016816, -5.175840503946164795, -1.569056257078813355 ) ) ;
#10147 = ORIENTED_EDGE ( 'NONE', *, *, #6616, .T. ) ;
#10148 = CARTESIAN_POINT ( 'NONE',  ( -59.29999999999996874, -2.718478022535892880, -2.574424139164518621 ) ) ;
#10149 = EDGE_LOOP ( 'NONE', ( #15248, #20159, #24888, #25915 ) ) ;
#10150 = B_SPLINE_CURVE_WITH_KNOTS ( 'NONE', 3,
 ( #27453, #7103, #9648, #22404, #14533, #28792, #5619, #7407, #10529, #24770, #19301, #20202, #13048, #28937, #29833, #8143, #10354, #9781, #20030 ),
 .UNSPECIFIED., .F., .F.,
 ( 4, 3, 3, 3, 3, 3, 4 ),
 ( 0.000000000000000000, 1.485152479261661559E-05, 2.963899638137941126E-05, 4.531421101975836217E-05, 6.339282692920784022E-05, 8.412900350910327988E-05, 8.561427748423850544E-05 ),
 .UNSPECIFIED. ) ;
#10151 = ADVANCED_FACE ( 'NONE', ( #1770 ), #6850, .F. ) ;
#10152 = CARTESIAN_POINT ( 'NONE',  ( -58.32202994616204705, -4.156921938165296204, -2.220106322563329850E-13 ) ) ;
#10153 = CARTESIAN_POINT ( 'NONE',  ( 48.46244267249164039, -1.426738769040753363, -3.843750315111145621 ) ) ;
#10154 = DIRECTION ( 'NONE',  ( -1.000000000000000000, 0.000000000000000000, 0.000000000000000000 ) ) ;
#10155 = CARTESIAN_POINT ( 'NONE',  ( 51.80639759064268191, -4.235057606083633353, -1.098058400101913357 ) ) ;
#10156 = CARTESIAN_POINT ( 'NONE',  ( -56.74005354137802470, -3.399999999999994138, 0.9110272542655987182 ) ) ;
#10158 = DIRECTION ( 'NONE',  ( -1.000000000000000000, -4.939082069373447378E-17, -1.520093157366847861E-16 ) ) ;
#10157 = DIRECTION ( 'NONE',  ( 0.000000000000000000, -0.2008964009354162750, 0.9796124928211136229 ) ) ;
#10159 = CARTESIAN_POINT ( 'NONE',  ( 69.05000000000002558, 4.557543281186736018E-17, -7.232603593413552923E-13 ) ) ;
#10160 = CARTESIAN_POINT ( 'NONE',  ( 16.10667815269232861, -3.294441450831202101, 4.290383166762130607 ) ) ;
#10162 = CARTESIAN_POINT ( 'NONE',  ( 51.25000000000001421, 1.100000000000537215, -1.196087371390568643 ) ) ;
#10161 = FACE_OUTER_BOUND ( 'NONE', #9441, .T. ) ;
#10163 = ORIENTED_EDGE ( 'NONE', *, *, #11765, .T. ) ;
#10164 = ADVANCED_FACE ( 'NONE', ( #13959 ), #9712, .T. ) ;
#10165 = CARTESIAN_POINT ( 'NONE',  ( 50.45688046812396976, -1.211457450596347352, -3.917546004217186351 ) ) ;
#10166 = DIRECTION ( 'NONE',  ( 0.000000000000000000, 1.000000000000000000, 3.491481338843137694E-15 ) ) ;
#10168 = CARTESIAN_POINT ( 'NONE',  ( 52.89380626919926698, 4.088132893582258731, -0.3545262462039958096 ) ) ;
#10167 = CARTESIAN_POINT ( 'NONE',  ( 15.03925126672132961, 2.199885893006009674, -4.939696249117653259 ) ) ;
#10169 = CARTESIAN_POINT ( 'NONE',  ( 56.95000000000001705, 0.7137254901960795594, 2.500119182087999103 ) ) ;
#10170 = ORIENTED_EDGE ( 'NONE', *, *, #17913, .T. ) ;
#10171 = CARTESIAN_POINT ( 'NONE',  ( -61.35985865640643055, -2.638419680335174267, 0.4713968906680494064 ) ) ;
#10172 = ORIENTED_EDGE ( 'NONE', *, *, #24864, .F. ) ;
#10173 = DIRECTION ( 'NONE',  ( 2.117927888850090591E-16, -0.02490330187381111643, 0.9996898646859343485 ) ) ;
#10175 = ORIENTED_EDGE ( 'NONE', *, *, #21836, .T. ) ;
#10174 = B_SPLINE_CURVE_WITH_KNOTS ( 'NONE', 3,
 ( #20875, #30504, #18500, #16278 ),
 .UNSPECIFIED., .F., .F.,
 ( 4, 4 ),
 ( 0.0001956043251250877066, 0.0003834565248886559865 ),
 .UNSPECIFIED. ) ;
#10176 = EDGE_CURVE ( 'NONE', #1297, #8161, #18034, .T. ) ;
#10177 = ORIENTED_EDGE ( 'NONE', *, *, #3230, .F. ) ;
#10178 = CARTESIAN_POINT ( 'NONE',  ( -60.54999999999995453, 0.7328781032566589193, -3.573665542649862914 ) ) ;
#10179 = ORIENTED_EDGE ( 'NONE', *, *, #6839, .T. ) ;
#10180 = CARTESIAN_POINT ( 'NONE',  ( -35.85663232820583346, -3.817150320980530864, 2.203324261490918090 ) ) ;
#10181 = CARTESIAN_POINT ( 'NONE',  ( -58.88452994616202574, 2.093608279459372350E-14, -3.600000000000208811 ) ) ;
#10182 = ORIENTED_EDGE ( 'NONE', *, *, #23686, .F. ) ;
#10183 = CARTESIAN_POINT ( 'NONE',  ( 54.49508724208691746, -0.002176679993770252661, 4.307918145378301311 ) ) ;
#10184 = CARTESIAN_POINT ( 'NONE',  ( 58.75000000000003553, -1.972190280207336555, -0.1053114364790862928 ) ) ;
#10185 = DIRECTION ( 'NONE',  ( 0.000000000000000000, 0.000000000000000000, -1.000000000000000000 ) ) ;
#10186 = VERTEX_POINT ( 'NONE', #7025 ) ;
#10187 = CIRCLE ( 'NONE', #18294, 0.04999999999999988481 ) ;
#10188 = EDGE_CURVE ( 'NONE', #23309, #25954, #17025, .T. ) ;
#10189 = CARTESIAN_POINT ( 'NONE',  ( 51.73251178704410336, -4.176834854957373722, -1.005432649909180576 ) ) ;
#10190 = EDGE_CURVE ( 'NONE', #4801, #1976, #23657, .T. ) ;
#10191 = CARTESIAN_POINT ( 'NONE',  ( -54.47710365256552478, -1.507983431629474014, 4.035431478432993657 ) ) ;
#10192 = CYLINDRICAL_SURFACE ( 'NONE', #2619, 0.05000000000000143219 ) ;
#10194 = EDGE_CURVE ( 'NONE', #9911, #11417, #13449, .T. ) ;
#10193 = CARTESIAN_POINT ( 'NONE',  ( 50.30000000000001847, 1.391941090707534023, 3.750000000000022649 ) ) ;
#10195 = CARTESIAN_POINT ( 'NONE',  ( -68.01382336603234080, -0.6601810586021509275, 3.219179684251519458 ) ) ;
#10196 =( REPRESENTATION_RELATIONSHIP ('NONE','NONE', #7047, #549 ) REPRESENTATION_RELATIONSHIP_WITH_TRANSFORMATION ( #11559 )SHAPE_REPRESENTATION_RELATIONSHIP( ) );
#10198 = CARTESIAN_POINT ( 'NONE',  ( 51.80000000000001847, 1.521694824349982378, -3.995005614707754393 ) ) ;
#10197 = PLANE ( 'NONE',  #10454 ) ;
#10199 = CARTESIAN_POINT ( 'NONE',  ( 36.50000000000002132, 0.000000000000000000, 0.000000000000000000 ) ) ;
#10200 = CARTESIAN_POINT ( 'NONE',  ( 58.64999999999999858, 1.874116925335308714, 0.06656272211392090521 ) ) ;
#10201 = CARTESIAN_POINT ( 'NONE',  ( 58.72200624034157812, 1.341335979948039547, -1.310319377727088064 ) ) ;
#10202 = LINE ( 'NONE', #19871, #5174 ) ;
#10203 = EDGE_LOOP ( 'NONE', ( #5470, #17178, #15630, #4170 ) ) ;
#10204 = CIRCLE ( 'NONE', #1604, 3.075000000000000622 ) ;
#10205 = VERTEX_POINT ( 'NONE', #26478 ) ;
#10206 = CIRCLE ( 'NONE', #8682, 0.4400000000000000577 ) ;
#10207 = ORIENTED_EDGE ( 'NONE', *, *, #18345, .F. ) ;
#10208 = DIRECTION ( 'NONE',  ( 0.000000000000000000, 0.000000000000000000, 1.000000000000000000 ) ) ;
#10209 = CARTESIAN_POINT ( 'NONE',  ( -58.92292740578360366, 2.256877952708268964, -2.542931754211924744 ) ) ;
#10211 = CARTESIAN_POINT ( 'NONE',  ( 51.45655683570189609, 0.9591657938401613182, -1.611094652690528317 ) ) ;
#10210 = CARTESIAN_POINT ( 'NONE',  ( 15.03925126672133139, -4.383220986679489783, 0.4611378927914256409 ) ) ;
#10212 = VERTEX_POINT ( 'NONE', #24113 ) ;
#10213 = EDGE_CURVE ( 'NONE', #24355, #28012, #11440, .T. ) ;
#10214 = EDGE_LOOP ( 'NONE', ( #10779, #10620, #8604, #1718 ) ) ;
#10215 = CARTESIAN_POINT ( 'NONE',  ( 51.30625150934615419, -4.280436737593984908, -1.378429032882124927 ) ) ;
#10216 = VERTEX_POINT ( 'NONE', #12085 ) ;
#10217 = CARTESIAN_POINT ( 'NONE',  ( 51.70000000000002416, 6.982261990806648555E-14, -1.793082891011605378E-13 ) ) ;
#10218 = VERTEX_POINT ( 'NONE', #21761 ) ;
#10219 = CARTESIAN_POINT ( 'NONE',  ( 29.24156347413317647, 6.028130183538130460, -1.950000000000102984 ) ) ;
#10220 = ADVANCED_FACE ( 'NONE', ( #49 ), #4157, .T. ) ;
#10221 = EDGE_LOOP ( 'NONE', ( #31323, #30998, #7057, #30193, #24945, #16852, #28169, #4250, #14613, #409, #8270, #27244 ) ) ;
#10222 = DIRECTION ( 'NONE',  ( -1.000000000000000000, 0.000000000000000000, 0.000000000000000000 ) ) ;
#10223 = CARTESIAN_POINT ( 'NONE',  ( 54.41366571437522026, 6.718673005292167488, 1.949999999999809663 ) ) ;
#10224 = ORIENTED_EDGE ( 'NONE', *, *, #13059, .F. ) ;
#10225 = CARTESIAN_POINT ( 'NONE',  ( 15.03925126672132961, -5.340403872473328484, -0.9205822173396246422 ) ) ;
#10226 = ADVANCED_FACE ( 'NONE', ( #10310 ), #28655, .T. ) ;
#10227 = CARTESIAN_POINT ( 'NONE',  ( -60.44702994616202574, -2.078460969082631227, -3.600000000000220801 ) ) ;
#10229 = EDGE_CURVE ( 'NONE', #16545, #24817, #22055, .T. ) ;
#10228 = CARTESIAN_POINT ( 'NONE',  ( 53.75840399023271488, 7.746411475361853149, -2.050000000000187228 ) ) ;
#10230 = CARTESIAN_POINT ( 'NONE',  ( 58.64999999999999858, 1.394635017528131904, 1.253243060178682367 ) ) ;
#10231 = DIRECTION ( 'NONE',  ( 1.000000000000000000, 1.047444401652940007E-14, 0.000000000000000000 ) ) ;
#10232 = FACE_OUTER_BOUND ( 'NONE', #20851, .T. ) ;
#10233 = PLANE ( 'NONE',  #4433 ) ;
#10234 = DIRECTION ( 'NONE',  ( 0.000000000000000000, -1.000000000000000000, 0.000000000000000000 ) ) ;
#10235 = DIRECTION ( 'NONE',  ( 3.491481338843133355E-15, 0.000000000000000000, 1.000000000000000000 ) ) ;
#10236 = DIRECTION ( 'NONE',  ( -1.000000000000000000, -1.293068473084537258E-16, -0.000000000000000000 ) ) ;
#10237 = CIRCLE ( 'NONE', #30458, 0.4999999999999996114 ) ;
#10238 = ORIENTED_EDGE ( 'NONE', *, *, #1348, .F. ) ;
#10239 = CARTESIAN_POINT ( 'NONE',  ( -59.29999999999998295, 2.957953439200568635, 2.295354275992711024 ) ) ;
#10240 = LINE ( 'NONE', #26732, #23162 ) ;
#10241 = CARTESIAN_POINT ( 'NONE',  ( 54.40419027210252523, 5.984372876903068850, -1.843143693225357538E-13 ) ) ;
#10242 = ORIENTED_EDGE ( 'NONE', *, *, #12789, .T. ) ;
#10243 = DIRECTION ( 'NONE',  ( 0.000000000000000000, -0.2008964009354147484, 0.9796124928211139560 ) ) ;
#10244 = ORIENTED_EDGE ( 'NONE', *, *, #1669, .T. ) ;
#10245 = CARTESIAN_POINT ( 'NONE',  ( 52.88620718028471401, 4.625382794676526466, 1.578939844535152570 ) ) ;
#10246 = CARTESIAN_POINT ( 'NONE',  ( -55.03335481156724285, 0.8699069336946695374, -4.241846523238430144 ) ) ;
#10248 = CARTESIAN_POINT ( 'NONE',  ( -62.07177862240501298, -2.624829244341188250, -0.3257396798314975417 ) ) ;
#10247 = DIRECTION ( 'NONE',  ( -1.000000000000000000, 0.000000000000000000, 1.047444401652940007E-14 ) ) ;
#10249 = ORIENTED_EDGE ( 'NONE', *, *, #8784, .T. ) ;
#10250 = EDGE_CURVE ( 'NONE', #31043, #19303, #27587, .T. ) ;
#10251 = DIRECTION ( 'NONE',  ( -0.5633368246415186853, 0.8262273428075416204, 0.000000000000000000 ) ) ;
#10252 = EDGE_CURVE ( 'NONE', #12009, #19299, #7775, .T. ) ;
#10253 = CARTESIAN_POINT ( 'NONE',  ( 58.99999999999998579, 1.401298464324817071E-42, -4.000000000000617284 ) ) ;
#10254 = VERTEX_POINT ( 'NONE', #7489 ) ;
#10256 = CARTESIAN_POINT ( 'NONE',  ( -59.69459045457838187, 2.420214307862085246, -1.235415406956913653 ) ) ;
#10255 = DIRECTION ( 'NONE',  ( 2.117927888850091331E-16, -0.02490330187381135929, 0.9996898646859343485 ) ) ;
#10257 = EDGE_CURVE ( 'NONE', #9817, #30573, #20576, .T. ) ;
#10258 = DIRECTION ( 'NONE',  ( -1.000000000000000000, -0.000000000000000000, -0.000000000000000000 ) ) ;
#10259 = CARTESIAN_POINT ( 'NONE',  ( -59.31249999999997158, -3.238593381231841040, -2.874284765127020247 ) ) ;
#10260 = CARTESIAN_POINT ( 'NONE',  ( 56.95000000000001705, -0.6937162836135747357, 1.768873629894432975 ) ) ;
#10261 = CARTESIAN_POINT ( 'NONE',  ( 58.64999999999999858, 1.571497941947157750, -1.022750809561051133 ) ) ;
#10262 = CARTESIAN_POINT ( 'NONE',  ( 47.05963571244991073, 8.266527678078146479, -1.550000000000163469 ) ) ;
#10263 = CARTESIAN_POINT ( 'NONE',  ( -59.69999999999993889, -0.8057164866800677894, -3.484314813711807624 ) ) ;
#10265 = DIRECTION ( 'NONE',  ( 3.489354422748178582E-15, -1.218509414717996338E-16, 1.000000000000000000 ) ) ;
#10264 = CIRCLE ( 'NONE', #28978, 0.1000000000000001998 ) ;
#10266 = DIRECTION ( 'NONE',  ( 1.000000000000000000, -0.000000000000000000, -0.000000000000000000 ) ) ;
#10267 = EDGE_LOOP ( 'NONE', ( #22232, #9095 ) ) ;
#10268 = EDGE_CURVE ( 'NONE', #556, #24802, #26112, .T. ) ;
#10269 = CARTESIAN_POINT ( 'NONE',  ( 15.76623786017564832, 3.091683853622046119, 4.437651790014722764 ) ) ;
#10270 = CYLINDRICAL_SURFACE ( 'NONE', #1797, 3.399999999999999911 ) ;
#10271 = CARTESIAN_POINT ( 'NONE',  ( 53.45668887520044876, 7.806764284940763687, -1.876589106057076295 ) ) ;
#10272 = PRODUCT_DEFINITION ( 'UNKNOWN', '', #13626, #5688 ) ;
#10273 = B_SPLINE_CURVE_WITH_KNOTS ( 'NONE', 3,
 ( #28345, #6651, #16314, #25958, #11085, #13908 ),
 .UNSPECIFIED., .F., .F.,
 ( 4, 2, 4 ),
 ( 0.000000000000000000, 0.0001000270069603067982, 0.0002000540139206135964 ),
 .UNSPECIFIED. ) ;
#10274 = CARTESIAN_POINT ( 'NONE',  ( -36.11122220296836360, 4.822476035523766136, -1.985498375066671262 ) ) ;
#10275 = CARTESIAN_POINT ( 'NONE',  ( -59.29999999999997584, -0.7533615035078030653, 3.673546848079178417 ) ) ;
#10276 = CARTESIAN_POINT ( 'NONE',  ( 31.71090952588640732, 7.663588669452821911, 2.049999999999887912 ) ) ;
#10277 = ORIENTED_EDGE ( 'NONE', *, *, #9991, .T. ) ;
#10278 = CARTESIAN_POINT ( 'NONE',  ( -63.82928932188132620, -2.699162634652022330, -0.06723891505928762669 ) ) ;
#10279 = ORIENTED_EDGE ( 'NONE', *, *, #19396, .T. ) ;
#10280 = DIRECTION ( 'NONE',  ( 1.000000000000000000, 1.047444401652940007E-14, -0.000000000000000000 ) ) ;
#10281 = AXIS2_PLACEMENT_3D ( 'NONE', #6164, #3626, #13258 ) ;
#10283 = DIRECTION ( 'NONE',  ( 0.000000000000000000, -1.000000000000000000, 0.000000000000000000 ) ) ;
#10282 = CARTESIAN_POINT ( 'NONE',  ( 15.22842924604238313, -3.779372845004303372, -3.883777290284644579 ) ) ;
#10284 = CIRCLE ( 'NONE', #5747, 2.649999999999999911 ) ;
#10285 = ORIENTED_EDGE ( 'NONE', *, *, #28454, .F. ) ;
#10286 = VERTEX_POINT ( 'NONE', #17443 ) ;
#10287 = DIRECTION ( 'NONE',  ( 3.002035892788116966E-16, -0.9996898646859343485, -0.02490330187381123786 ) ) ;
#10288 = EDGE_CURVE ( 'NONE', #12947, #15675, #25084, .T. ) ;
#10289 = CARTESIAN_POINT ( 'NONE',  ( 51.84831113588973039, 0.6920605891666480325, 1.653603923793167674 ) ) ;
#10290 = ORIENTED_EDGE ( 'NONE', *, *, #20931, .T. ) ;
#10292 = CARTESIAN_POINT ( 'NONE',  ( 56.99139336475067807, -0.7078862301243328270, -1.763423818528686349 ) ) ;
#10291 = CARTESIAN_POINT ( 'NONE',  ( -59.57202994616203995, 2.078460969082674747, -3.600000000000202593 ) ) ;
#10293 = DIRECTION ( 'NONE',  ( 2.614375865348240525E-16, -0.2008964009354147762, 0.9796124928211140670 ) ) ;
#10294 = CARTESIAN_POINT ( 'NONE',  ( -36.30424252565903487, -4.911231426340521011, -1.712337380313407209 ) ) ;
#10295 = APPLICATION_PROTOCOL_DEFINITION ( 'draft international standard', 'automotive_design', 1998, #30768 ) ;
#10296 = CARTESIAN_POINT ( 'NONE',  ( -54.44999999999997442, 0.000000000000000000, 2.168404344971008868E-14 ) ) ;
#10297 = VERTEX_POINT ( 'NONE', #19687 ) ;
#10298 = EDGE_CURVE ( 'NONE', #26730, #27342, #24723, .T. ) ;
#10299 = CARTESIAN_POINT ( 'NONE',  ( -59.13452994616204705, -3.117691453623976816, 1.799999999999778000 ) ) ;
#10300 = CARTESIAN_POINT ( 'NONE',  ( 52.88620718028472822, 4.625382794676503373, -2.050000000000184119 ) ) ;
#10301 = DIRECTION ( 'NONE',  ( -1.000000000000000000, -3.053848253006669023E-16, 2.042510438544995415E-16 ) ) ;
#10302 = AXIS2_PLACEMENT_3D ( 'NONE', #21338, #6909, #2145 ) ;
#10303 = CARTESIAN_POINT ( 'NONE',  ( 16.07512358269906372, 0.3169205264062135985, 5.400007398663869473 ) ) ;
#10304 = CARTESIAN_POINT ( 'NONE',  ( 51.06302884844836143, -4.023893809447297798, 1.198232146805239928 ) ) ;
#10305 = FACE_OUTER_BOUND ( 'NONE', #17970, .T. ) ;
#10307 = CARTESIAN_POINT ( 'NONE',  ( -36.50489844130334660, -0.3564988296781614885, -5.398869307934827333 ) ) ;
#10306 = CARTESIAN_POINT ( 'NONE',  ( 26.19155409318043226, 5.638511060912941630, -1.425000000000091305 ) ) ;
#10308 = PRODUCT ( 'End Cap Ring', 'End Cap Ring', '', ( #6033 ) ) ;
#10309 = CARTESIAN_POINT ( 'NONE',  ( -62.09889467716561740, -2.519749790771223630, 0.1627451747621806999 ) ) ;
#10310 = FACE_OUTER_BOUND ( 'NONE', #8325, .T. ) ;
#10312 = DIRECTION ( 'NONE',  ( 1.047444401652940007E-14, 0.000000000000000000, 1.000000000000000000 ) ) ;
#10311 = FACE_OUTER_BOUND ( 'NONE', #29203, .T. ) ;
#10313 = ORIENTED_EDGE ( 'NONE', *, *, #11746, .T. ) ;
#10314 = DIRECTION ( 'NONE',  ( 0.000000000000000000, 0.000000000000000000, 1.000000000000000000 ) ) ;
#10315 =( BOUNDED_CURVE ( )  B_SPLINE_CURVE ( 2, ( #30660, #6141, #8656, #23394, #18336, #27972, #25595, #1534, #11193 ),
 .UNSPECIFIED., .F., .T. ) 
 B_SPLINE_CURVE_WITH_KNOTS ( ( 3, 2, 2, 2, 3 ),
 ( 0.2500000000000000000, 0.2592592592592592449, 0.2777777777777777901, 0.2962962962962962798, 0.3055555555555555802 ),
 .UNSPECIFIED. ) 
 CURVE ( )  GEOMETRIC_REPRESENTATION_ITEM ( )  RATIONAL_B_SPLINE_CURVE ( ( 0.9330127018922192983, 0.9330127018922194093, 1.000000000000000000, 0.8660254037844387076, 1.000000000000000000, 0.8660254037844387076, 1.000000000000000000, 0.9330127018922191873, 0.9330127018922194093 ) ) 
 REPRESENTATION_ITEM ( '' )  );
#10316 = DIRECTION ( 'NONE',  ( 0.9396926207859097602, -0.008517430876162936787, 0.3419140708010978136 ) ) ;
#10318 = CARTESIAN_POINT ( 'NONE',  ( 51.80000000000001137, 6.475000000000062705, -2.050000000000180123 ) ) ;
#10317 = CARTESIAN_POINT ( 'NONE',  ( 15.94709373951304698, 3.646691605040303763, -3.993181011920754475 ) ) ;
#10319 = CARTESIAN_POINT ( 'NONE',  ( 47.49374849065389270, -4.280436737593935170, 1.378429032881762994 ) ) ;
#10320 = ORIENTED_EDGE ( 'NONE', *, *, #1505, .T. ) ;
#10321 = CARTESIAN_POINT ( 'NONE',  ( -61.37466933804601865, -2.649564458509630072, 0.4839885628739446499 ) ) ;
#10322 = CARTESIAN_POINT ( 'NONE',  ( 33.05069135236684019, 8.148093138862860130, -1.550000000000114619 ) ) ;
#10323 = EDGE_CURVE ( 'NONE', #23389, #203, #25305, .T. ) ;
#10324 = EDGE_LOOP ( 'NONE', ( #21883, #12349, #26181, #26769 ) ) ;
#10325 = ORIENTED_EDGE ( 'NONE', *, *, #9400, .F. ) ;
#10326 = ORIENTED_EDGE ( 'NONE', *, *, #16317, .F. ) ;
#10327 = CARTESIAN_POINT ( 'NONE',  ( 15.61552784268241822, 5.277544294472392927, 1.204650266290664407 ) ) ;
#10328 = ORIENTED_EDGE ( 'NONE', *, *, #20916, .F. ) ;
#10329 = SHAPE_REPRESENTATION_RELATIONSHIP ( 'NONE' , 'NONE' ,  #3777, #1717 ) ;
#10330 = CARTESIAN_POINT ( 'NONE',  ( 31.84692766216867810, 7.617555580675888116, 1.949999999999889599 ) ) ;
#10331 = CARTESIAN_POINT ( 'NONE',  ( -60.00952994616204705, -4.643455692769866465E-15, 3.599999999999786038 ) ) ;
#10332 = VERTEX_POINT ( 'NONE', #10021 ) ;
#10333 = DIRECTION ( 'NONE',  ( 1.000000000000000000, 0.000000000000000000, 0.000000000000000000 ) ) ;
#10334 = AXIS2_PLACEMENT_3D ( 'NONE', #5521, #14558, #12033 ) ;
#10335 = DIRECTION ( 'NONE',  ( 1.000000000000000000, 3.125586771759065906E-16, 0.000000000000000000 ) ) ;
#10336 = CARTESIAN_POINT ( 'NONE',  ( 26.92903764427223123, 5.249711979587693200, 1.949999999999972422 ) ) ;
#10337 = ORIENTED_EDGE ( 'NONE', *, *, #22040, .T. ) ;
#10338 = EDGE_CURVE ( 'NONE', #17296, #17741, #6785, .T. ) ;
#10339 = CARTESIAN_POINT ( 'NONE',  ( 51.84831113588968066, 0.6920605891666815612, -1.653603923793075081 ) ) ;
#10340 = CARTESIAN_POINT ( 'NONE',  ( 52.02336772807328913, 3.827384603151627651, -2.050000000000181455 ) ) ;
#10341 = CARTESIAN_POINT ( 'NONE',  ( 58.45000000000001705, -0.8000000000000001554, -1.778341924377873973 ) ) ;
#10342 = DIRECTION ( 'NONE',  ( 0.000000000000000000, 0.000000000000000000, -1.000000000000000000 ) ) ;
#10343 = AXIS2_PLACEMENT_3D ( 'NONE', #16217, #23669, #8914 ) ;
#10344 = DIRECTION ( 'NONE',  ( -3.002035892788117952E-16, 0.9996898646859344595, 0.02490330187381124133 ) ) ;
#10346 = CARTESIAN_POINT ( 'NONE',  ( 58.65000000000002700, -1.022750809560422969, 1.571497941946552679 ) ) ;
#10345 = SURFACE_SIDE_STYLE ('',( #2922 ) ) ;
#10347 = EDGE_CURVE ( 'NONE', #5910, #30896, #22908, .T. ) ;
#10348 = CARTESIAN_POINT ( 'NONE',  ( 51.43900111557092458, 0.9711356030203728285, 1.449573366541679009 ) ) ;
#10349 = CARTESIAN_POINT ( 'NONE',  ( 50.35762544161296006, 8.151359338959888845, 1.549999999999824629 ) ) ;
#10350 = CARTESIAN_POINT ( 'NONE',  ( 58.75000000000000711, 1.457266603154988793, -1.320165430232766557 ) ) ;
#10351 = CARTESIAN_POINT ( 'NONE',  ( -56.72499999999997300, 3.116721586436802063E-15, -1.005743832985040150E-16 ) ) ;
#10352 = CIRCLE ( 'NONE', #750, 0.05000000000000015543 ) ;
#10353 = ORIENTED_EDGE ( 'NONE', *, *, #15824, .T. ) ;
#10354 = CARTESIAN_POINT ( 'NONE',  ( -54.49999477219272848, 1.549165129012789466, 3.331602747802265174 ) ) ;
#10355 = EDGE_LOOP ( 'NONE', ( #22574, #1955, #28445, #2216 ) ) ;
#10356 = EDGE_CURVE ( 'NONE', #17058, #26017, #5573, .T. ) ;
#10357 = ORIENTED_EDGE ( 'NONE', *, *, #2823, .F. ) ;
#10358 = EDGE_CURVE ( 'NONE', #5946, #10684, #3652, .T. ) ;
#10359 = CARTESIAN_POINT ( 'NONE',  ( -54.49999999999997868, 0.2900967345938421649, -3.387601494358211340 ) ) ;
#10360 = CARTESIAN_POINT ( 'NONE',  ( -57.73542740578360366, -3.725040285533365303, 1.239922660687675204 ) ) ;
#10361 = CARTESIAN_POINT ( 'NONE',  ( 15.97944027357900687, 4.944296796129566296, 2.193698057025775583 ) ) ;
#10362 = ADVANCED_FACE ( 'NONE', ( #25194 ), #12445, .F. ) ;
#10363 = ORIENTED_EDGE ( 'NONE', *, *, #18713, .T. ) ;
#10364 = ORIENTED_EDGE ( 'NONE', *, *, #23410, .T. ) ;
#10365 = VECTOR ( 'NONE', #20384, 1000.000000000000000 ) ;
#10366 = FACE_OUTER_BOUND ( 'NONE', #23638, .T. ) ;
#10367 = EDGE_LOOP ( 'NONE', ( #6244, #1929, #1520, #27753 ) ) ;
#10368 = CARTESIAN_POINT ( 'NONE',  ( 58.65000000000000568, 1.469015551797813179, -1.320082690053157037 ) ) ;
#10369 = ORIENTED_EDGE ( 'NONE', *, *, #20074, .T. ) ;
#10370 = CARTESIAN_POINT ( 'NONE',  ( 32.27289361194181083, 7.909974131749012649, -2.050000000000113509 ) ) ;
#10371 = CIRCLE ( 'NONE', #16430, 0.04999999999999989175 ) ;
#10372 = DIRECTION ( 'NONE',  ( 1.000000000000000000, -1.219044193948983948E-29, 3.491481338843133355E-15 ) ) ;
#10373 = FACE_OUTER_BOUND ( 'NONE', #6671, .T. ) ;
#10374 = EDGE_CURVE ( 'NONE', #6314, #8529, #11946, .T. ) ;
#10375 = CARTESIAN_POINT ( 'NONE',  ( 15.67083574136775681, -5.256402525809859227, -1.287848407636900117 ) ) ;
#10376 = CIRCLE ( 'NONE', #28067, 0.1500000000000002720 ) ;
#10377 = CARTESIAN_POINT ( 'NONE',  ( -60.33155989232410121, -1.962990915244706924, -3.400000000000220179 ) ) ;
#10378 = CARTESIAN_POINT ( 'NONE',  ( 53.87827693845231636, 5.944250707180074755, -2.050000000000187228 ) ) ;
#10379 = CARTESIAN_POINT ( 'NONE',  ( 47.10000000821191435, -3.608818513796487437, -1.949335135736566249 ) ) ;
#10380 = CARTESIAN_POINT ( 'NONE',  ( -59.19126343180466421, -2.406052454186071277, 1.245092465133171844 ) ) ;
#10381 = DIRECTION ( 'NONE',  ( 0.000000000000000000, 0.000000000000000000, 1.000000000000000000 ) ) ;
#10382 = CARTESIAN_POINT ( 'NONE',  ( 63.50000000000004263, -0.8382352941176473005, 2.222158093316616068 ) ) ;
#10383 = EDGE_CURVE ( 'NONE', #6063, #4965, #6377, .T. ) ;
#10384 = CIRCLE ( 'NONE', #8352, 159.6997717543496833 ) ;
#10385 = CARTESIAN_POINT ( 'NONE',  ( -59.09664939113120852, -2.332125100258536143, 1.258448456133006710 ) ) ;
#10386 = VECTOR ( 'NONE', #29327, 1000.000000000000000 ) ;
#10387 = DIRECTION ( 'NONE',  ( 0.000000000000000000, 1.000000000000000000, 0.000000000000000000 ) ) ;
#10388 = CARTESIAN_POINT ( 'NONE',  ( 51.55144386500332132, -1.037443573994098811, 1.251214392908860829 ) ) ;
#10389 = ORIENTED_EDGE ( 'NONE', *, *, #2095, .F. ) ;
#10390 = COLOUR_RGB ( '', 0.72549020, 0.75294118, 0.79215686) ;
#10391 = DIRECTION ( 'NONE',  ( 1.000000000000000000, 1.047444401652940007E-14, 0.000000000000000000 ) ) ;
#10392 = CARTESIAN_POINT ( 'NONE',  ( -36.48174642953001978, -3.496282614933922783, -4.130238739723587571 ) ) ;
#10393 = CARTESIAN_POINT ( 'NONE',  ( 54.40301486585899937, 5.980869397714326574, 0.9749999999998116840 ) ) ;
#10394 = AXIS2_PLACEMENT_3D ( 'NONE', #13359, #15763, #13068 ) ;
#10395 = EDGE_LOOP ( 'NONE', ( #19168, #11816, #24769, #4683 ) ) ;
#10396 = ADVANCED_FACE ( 'NONE', ( #8100 ), #23592, .T. ) ;
#10397 = CARTESIAN_POINT ( 'NONE',  ( -59.69142724121850563, -2.412383461849193278, -1.233589124872107146 ) ) ;
#10398 = ORIENTED_EDGE ( 'NONE', *, *, #3009, .T. ) ;
#10399 = AXIS2_PLACEMENT_3D ( 'NONE', #6971, #21862, #24970 ) ;
#10400 = EDGE_CURVE ( 'NONE', #10954, #4977, #27554, .T. ) ;
#10401 = CARTESIAN_POINT ( 'NONE',  ( 51.75922852344036329, 4.143493964997498225, 1.955480185863871956 ) ) ;
#10402 = CARTESIAN_POINT ( 'NONE',  ( -55.15835481156724285, -3.238593381231841928, -2.874284765127022911 ) ) ;
#10404 = CARTESIAN_POINT ( 'NONE',  ( 51.67105141853712524, -3.772456960769059453, -1.610749547355440292 ) ) ;
#10403 = CARTESIAN_POINT ( 'NONE',  ( 58.50000000000001421, 0.000000000000000000, 0.000000000000000000 ) ) ;
#10405 = EDGE_CURVE ( 'NONE', #4841, #5779, #27127, .T. ) ;
#10406 = ORIENTED_EDGE ( 'NONE', *, *, #3039, .F. ) ;
#10407 = DIRECTION ( 'NONE',  ( -1.000000000000000000, 1.219044193948983948E-29, -3.491481338843133355E-15 ) ) ;
#10408 = CARTESIAN_POINT ( 'NONE',  ( 57.00965563974653350, -0.7295352771400042124, -1.796193723857490321 ) ) ;
#10409 = ORIENTED_EDGE ( 'NONE', *, *, #25059, .T. ) ;
#10411 = CARTESIAN_POINT ( 'NONE',  ( -54.46895629856896903, -1.503487923075246480, -4.032311158269683560 ) ) ;
#10410 = CARTESIAN_POINT ( 'NONE',  ( 58.65000000000003411, -1.469015551795667784, 1.320082690054176666 ) ) ;
#10412 = DIRECTION ( 'NONE',  ( -1.000000000000000000, -0.000000000000000000, -0.000000000000000000 ) ) ;
#10413 = VERTEX_POINT ( 'NONE', #30396 ) ;
#10414 = CARTESIAN_POINT ( 'NONE',  ( -59.12499999999997158, 2.489203624310590612, -2.804704140674917134 ) ) ;
#10415 = CARTESIAN_POINT ( 'NONE',  ( -56.06249999999995737, -1.962990915244703816, -3.400000000000207745 ) ) ;
#10416 = AXIS2_PLACEMENT_3D ( 'NONE', #14855, #17399, #19791 ) ;
#10417 = CARTESIAN_POINT ( 'NONE',  ( 58.72204580543390762, 1.612507782426283898, -0.9570475208907850417 ) ) ;
#10418 = AXIS2_PLACEMENT_3D ( 'NONE', #23605, #1724, #2057 ) ;
#10419 = CARTESIAN_POINT ( 'NONE',  ( -54.49999999999995737, -2.900697337314245505, -2.163606381124719924 ) ) ;
#10420 = CARTESIAN_POINT ( 'NONE',  ( 51.90000000000001279, 1.734723475976807094E-15, 0.000000000000000000 ) ) ;
#10421 = CARTESIAN_POINT ( 'NONE',  ( -55.25952994616203995, -3.117691453623963938, -1.800000000000207434 ) ) ;
#10422 = CARTESIAN_POINT ( 'NONE',  ( 16.00221665700883378, 0.5763363385013873241, 5.380853831843024793 ) ) ;
#10423 = AXIS2_PLACEMENT_3D ( 'NONE', #28930, #7700, #7241 ) ;
#10424 = VERTEX_POINT ( 'NONE', #25346 ) ;
#10425 = AXIS2_PLACEMENT_3D ( 'NONE', #29354, #2918, #12115 ) ;
#10426 = AXIS2_PLACEMENT_3D ( 'NONE', #30252, #10776, #29939 ) ;
#10427 = CARTESIAN_POINT ( 'NONE',  ( -61.82620411128902305, -2.492743192708819944, -0.4118588219422569252 ) ) ;
#10428 = ADVANCED_BREP_SHAPE_REPRESENTATION ( '', ( #26054, #9018 ), #15625 ) ;
#10429 = EDGE_CURVE ( 'NONE', #9996, #15276, #10932, .T. ) ;
#10430 = EDGE_CURVE ( 'NONE', #3555, #12911, #22578, .T. ) ;
#10431 = CARTESIAN_POINT ( 'NONE',  ( -54.98542740578361077, 2.936324665650207333, 2.606018187048498191 ) ) ;
#10433 = EDGE_CURVE ( 'NONE', #27144, #9993, #23297, .T. ) ;
#10432 = DIRECTION ( 'NONE',  ( 0.000000000000000000, 0.000000000000000000, -1.000000000000000000 ) ) ;
#10434 = VECTOR ( 'NONE', #18471, 1000.000000000000000 ) ;
#10435 = CARTESIAN_POINT ( 'NONE',  ( -36.04518387042480043, 4.861582133260092142, -2.394243994563964417 ) ) ;
#10436 = DIRECTION ( 'NONE',  ( -0.3180732113053867383, -0.9480661539417379879, -0.000000000000000000 ) ) ;
#10437 = CARTESIAN_POINT ( 'NONE',  ( 32.52839478919696603, 7.997762531131884955, 2.049999999999888800 ) ) ;
#10438 = ORIENTED_EDGE ( 'NONE', *, *, #23484, .F. ) ;
#10439 = CYLINDRICAL_SURFACE ( 'NONE', #24940, 0.1000000000000000472 ) ;
#10440 = CONICAL_SURFACE ( 'NONE', #13947, 2.099999999999999645, 0.7853981633974396193 ) ;
#10441 = ORIENTED_EDGE ( 'NONE', *, *, #28770, .T. ) ;
#10442 = PRODUCT_DEFINITION_CONTEXT ( 'detailed design', #17699, 'design' ) ;
#10443 = CARTESIAN_POINT ( 'NONE',  ( -59.16035890245980511, 2.496590366952375017, -0.9473018300160132021 ) ) ;
#10445 = CARTESIAN_POINT ( 'NONE',  ( 58.70362814788261119, -0.4999999999993853805, -1.816403611747765767 ) ) ;
#10444 = CARTESIAN_POINT ( 'NONE',  ( -54.48133250964848884, -2.367385699161606016, -2.689772239255368902 ) ) ;
#10446 = AXIS2_PLACEMENT_3D ( 'NONE', #3549, #8286, #1017 ) ;
#10447 = EDGE_LOOP ( 'NONE', ( #16398, #4021, #10661, #21143 ) ) ;
#10448 = EDGE_LOOP ( 'NONE', ( #21627, #10502, #14369, #12830 ) ) ;
#10449 = LINE ( 'NONE', #20131, #13831 ) ;
#10450 = CIRCLE ( 'NONE', #3868, 0.09999999999999986677 ) ;
#10451 = CARTESIAN_POINT ( 'NONE',  ( -73.89999999999997726, -2.435524336289708093E-15, 4.607889071584891164E-15 ) ) ;
#10452 =( BOUNDED_CURVE ( )  B_SPLINE_CURVE ( 3, ( #8397, #18083, #29614, #7942 ),
 .UNSPECIFIED., .F., .T. ) 
 B_SPLINE_CURVE_WITH_KNOTS ( ( 4, 4 ),
 ( 1.033802687944701759, 1.276740478505648202 ),
 .UNSPECIFIED. ) 
 CURVE ( )  GEOMETRIC_REPRESENTATION_ITEM ( )  RATIONAL_B_SPLINE_CURVE ( ( 1.000000000000000000, 0.9950878134350369386, 0.9950878134350369386, 1.000000000000000000 ) ) 
 REPRESENTATION_ITEM ( '' )  );
#10453 = VERTEX_POINT ( 'NONE', #20310 ) ;
#10454 = AXIS2_PLACEMENT_3D ( 'NONE', #2461, #229, #19866 ) ;
#10456 = CARTESIAN_POINT ( 'NONE',  ( 51.79412664516154763, -4.148449925053760090, 1.066233527417929539 ) ) ;
#10455 = CARTESIAN_POINT ( 'NONE',  ( -56.00952994616203995, -3.117691453623963938, -1.800000000000210099 ) ) ;
#10457 = CARTESIAN_POINT ( 'NONE',  ( 50.31565037626138803, 1.386108502191577108, 3.851082811767820413 ) ) ;
#10458 = CARTESIAN_POINT ( 'NONE',  ( -35.85663232820584057, -4.804073783693461941, 2.042134687550347216 ) ) ;
#10459 = DIRECTION ( 'NONE',  ( 1.000000000000000000, 0.000000000000000000, 0.000000000000000000 ) ) ;
#10460 = CARTESIAN_POINT ( 'NONE',  ( 58.65844932252340982, -1.302247349114548980, -1.349094575298717347 ) ) ;
#10461 = TOROIDAL_SURFACE ( 'NONE', #28146, 2.649999999999999911, 0.05000000000000000278 ) ;
#10462 = EDGE_LOOP ( 'NONE', ( #24456, #9554, #3917 ) ) ;
#10463 = VECTOR ( 'NONE', #14182, 1000.000000000000000 ) ;
#10464 = CARTESIAN_POINT ( 'NONE',  ( -60.44702994616202574, -2.078460969082631227, -3.600000000000220801 ) ) ;
#10465 = VECTOR ( 'NONE', #28353, 1000.000000000000000 ) ;
#10466 = FACE_OUTER_BOUND ( 'NONE', #28280, .T. ) ;
#10467 = LINE ( 'NONE', #27081, #27804 ) ;
#10468 = DIRECTION ( 'NONE',  ( 0.000000000000000000, 1.000000000000000000, 0.000000000000000000 ) ) ;
#10469 = EDGE_CURVE ( 'NONE', #6234, #6022, #13426, .T. ) ;
#10470 = CLOSED_SHELL ( 'NONE', ( #16351, #13427, #17251, #2847 ) ) ;
#10471 = AXIS2_PLACEMENT_3D ( 'NONE', #9434, #1987, #22050 ) ;
#10472 = EDGE_CURVE ( 'NONE', #26143, #13128, #16213, .T. ) ;
#10473 = DIRECTION ( 'NONE',  ( 1.000000000000000000, 3.054025858079668409E-16, -2.042474015755241579E-16 ) ) ;
#10474 = CIRCLE ( 'NONE', #14522, 0.04999999999999969746 ) ;
#10477 = EDGE_CURVE ( 'NONE', #26805, #4199, #19018, .T. ) ;
#10476 = DIRECTION ( 'NONE',  ( -1.000000000000000000, -0.000000000000000000, -0.000000000000000000 ) ) ;
#10475 = CARTESIAN_POINT ( 'NONE',  ( 24.57460841532290630, 5.893272594507614315, -1.425000000000085754 ) ) ;
#10478 = CONICAL_SURFACE ( 'NONE', #28167, 1.350000000000000089, 0.04164257909858841422 ) ;
#10479 = CARTESIAN_POINT ( 'NONE',  ( 51.90000000000001990, -4.131056160354152240, -1.100000000000000089 ) ) ;
#10480 = CARTESIAN_POINT ( 'NONE',  ( 50.25000000000000000, 1.791164585743128423, -0.8897917884432153812 ) ) ;
#10482 = CARTESIAN_POINT ( 'NONE',  ( -54.49999999999999289, 1.970152530825497017, -2.913597794826568332 ) ) ;
#10481 = DIRECTION ( 'NONE',  ( 1.000000000000000000, 8.626663965456221796E-17, 1.494526870159859873E-16 ) ) ;
#10483 = ORIENTED_EDGE ( 'NONE', *, *, #20072, .F. ) ;
#10484 = DIRECTION ( 'NONE',  ( 1.000000000000000000, 1.047444401652940007E-14, 0.000000000000000000 ) ) ;
#10485 = DIRECTION ( 'NONE',  ( 1.000000000000000000, -0.000000000000000000, -0.000000000000000000 ) ) ;
#10486 = AXIS2_PLACEMENT_3D ( 'NONE', #24669, #2811, #2982 ) ;
#10488 = FACE_OUTER_BOUND ( 'NONE', #15748, .T. ) ;
#10487 = CARTESIAN_POINT ( 'NONE',  ( 15.29954477411490465, 4.018128194441618284, -3.618665885216152400 ) ) ;
#10489 = CARTESIAN_POINT ( 'NONE',  ( -54.39999999999999147, 1.499999999999996003, 3.959797974644419849 ) ) ;
#10490 = EDGE_LOOP ( 'NONE', ( #22386, #7243, #12744, #27156 ) ) ;
#10491 = CARTESIAN_POINT ( 'NONE',  ( 61.20026580823483187, -0.7453886133000856562, 1.660366360129213348 ) ) ;
#10492 = CARTESIAN_POINT ( 'NONE',  ( 51.80000000000001847, 1.521694824349982378, -3.995005614707754393 ) ) ;
#10493 = AXIS2_PLACEMENT_3D ( 'NONE', #24619, #7680, #7372 ) ;
#10494 = EDGE_CURVE ( 'NONE', #16074, #26012, #15492, .T. ) ;
#10495 = CIRCLE ( 'NONE', #13499, 1.625000000000000222 ) ;
#10496 = ORIENTED_EDGE ( 'NONE', *, *, #28790, .F. ) ;
#10497 = CARTESIAN_POINT ( 'NONE',  ( -45.15971931043468146, 0.000000000000000000, 0.000000000000000000 ) ) ;
#10498 = ORIENTED_EDGE ( 'NONE', *, *, #9263, .F. ) ;
#10499 = EDGE_LOOP ( 'NONE', ( #6520, #7215 ) ) ;
#10500 = CARTESIAN_POINT ( 'NONE',  ( 51.70000000000001705, -4.179189514726507682, 0.8999999999999998002 ) ) ;
#10501 = CARTESIAN_POINT ( 'NONE',  ( 49.00000000000000000, 0.5000000000000000000, -1.988246715073869408 ) ) ;
#10502 = ORIENTED_EDGE ( 'NONE', *, *, #6579, .F. ) ;
#10503 = CARTESIAN_POINT ( 'NONE',  ( 34.49381514799785009, 8.210676854548648151, 1.949999999999878719 ) ) ;
#10504 = VECTOR ( 'NONE', #13853, 1000.000000000000000 ) ;
#10505 = CARTESIAN_POINT ( 'NONE',  ( -60.44702994616202574, -2.078460969082631227, -3.600000000000220801 ) ) ;
#10506 = ORIENTED_EDGE ( 'NONE', *, *, #30536, .F. ) ;
#10507 = DIRECTION ( 'NONE',  ( 0.000000000000000000, -6.217248937900896348E-15, 1.000000000000000000 ) ) ;
#10508 = AXIS2_PLACEMENT_3D ( 'NONE', #2140, #11962, #1990 ) ;
#10509 = AXIS2_PLACEMENT_3D ( 'NONE', #26750, #4721, #16630 ) ;
#10510 = CARTESIAN_POINT ( 'NONE',  ( -54.49999999999996447, 1.600000000000021627, -3.363870538531680054 ) ) ;
#10511 = CARTESIAN_POINT ( 'NONE',  ( 26.61241883252574070, 5.319505464261285788, 2.049999999999907008 ) ) ;
#10512 = VERTEX_POINT ( 'NONE', #11574 ) ;
#10513 = FACE_OUTER_BOUND ( 'NONE', #928, .T. ) ;
#10514 = CARTESIAN_POINT ( 'NONE',  ( 58.65000000000001279, 0.5811678240991622335, -1.782657835994492679 ) ) ;
#10515 = CARTESIAN_POINT ( 'NONE',  ( 17.21035195517769267, 5.407411300779131125, 0.000000000000000000 ) ) ;
#10516 = AXIS2_PLACEMENT_3D ( 'NONE', #17252, #12480, #10122 ) ;
#10517 = CARTESIAN_POINT ( 'NONE',  ( -35.85663232820584057, 0.9159215771353744762, 4.311190327365977737 ) ) ;
#10518 = DIRECTION ( 'NONE',  ( 1.000000000000000000, 3.054025858079668409E-16, -2.042474015755241579E-16 ) ) ;
#10519 = VECTOR ( 'NONE', #4067, 1000.000000000000000 ) ;
#10520 = EDGE_CURVE ( 'NONE', #26980, #5427, #26443, .T. ) ;
#10521 = TOROIDAL_SURFACE ( 'NONE', #28212, 2.973495046502706796, 1.679509022399086948 ) ;
#10523 = CARTESIAN_POINT ( 'NONE',  ( -64.32138495697122949, -2.298612619042724958, -0.05726080253994958458 ) ) ;
#10522 = CARTESIAN_POINT ( 'NONE',  ( 50.87477060347630697, 8.633605004120575188, 1.549999999999822631 ) ) ;
#10524 = CARTESIAN_POINT ( 'NONE',  ( 51.37191502447495139, 0.9974949139205757653, 1.404479416154130522 ) ) ;
#10525 = DIRECTION ( 'NONE',  ( 0.000000000000000000, 0.9996898646859343485, 0.02490330187381116153 ) ) ;
#10526 = CARTESIAN_POINT ( 'NONE',  ( 58.64999999999999858, 1.253243060178337087, -1.394635017528379484 ) ) ;
#10527 = DIRECTION ( 'NONE',  ( -2.614375865348240525E-16, 0.2008964009354147484, -0.9796124928211139560 ) ) ;
#10528 = EDGE_LOOP ( 'NONE', ( #25758, #164, #28817, #24398 ) ) ;
#10529 = CARTESIAN_POINT ( 'NONE',  ( -54.48531357662248809, 1.514292094527452504, 3.309285685900293927 ) ) ;
#10530 = ORIENTED_EDGE ( 'NONE', *, *, #30919, .F. ) ;
#10531 = ADVANCED_FACE ( 'NONE', ( #28506 ), #23924, .T. ) ;
#10532 = VERTEX_POINT ( 'NONE', #25813 ) ;
#10533 = CARTESIAN_POINT ( 'NONE',  ( -59.10142724674265935, 2.309330906357313307, 1.299824891736185206 ) ) ;
#10534 = CARTESIAN_POINT ( 'NONE',  ( -57.11042740578361077, -0.7887156198831601905, 3.845940847736173840 ) ) ;
#10536 = CARTESIAN_POINT ( 'NONE',  ( -61.35320637528415944, -2.582160856334464683, 0.6721421056772638458 ) ) ;
#10535 = CARTESIAN_POINT ( 'NONE',  ( -58.18749999999995737, 1.962990915244749557, -3.400000000000197531 ) ) ;
#10537 = ORIENTED_EDGE ( 'NONE', *, *, #28162, .F. ) ;
#10538 = ORIENTED_EDGE ( 'NONE', *, *, #25940, .F. ) ;
#10539 = CARTESIAN_POINT ( 'NONE',  ( -55.78335481156724285, 0.7533615035078067290, -3.673546848079180194 ) ) ;
#10540 = AXIS2_PLACEMENT_3D ( 'NONE', #8430, #27434, #27751 ) ;
#10541 = ORIENTED_EDGE ( 'NONE', *, *, #10815, .F. ) ;
#10542 = CARTESIAN_POINT ( 'NONE',  ( 51.71302666497697942, 3.851408839085467495, -1.405934584416819400 ) ) ;
#10543 = EDGE_LOOP ( 'NONE', ( #2346, #15145, #16290, #11763 ) ) ;
#10544 = CARTESIAN_POINT ( 'NONE',  ( 30.17828911090724375, 6.795520168003006845, -2.050000000000104627 ) ) ;
#10545 = CARTESIAN_POINT ( 'NONE',  ( -67.99999999999995737, 0.6629581230868679675, -3.232721226309673845 ) ) ;
#10546 = CARTESIAN_POINT ( 'NONE',  ( 54.40293493925265267, 6.717672571224089673, 2.002198665876135930 ) ) ;
#10547 = ORIENTED_EDGE ( 'NONE', *, *, #3219, .T. ) ;
#10548 = CARTESIAN_POINT ( 'NONE',  ( -59.83155989232413674, -1.962990915244731571, 3.399999999999779199 ) ) ;
#10549 = CARTESIAN_POINT ( 'NONE',  ( 47.12240576366414757, -3.662050566052967415, 1.846868639358291819 ) ) ;
#10550 = CARTESIAN_POINT ( 'NONE',  ( 47.86840742095310475, -4.031600731367475099, -1.173113608354439563 ) ) ;
#10551 = EDGE_CURVE ( 'NONE', #18572, #2009, #4442, .T. ) ;
#10552 = CARTESIAN_POINT ( 'NONE',  ( 48.43975240335598897, 1.282505688586122572, 3.869483523004607406 ) ) ;
#10553 = CARTESIAN_POINT ( 'NONE',  ( -35.85663232820584057, -0.9159215771349861202, -4.311190327366008823 ) ) ;
#10556 = ADVANCED_FACE ( 'NONE', ( #4737 ), #21909, .F. ) ;
#10555 = CYLINDRICAL_SURFACE ( 'NONE', #12940, 0.09999999999999972800 ) ;
#10554 = LINE ( 'NONE', #22903, #15493 ) ;
#10557 = EDGE_CURVE ( 'NONE', #27460, #24533, #9446, .T. ) ;
#10558 = CIRCLE ( 'NONE', #30251, 4.299999999999998046 ) ;
#10559 = FACE_OUTER_BOUND ( 'NONE', #1278, .T. ) ;
#10560 = AXIS2_PLACEMENT_3D ( 'NONE', #2834, #306, #12488 ) ;
#10561 = DIRECTION ( 'NONE',  ( -0.6819983600625022513, 0.7313537016191670181, 2.468850131082277965E-15 ) ) ;
#10562 = ORIENTED_EDGE ( 'NONE', *, *, #29291, .T. ) ;
#10563 = DIRECTION ( 'NONE',  ( 1.000000000000000000, -1.219044193948983948E-29, 3.491481338843133355E-15 ) ) ;
#10564 = CARTESIAN_POINT ( 'NONE',  ( 54.32946475390676966, 6.710822919118950125, 2.049999999999810196 ) ) ;
#10565 = ORIENTED_EDGE ( 'NONE', *, *, #24895, .T. ) ;
#10566 = EDGE_CURVE ( 'NONE', #12762, #11632, #22015, .T. ) ;
#10567 = DIRECTION ( 'NONE',  ( -1.000000000000000000, 0.000000000000000000, 0.000000000000000000 ) ) ;
#10568 = ORIENTED_EDGE ( 'NONE', *, *, #26030, .F. ) ;
#10569 = FACE_OUTER_BOUND ( 'NONE', #30682, .T. ) ;
#10570 = DIRECTION ( 'NONE',  ( 1.000000000000000000, 1.047444401652940007E-14, 0.000000000000000000 ) ) ;
#10572 = DIRECTION ( 'NONE',  ( 1.000000000000000000, 4.939082069373669245E-17, -1.520093157366878429E-16 ) ) ;
#10571 = DIRECTION ( 'NONE',  ( 0.03489949670185131525, 0.9993908270191184107, 0.000000000000000000 ) ) ;
#10573 = VERTEX_POINT ( 'NONE', #9814 ) ;
#10574 = CARTESIAN_POINT ( 'NONE',  ( 51.80000000000002558, 4.175664755576631748, 1.929721184273780255 ) ) ;
#10575 = PLANE ( 'NONE',  #20617 ) ;
#10576 = ORIENTED_EDGE ( 'NONE', *, *, #28431, .F. ) ;
#10578 = CYLINDRICAL_SURFACE ( 'NONE', #6974, 1.000000000000000000 ) ;
#10577 = DIRECTION ( 'NONE',  ( 0.000000000000000000, 0.000000000000000000, 1.000000000000000000 ) ) ;
#10579 = ORIENTED_EDGE ( 'NONE', *, *, #13276, .F. ) ;
#10580 = VERTEX_POINT ( 'NONE', #26763 ) ;
#10581 = CARTESIAN_POINT ( 'NONE',  ( 53.91566439300392943, 6.672259399342834740, -1.839335743490527530 ) ) ;
#10582 = CARTESIAN_POINT ( 'NONE',  ( 56.95641943120798345, -0.7163990203283279179, 1.759764883066090801 ) ) ;
#10583 = EDGE_CURVE ( 'NONE', #27339, #4409, #815, .T. ) ;
#10584 = AXIS2_PLACEMENT_3D ( 'NONE', #19953, #17583, #27227 ) ;
#10585 = CARTESIAN_POINT ( 'NONE',  ( 58.75000000000002132, -0.5380862305903428844, -2.008165151418244143 ) ) ;
#10586 = CARTESIAN_POINT ( 'NONE',  ( 51.45655683570191741, -0.9591657938390818483, 1.468576096419532906 ) ) ;
#10587 = ORIENTED_EDGE ( 'NONE', *, *, #2806, .F. ) ;
#10588 = EDGE_CURVE ( 'NONE', #19797, #7506, #8896, .T. ) ;
#10589 = CARTESIAN_POINT ( 'NONE',  ( 15.56401610563845672, -2.291889356119292120, 4.901871067649883784 ) ) ;
#10590 = ADVANCED_FACE ( 'NONE', ( #17402 ), #5517, .T. ) ;
#10591 = TOROIDAL_SURFACE ( 'NONE', #10076, 3.020710678118645909, 0.05000000000000000278 ) ;
#10592 = EDGE_CURVE ( 'NONE', #28731, #4847, #19648, .T. ) ;
#10593 = CARTESIAN_POINT ( 'NONE',  ( -60.60075002049966031, -2.485844148457513114, 0.9463202019723547798 ) ) ;
#10594 = DIRECTION ( 'NONE',  ( -1.000000000000000000, 0.000000000000000000, 1.047444401652940007E-14 ) ) ;
#10595 = CARTESIAN_POINT ( 'NONE',  ( -59.19702994616205416, -2.078460969082660537, 3.599999999999779821 ) ) ;
#10596 = PRESENTATION_LAYER_ASSIGNMENT (  '', '', ( #27754 ) ) ;
#10597 = DIRECTION ( 'NONE',  ( 0.000000000000000000, -1.224646799147353947E-16, 1.000000000000000000 ) ) ;
#10598 = CARTESIAN_POINT ( 'NONE',  ( 22.68377116885792333, 6.706477478074083010, 2.049999999999920774 ) ) ;
#10599 = VERTEX_POINT ( 'NONE', #463 ) ;
#10600 = TOROIDAL_SURFACE ( 'NONE', #14647, 2.150000000000000355, 0.05000000000000000278 ) ;
#10601 = FACE_OUTER_BOUND ( 'NONE', #26352, .T. ) ;
#10602 = ORIENTED_EDGE ( 'NONE', *, *, #17564, .F. ) ;
#10603 = DIRECTION ( 'NONE',  ( -1.110223024625157329E-14, 0.000000000000000000, -1.000000000000000000 ) ) ;
#10605 = CARTESIAN_POINT ( 'NONE',  ( 58.74999981404334903, -1.321446761053663099, 1.441842230225543808 ) ) ;
#10604 = CARTESIAN_POINT ( 'NONE',  ( -54.48513940398811428, -2.374617027978079609, -2.675739047658152625 ) ) ;
#10606 = ORIENTED_EDGE ( 'NONE', *, *, #29178, .F. ) ;
#10607 = ORIENTED_EDGE ( 'NONE', *, *, #10229, .T. ) ;
#10608 = CARTESIAN_POINT ( 'NONE',  ( -59.69999999999997442, 3.400000000000007905, -2.001823990013003858E-13 ) ) ;
#10609 = CARTESIAN_POINT ( 'NONE',  ( -57.31249999999996447, -0.7533615035078060629, 3.673546848079176641 ) ) ;
#10610 = ORIENTED_EDGE ( 'NONE', *, *, #24907, .F. ) ;
#10612 = FACE_OUTER_BOUND ( 'NONE', #10448, .T. ) ;
#10611 = CARTESIAN_POINT ( 'NONE',  ( -57.00952994616205416, -4.643455692769903542E-15, 3.599999999999796696 ) ) ;
#10613 = CARTESIAN_POINT ( 'NONE',  ( -57.11042740578361077, -0.7887156198831601905, 3.845940847736173840 ) ) ;
#10614 = EDGE_CURVE ( 'NONE', #5591, #13554, #22714, .T. ) ;
#10615 = DIRECTION ( 'NONE',  ( 1.000000000000000000, -1.219044193948983948E-29, 3.491481338843133355E-15 ) ) ;
#10616 = CARTESIAN_POINT ( 'NONE',  ( 0.000000000000000000, 0.000000000000000000, 0.000000000000000000 ) ) ;
#10617 = CARTESIAN_POINT ( 'NONE',  ( -59.30000000000000426, -3.594491936234972318, -0.2567477776118052835 ) ) ;
#10618 = SURFACE_STYLE_FILL_AREA ( #13135 ) ;
#10619 = EDGE_CURVE ( 'NONE', #5779, #8227, #23726, .T. ) ;
#10620 = ORIENTED_EDGE ( 'NONE', *, *, #26060, .T. ) ;
#10621 = AXIS2_PLACEMENT_3D ( 'NONE', #2479, #29510, #14657 ) ;
#10622 = CYLINDRICAL_SURFACE ( 'NONE', #25605, 0.1000000000000001721 ) ;
#10623 = CARTESIAN_POINT ( 'NONE',  ( 52.09213388422764979, 8.600000000000108002, -1.949999998429221337 ) ) ;
#10624 = CARTESIAN_POINT ( 'NONE',  ( -73.89999999999996305, -1.301636140808608788, -0.03242509391109851813 ) ) ;
#10625 = CARTESIAN_POINT ( 'NONE',  ( 15.61552784268242000, 0.4851603899461020553, 5.391500295856302749 ) ) ;
#10626 = EDGE_CURVE ( 'NONE', #19375, #23193, #719, .T. ) ;
#10627 = VECTOR ( 'NONE', #7692, 1000.000000000000000 ) ;
#10628 = CARTESIAN_POINT ( 'NONE',  ( -59.69873842481536030, -2.257036478699359972, 1.538083288954898542 ) ) ;
#10630 = CARTESIAN_POINT ( 'NONE',  ( 58.72200624034177707, -1.805437858155882758, -0.5064713447804831681 ) ) ;
#10629 = CARTESIAN_POINT ( 'NONE',  ( -56.87499999999996447, -2.944486372867073598, -1.700000000000217781 ) ) ;
#10631 = DIRECTION ( 'NONE',  ( 1.000000000000000000, 1.047444401652940007E-14, 0.000000000000000000 ) ) ;
#10632 = CARTESIAN_POINT ( 'NONE',  ( 51.80000000000001847, 2.428612866367529932E-14, 0.000000000000000000 ) ) ;
#10634 = CARTESIAN_POINT ( 'NONE',  ( -54.49999999999997158, 0.5440517917263103520, -3.381945888744238626 ) ) ;
#10633 = DIRECTION ( 'NONE',  ( 1.000000000000000000, 0.000000000000000000, -1.047444401652940007E-14 ) ) ;
#10635 = ORIENTED_EDGE ( 'NONE', *, *, #29326, .T. ) ;
#10636 =( BOUNDED_CURVE ( )  B_SPLINE_CURVE ( 3, ( #17290, #15063, #26474, #19520 ),
 .UNSPECIFIED., .F., .T. ) 
 B_SPLINE_CURVE_WITH_KNOTS ( ( 4, 4 ),
 ( 4.242719404917985493, 4.329617956773491372 ),
 .UNSPECIFIED. ) 
 CURVE ( )  GEOMETRIC_REPRESENTATION_ITEM ( )  RATIONAL_B_SPLINE_CURVE ( ( 1.000000000000000000, 0.9993708191325071377, 0.9993708191325071377, 1.000000000000000000 ) ) 
 REPRESENTATION_ITEM ( '' )  );
#10637 = CARTESIAN_POINT ( 'NONE',  ( 49.00000000000002132, 1.401298464324817071E-42, -5.132477568099407673E-13 ) ) ;
#10638 = CYLINDRICAL_SURFACE ( 'NONE', #8753, 0.1000000000000000472 ) ;
#10640 = CARTESIAN_POINT ( 'NONE',  ( -59.61160122551025609, -2.340542558125645822, -1.243912201914837423 ) ) ;
#10639 = CARTESIAN_POINT ( 'NONE',  ( 63.50000000000000000, 0.7500000000000000000, -1.988246715074021731 ) ) ;
#10641 = CARTESIAN_POINT ( 'NONE',  ( -60.49999999999995737, -0.8638545240222812449, 4.212333719130789689 ) ) ;
#10642 = ORIENTED_EDGE ( 'NONE', *, *, #21675, .F. ) ;
#10643 = CARTESIAN_POINT ( 'NONE',  ( 53.93929004300593277, 7.474130129650687238, 2.049999999999811084 ) ) ;
#10644 = CARTESIAN_POINT ( 'NONE',  ( 63.50000000000002842, 1.401298464324817071E-42, -6.651271950496169736E-13 ) ) ;
#10645 = ORIENTED_EDGE ( 'NONE', *, *, #4981, .T. ) ;
#10646 = FACE_OUTER_BOUND ( 'NONE', #16336, .T. ) ;
#10647 = VERTEX_POINT ( 'NONE', #5065 ) ;
#10648 = EDGE_CURVE ( 'NONE', #5085, #20372, #8537, .T. ) ;
#10649 = LINE ( 'NONE', #27896, #8708 ) ;
#10650 = DIRECTION ( 'NONE',  ( 1.000000000000000000, -1.219044193948983948E-29, 3.491481338843133355E-15 ) ) ;
#10651 = EDGE_LOOP ( 'NONE', ( #17346, #19544, #26356, #16591, #18801, #2311 ) ) ;
#10652 = VECTOR ( 'NONE', #11713, 1000.000000000000000 ) ;
#10653 = EDGE_CURVE ( 'NONE', #14688, #25687, #10144, .T. ) ;
#10654 = CARTESIAN_POINT ( 'NONE',  ( 58.45000000000001705, 0.8000000000000002665, -2.421260002560650104 ) ) ;
#10655 = CARTESIAN_POINT ( 'NONE',  ( -54.64405989232413674, -3.920666489018357767E-15, 3.399999999999804512 ) ) ;
#10656 = ORIENTED_EDGE ( 'NONE', *, *, #26854, .F. ) ;
#10657 = CARTESIAN_POINT ( 'NONE',  ( 58.65000000000004121, -1.782657835994308604, 0.5811678240972268927 ) ) ;
#10658 = EDGE_CURVE ( 'NONE', #2983, #29380, #18170, .T. ) ;
#10659 = PLANE ( 'NONE',  #14196 ) ;
#10660 = CARTESIAN_POINT ( 'NONE',  ( 22.32354329421583472, 7.018810582754515970, 2.049999999999858158 ) ) ;
#10661 = ORIENTED_EDGE ( 'NONE', *, *, #3847, .T. ) ;
#10662 = CARTESIAN_POINT ( 'NONE',  ( -56.93749999999997158, -3.925981830489445379, -2.163561077067149631E-13 ) ) ;
#10663 = DIRECTION ( 'NONE',  ( 0.000000000000000000, 0.000000000000000000, 1.000000000000000000 ) ) ;
#10664 = CARTESIAN_POINT ( 'NONE',  ( 58.45000000000001705, 0.8000000000000000444, -2.421260002560649660 ) ) ;
#10665 = CARTESIAN_POINT ( 'NONE',  ( 34.50000000000001421, 0.000000000000000000, 0.000000000000000000 ) ) ;
#10666 = FACE_OUTER_BOUND ( 'NONE', #17919, .T. ) ;
#10667 = EDGE_CURVE ( 'NONE', #29070, #2569, #27755, .T. ) ;
#10668 = FACE_OUTER_BOUND ( 'NONE', #184, .T. ) ;
#10669 = CIRCLE ( 'NONE', #25828, 4.375000000000000000 ) ;
#10670 = DIRECTION ( 'NONE',  ( 1.000000000000000000, 0.000000000000000000, 0.000000000000000000 ) ) ;
#10671 = CARTESIAN_POINT ( 'NONE',  ( 50.59602332238209499, 0.1408342061609078322, 1.212874140286674063 ) ) ;
#10672 = DIRECTION ( 'NONE',  ( 1.000000000000000000, 0.000000000000000000, -3.491481338843133355E-15 ) ) ;
#10673 = CARTESIAN_POINT ( 'NONE',  ( -54.47754877553799702, 1.508273929415538062, -3.305418158118663907 ) ) ;
#10674 = DIRECTION ( 'NONE',  ( 1.000000000000000000, 0.000000000000000000, -1.047444401652940007E-14 ) ) ;
#10675 = VERTEX_POINT ( 'NONE', #21874 ) ;
#10676 = CARTESIAN_POINT ( 'NONE',  ( -59.69142724121850563, -2.412383461849193278, -1.233589124872107146 ) ) ;
#10677 = ORIENTED_EDGE ( 'NONE', *, *, #16600, .F. ) ;
#10678 = ORIENTED_EDGE ( 'NONE', *, *, #14883, .F. ) ;
#10679 = CARTESIAN_POINT ( 'NONE',  ( -62.09248695497047521, -2.506581153329065170, -0.3044590188957451149 ) ) ;
#10680 = CARTESIAN_POINT ( 'NONE',  ( -58.67292740578360366, 1.073804522883521351, 3.225979517392336682 ) ) ;
#10682 = CARTESIAN_POINT ( 'NONE',  ( -61.34999999999997300, -2.569640616537276490, 0.6664830392735136000 ) ) ;
#10681 = CARTESIAN_POINT ( 'NONE',  ( -55.31249999999997158, -1.962990915244707368, -3.400000000000203304 ) ) ;
#10683 = VERTEX_POINT ( 'NONE', #29127 ) ;
#10684 = VERTEX_POINT ( 'NONE', #12328 ) ;
#10685 = CIRCLE ( 'NONE', #12206, 0.4576450603546982632 ) ;
#10686 = EDGE_LOOP ( 'NONE', ( #2519, #9138, #234, #8250, #10224 ) ) ;
#10687 = EDGE_CURVE ( 'NONE', #21368, #28904, #25743, .T. ) ;
#10688 = DIRECTION ( 'NONE',  ( 0.000000000000000000, 0.000000000000000000, 1.000000000000000000 ) ) ;
#10689 = VERTEX_POINT ( 'NONE', #24836 ) ;
#10690 = CARTESIAN_POINT ( 'NONE',  ( 23.88937651016952657, 5.720041407194943694, -1.950000000000082112 ) ) ;
#10691 = B_SPLINE_CURVE_WITH_KNOTS ( 'NONE', 3,
 ( #1484, #16060, #20967, #18437 ),
 .UNSPECIFIED., .F., .F.,
 ( 4, 4 ),
 ( 0.000000000000000000, 6.653267247438212099E-05 ),
 .UNSPECIFIED. ) ;
#10692 = SPHERICAL_SURFACE ( 'NONE', #26320, 0.05000000000000000278 ) ;
#10693 = CARTESIAN_POINT ( 'NONE',  ( -58.87499999999996447, 2.944486372867118007, -1.700000000000177147 ) ) ;
#10694 = DIRECTION ( 'NONE',  ( 0.000000000000000000, -0.9996898646859344595, -0.02490330187381124480 ) ) ;
#10695 = CARTESIAN_POINT ( 'NONE',  ( -58.89405989232411542, -2.944486372867076263, -1.700000000000219558 ) ) ;
#10696 = CARTESIAN_POINT ( 'NONE',  ( 47.88101986748534244, -3.908336255397547809, 1.238913925478448252 ) ) ;
#10697 = CARTESIAN_POINT ( 'NONE',  ( 51.70000000000000995, -4.020776289669855785, -2.234582293948758736 ) ) ;
#10698 = EDGE_CURVE ( 'NONE', #25407, #9597, #946, .T. ) ;
#10699 = AXIS2_PLACEMENT_3D ( 'NONE', #26359, #26828, #2457 ) ;
#10700 = DIRECTION ( 'NONE',  ( 1.000000000000000000, 0.000000000000000000, -0.000000000000000000 ) ) ;
#10701 = DIRECTION ( 'NONE',  ( -1.000000000000000000, -3.053848253006669023E-16, 2.042510438544995415E-16 ) ) ;
#10703 = CARTESIAN_POINT ( 'NONE',  ( 50.93238199930985388, -4.417905785811345076, 1.285520522239830044 ) ) ;
#10702 = CARTESIAN_POINT ( 'NONE',  ( -59.49038236770705623, 3.145408112564967773, 1.387068135838901428 ) ) ;
#10704 = DIRECTION ( 'NONE',  ( -1.000000000000000000, 1.219044193948983948E-29, -3.491481338843133355E-15 ) ) ;
#10705 = CARTESIAN_POINT ( 'NONE',  ( 50.83686442967772479, 8.734989671305513070, -2.050000000000176570 ) ) ;
#10706 = DIRECTION ( 'NONE',  ( 1.000000000000000000, 0.000000000000000000, 0.000000000000000000 ) ) ;
#10707 = ORIENTED_EDGE ( 'NONE', *, *, #12781, .F. ) ;
#10708 = CARTESIAN_POINT ( 'NONE',  ( 51.31757909864148104, -1.004435980685438157, -1.391945786376508343 ) ) ;
#10709 = CARTESIAN_POINT ( 'NONE',  ( 54.42157938624325197, 6.359826701677585348, 2.020140340243033350 ) ) ;
#10710 = EDGE_LOOP ( 'NONE', ( #15384, #19596, #31067, #17692 ) ) ;
#10711 = CARTESIAN_POINT ( 'NONE',  ( 58.75000000000003553, -1.470078920827915470, 1.470078920827824209 ) ) ;
#10712 = VERTEX_POINT ( 'NONE', #27988 ) ;
#10713 = CYLINDRICAL_SURFACE ( 'NONE', #3613, 2.800000000000000266 ) ;
#10714 = CARTESIAN_POINT ( 'NONE',  ( -36.22909104983321527, -5.326676561279865219, 0.9978806102897157526 ) ) ;
#10716 = CYLINDRICAL_SURFACE ( 'NONE', #9085, 0.1000000000000000472 ) ;
#10715 = DIRECTION ( 'NONE',  ( 0.000000000000000000, 0.000000000000000000, 1.000000000000000000 ) ) ;
#10717 = ORIENTED_EDGE ( 'NONE', *, *, #18097, .T. ) ;
#10718 = CARTESIAN_POINT ( 'NONE',  ( 60.87107532335728166, -0.5000002988016893912, -1.554802360349110790 ) ) ;
#10719 = EDGE_CURVE ( 'NONE', #30422, #9190, #20737, .T. ) ;
#10720 = CARTESIAN_POINT ( 'NONE',  ( 57.00630022123013418, -0.7249518695496515175, -1.800067615291236711 ) ) ;
#10721 = VERTEX_POINT ( 'NONE', #1091 ) ;
#10723 = DIRECTION ( 'NONE',  ( 1.000000000000000000, 2.586136946169074517E-16, -0.000000000000000000 ) ) ;
#10722 = DIRECTION ( 'NONE',  ( 0.000000000000000000, 0.000000000000000000, -1.000000000000000000 ) ) ;
#10724 = LINE ( 'NONE', #8346, #8855 ) ;
#10725 = ORIENTED_EDGE ( 'NONE', *, *, #4429, .F. ) ;
#10726 = AXIS2_PLACEMENT_3D ( 'NONE', #9468, #21676, #19134 ) ;
#10727 = CARTESIAN_POINT ( 'NONE',  ( -36.25997906085253675, 4.878092280899812394, -1.814329181850203865 ) ) ;
#10728 = EDGE_CURVE ( 'NONE', #21568, #22153, #4500, .T. ) ;
#10729 = CARTESIAN_POINT ( 'NONE',  ( -54.51905989232412963, -2.944486372867088697, 1.699999999999795008 ) ) ;
#10730 = CARTESIAN_POINT ( 'NONE',  ( -74.39999999999997726, 0.4598573377555272290, 0.01145551886195788488 ) ) ;
#10731 = CARTESIAN_POINT ( 'NONE',  ( 51.50435016707358926, -0.9265794315402072767, 1.339215852266877782 ) ) ;
#10732 = VERTEX_POINT ( 'NONE', #1231 ) ;
#10733 = EDGE_CURVE ( 'NONE', #10599, #4028, #22210, .T. ) ;
#10734 = CARTESIAN_POINT ( 'NONE',  ( 15.74504787372188908, 3.003531019938586955, 4.498666779076369693 ) ) ;
#10735 = CIRCLE ( 'NONE', #3724, 0.5000000000000013323 ) ;
#10736 = APPLICATION_CONTEXT ( 'automotive_design' ) ;
#10737 = FACE_OUTER_BOUND ( 'NONE', #31113, .T. ) ;
#10738 = B_SPLINE_CURVE_WITH_KNOTS ( 'NONE', 3,
 ( #2756, #22095, #14931, #10052, #5278, #7808, #19721, #29356, #26970, #2919, #19864, #10807, #28058, #30584, #6375, #13789 ),
 .UNSPECIFIED., .F., .F.,
 ( 4, 3, 3, 3, 3, 4 ),
 ( 0.000000000000000000, 2.009849036138677304E-05, 3.995053695856421648E-05, 5.889062715234580982E-05, 7.635198602698413037E-05, 8.503766575809868053E-05 ),
 .UNSPECIFIED. ) ;
#10739 = EDGE_CURVE ( 'NONE', #8076, #3273, #3764, .T. ) ;
#10740 = CARTESIAN_POINT ( 'NONE',  ( -58.19702994616203284, -2.078460969082624565, -3.600000000000216360 ) ) ;
#10741 = DIRECTION ( 'NONE',  ( 1.282749433769087582E-30, 1.000000000000000000, 1.224646799147353207E-16 ) ) ;
#10742 = CARTESIAN_POINT ( 'NONE',  ( 25.68828371051467130, 5.335084521667699420, 2.049999999999909228 ) ) ;
#10743 = ORIENTED_EDGE ( 'NONE', *, *, #15038, .F. ) ;
#10744 = CYLINDRICAL_SURFACE ( 'NONE', #22432, 1.000000000000000000 ) ;
#10745 = ORIENTED_EDGE ( 'NONE', *, *, #11947, .T. ) ;
#10746 = UNCERTAINTY_MEASURE_WITH_UNIT (LENGTH_MEASURE( 1.000000000000000082E-05 ), #30587, 'distance_accuracy_value', 'NONE');
#10747 = FACE_OUTER_BOUND ( 'NONE', #18723, .T. ) ;
#10749 = CARTESIAN_POINT ( 'NONE',  ( 58.75000000000002842, -1.106298139389714663, -1.666164585742599513 ) ) ;
#10748 = DIRECTION ( 'NONE',  ( -1.000000000000000000, -3.053848253006669023E-16, 2.042510438544995415E-16 ) ) ;
#10750 = ORIENTED_EDGE ( 'NONE', *, *, #10288, .F. ) ;
#10751 = ORIENTED_EDGE ( 'NONE', *, *, #5718, .F. ) ;
#10752 = CARTESIAN_POINT ( 'NONE',  ( -59.08155989232413674, -1.962990915244734236, 3.399999999999780975 ) ) ;
#10753 = ADVANCED_FACE ( 'NONE', ( #30048 ), #25112, .F. ) ;
#10754 = CARTESIAN_POINT ( 'NONE',  ( 23.27131915274574681, 6.595123925190214287, 1.424999999999918332 ) ) ;
#10755 = ORIENTED_EDGE ( 'NONE', *, *, #13112, .F. ) ;
#10757 = CARTESIAN_POINT ( 'NONE',  ( 61.25000000000000711, 1.666164585743243665, -1.106298139389324975 ) ) ;
#10756 = CARTESIAN_POINT ( 'NONE',  ( -57.75952994616205416, -4.643455692769894075E-15, 3.599999999999794031 ) ) ;
#10758 = CARTESIAN_POINT ( 'NONE',  ( -57.73542740578360366, -3.725040285533365303, 1.239922660687675204 ) ) ;
#10759 = CIRCLE ( 'NONE', #14797, 4.314644660940672338 ) ;
#10760 = DIRECTION ( 'NONE',  ( 1.000000000000000000, -0.000000000000000000, -1.047444401652940007E-14 ) ) ;
#10761 = APPLICATION_PROTOCOL_DEFINITION ( 'draft international standard', 'automotive_design', 1998, #486 ) ;
#10762 = CARTESIAN_POINT ( 'NONE',  ( -59.59999999999998721, 2.022492213459062160, 1.712315755489264513 ) ) ;
#10763 = ORIENTED_EDGE ( 'NONE', *, *, #9667, .F. ) ;
#10764 = ADVANCED_FACE ( 'NONE', ( #12792 ), #237, .T. ) ;
#10765 = CARTESIAN_POINT ( 'NONE',  ( -62.09999999999997300, -2.509696570289218442, -0.2775754403374581791 ) ) ;
#10766 = CARTESIAN_POINT ( 'NONE',  ( 53.55869261961971972, 7.702978059423484680, -2.050000000000185896 ) ) ;
#10767 = CARTESIAN_POINT ( 'NONE',  ( 48.40130545986176003, -0.9107929593199913798, -3.923749358243191043 ) ) ;
#10768 = FACE_OUTER_BOUND ( 'NONE', #29088, .T. ) ;
#10769 = FACE_OUTER_BOUND ( 'NONE', #206, .T. ) ;
#10771 = CARTESIAN_POINT ( 'NONE',  ( 58.74999981404336324, -1.909395380151198252, -0.4234853497079255624 ) ) ;
#10770 = CARTESIAN_POINT ( 'NONE',  ( 31.20024169534877601, 7.859880414064924103, -1.425000000000108402 ) ) ;
#10772 = AXIS2_PLACEMENT_3D ( 'NONE', #12493, #27520, #20122 ) ;
#10773 = AXIS2_PLACEMENT_3D ( 'NONE', #3516, #3191, #3658 ) ;
#10774 = ADVANCED_FACE ( 'NONE', ( #15954 ), #25931, .F. ) ;
#10775 = DIRECTION ( 'NONE',  ( 0.000000000000000000, 0.000000000000000000, -1.000000000000000000 ) ) ;
#10776 = DIRECTION ( 'NONE',  ( -1.727378680347082743E-15, 0.9428090415820579162, -0.3333333333333488580 ) ) ;
#10778 = DIRECTION ( 'NONE',  ( -1.000000000000000000, -3.053848253006669023E-16, 2.042510438544995415E-16 ) ) ;
#10777 = DIRECTION ( 'NONE',  ( -3.491481338843133355E-15, -3.491481338843133355E-15, 1.000000000000000000 ) ) ;
#10779 = ORIENTED_EDGE ( 'NONE', *, *, #30590, .T. ) ;
#10780 = CYLINDRICAL_SURFACE ( 'NONE', #7366, 2.700000000000000178 ) ;
#10781 = EDGE_CURVE ( 'NONE', #18960, #15811, #19152, .T. ) ;
#10782 = CARTESIAN_POINT ( 'NONE',  ( -36.52757395963737963, 2.413203405699283710, -4.840238007535727860 ) ) ;
#10784 = CARTESIAN_POINT ( 'NONE',  ( 47.38264676386181407, -3.967853068034124853, -1.365472663301307232 ) ) ;
#10783 = CARTESIAN_POINT ( 'NONE',  ( 15.49676243306308621, 3.102491976071176882, -4.173461118157685057 ) ) ;
#10785 = DIRECTION ( 'NONE',  ( 0.7071067811865487940, -0.1420552074174027679, 0.6926906366088665390 ) ) ;
#10786 = ORIENTED_EDGE ( 'NONE', *, *, #17782, .T. ) ;
#10787 = CARTESIAN_POINT ( 'NONE',  ( 53.75840399023272198, 7.746411475361852261, 2.049999999999812417 ) ) ;
#10788 = CARTESIAN_POINT ( 'NONE',  ( 47.00305898648056768, -4.143816080048276618, 1.075455348895917762 ) ) ;
#10789 = ORIENTED_EDGE ( 'NONE', *, *, #24374, .F. ) ;
#10790 = EDGE_CURVE ( 'NONE', #27880, #15664, #27136, .T. ) ;
#10791 = DIRECTION ( 'NONE',  ( 1.000000000000000000, 0.000000000000000000, -3.491481338843133355E-15 ) ) ;
#10792 = VERTEX_POINT ( 'NONE', #3080 ) ;
#10793 = EDGE_CURVE ( 'NONE', #16714, #7404, #6010, .T. ) ;
#10794 = CARTESIAN_POINT ( 'NONE',  ( 58.50000000000001421, 0.8156862745098042433, 2.468735688885369317 ) ) ;
#10795 = CARTESIAN_POINT ( 'NONE',  ( 58.65000000000000568, 1.590093208333579256, -0.9941784314382211551 ) ) ;
#10796 = ORIENTED_EDGE ( 'NONE', *, *, #27010, .T. ) ;
#10797 = CARTESIAN_POINT ( 'NONE',  ( 31.30765689092466530, 7.353940011527059895, 1.949999999999889599 ) ) ;
#10798 = CARTESIAN_POINT ( 'NONE',  ( -57.76905989232412963, 2.944486372867092250, 1.699999999999806111 ) ) ;
#10799 = ORIENTED_EDGE ( 'NONE', *, *, #22427, .T. ) ;
#10800 = VERTEX_POINT ( 'NONE', #22559 ) ;
#10801 = AXIS2_PLACEMENT_3D ( 'NONE', #31042, #19030, #20782 ) ;
#10802 = VERTEX_POINT ( 'NONE', #867 ) ;
#10803 = CARTESIAN_POINT ( 'NONE',  ( -58.68749999999998579, 1.962990915244722689, 3.399999999999799627 ) ) ;
#10804 = CARTESIAN_POINT ( 'NONE',  ( 49.00000000000002132, 1.401298464324817071E-42, -5.132477568099407673E-13 ) ) ;
#10805 = LINE ( 'NONE', #20489, #30419 ) ;
#10806 = DIRECTION ( 'NONE',  ( -1.000000000000000000, -3.053848253006669023E-16, 2.042510438544995415E-16 ) ) ;
#10807 = CARTESIAN_POINT ( 'NONE',  ( 57.03559403007977124, 0.7482252654948684523, 2.422430812887707230 ) ) ;
#10808 =( BOUNDED_CURVE ( )  B_SPLINE_CURVE ( 2, ( #9565, #30761, #30920, #6691, #16685, #25999, #28538, #16353, #30586 ),
 .UNSPECIFIED., .F., .T. ) 
 B_SPLINE_CURVE_WITH_KNOTS ( ( 3, 2, 2, 2, 3 ),
 ( 0.4722222222222222654, 0.4814814814814814548, 0.5000000000000000000, 0.5185185185185184897, 0.5277777777777777901 ),
 .UNSPECIFIED. ) 
 CURVE ( )  GEOMETRIC_REPRESENTATION_ITEM ( )  RATIONAL_B_SPLINE_CURVE ( ( 0.9330127018922194093, 0.9330127018922197424, 1.000000000000000000, 0.8660254037844387076, 1.000000000000000000, 0.8660254037844387076, 1.000000000000000000, 0.9330127018922194093, 0.9330127018922194093 ) ) 
 REPRESENTATION_ITEM ( '' )  );
#10810 = FACE_OUTER_BOUND ( 'NONE', #12927, .T. ) ;
#10809 = DIRECTION ( 'NONE',  ( 1.387778780781445676E-14, -1.734723475976807094E-15, 1.000000000000000000 ) ) ;
#10811 = B_SPLINE_CURVE_WITH_KNOTS ( 'NONE', 3,
 ( #20484, #25686, #8583, #20180, #22860, #15723, #29964, #18264, #3377, #22709, #18114, #1148, #15863, #3989, #13027, #27902 ),
 .UNSPECIFIED., .F., .F.,
 ( 4, 3, 3, 3, 3, 4 ),
 ( 0.000000000000000000, 1.391268354954338704E-05, 4.880039988305115829E-05, 8.637315450940535953E-05, 0.0001246458323646918982, 0.0001626605312951481396 ),
 .UNSPECIFIED. ) ;
#10812 = EDGE_CURVE ( 'NONE', #17625, #1825, #24914, .T. ) ;
#10813 = CARTESIAN_POINT ( 'NONE',  ( 58.67990267795905623, -0.4999999999993856026, 1.808383001045803073 ) ) ;
#10814 = CARTESIAN_POINT ( 'NONE',  ( -59.60127941732040568, 2.337454683939000688, -1.248534441610057444 ) ) ;
#10815 = EDGE_CURVE ( 'NONE', #21074, #16500, #11676, .T. ) ;
#10816 = CARTESIAN_POINT ( 'NONE',  ( -59.69619597676793887, 2.090631638210891374, 1.743547763621478452 ) ) ;
#10817 = CARTESIAN_POINT ( 'NONE',  ( -54.46462222424374033, 1.502185874895793694, -3.301501926143237675 ) ) ;
#10818 = DIRECTION ( 'NONE',  ( 1.000000000000000000, 0.000000000000000000, 0.000000000000000000 ) ) ;
#10819 = EDGE_CURVE ( 'NONE', #24615, #28796, #10150, .T. ) ;
#10820 = AXIS2_PLACEMENT_3D ( 'NONE', #26609, #475, #14731 ) ;
#10821 = ORIENTED_EDGE ( 'NONE', *, *, #15594, .T. ) ;
#10822 = CARTESIAN_POINT ( 'NONE',  ( 52.20711756518983293, 0.6500000000005468070, -1.489337100860647967 ) ) ;
#10823 = DIRECTION ( 'NONE',  ( 1.000000000000000000, -1.219044193948983948E-29, 3.491481338843133355E-15 ) ) ;
#10824 = ORIENTED_EDGE ( 'NONE', *, *, #3591, .F. ) ;
#10825 = ORIENTED_EDGE ( 'NONE', *, *, #7930, .F. ) ;
#10826 = CARTESIAN_POINT ( 'NONE',  ( -59.11151511461849850, 2.314313660749603763, 1.291265858342419248 ) ) ;
#10827 = PRODUCT_DEFINITION_SHAPE ( 'NONE', 'NONE',  #31330 ) ;
#10828 = VECTOR ( 'NONE', #23434, 999.9999999999998863 ) ;
#10829 = DIRECTION ( 'NONE',  ( 1.520093157366878429E-16, -0.5877852522924742473, 0.8090169943749465631 ) ) ;
#10831 = DIRECTION ( 'NONE',  ( 0.000000000000000000, 0.9507508458639141180, 0.3099561728519886206 ) ) ;
#10830 = CARTESIAN_POINT ( 'NONE',  ( -56.43749999999998579, 1.962990915244722689, 3.399999999999807621 ) ) ;
#10832 = EDGE_LOOP ( 'NONE', ( #5056, #30492, #22572, #8653 ) ) ;
#10833 = ORIENTED_EDGE ( 'NONE', *, *, #17555, .T. ) ;
#10834 = AXIS2_PLACEMENT_3D ( 'NONE', #23106, #1398, #11058 ) ;
#10835 = CARTESIAN_POINT ( 'NONE',  ( 51.77906683064299642, -4.146898708458731875, -1.994789398600458785 ) ) ;
#10836 = VERTEX_POINT ( 'NONE', #26733 ) ;
#10837 = CARTESIAN_POINT ( 'NONE',  ( -67.92156587216960872, -6.098012745906804249E-16, 3.386787660360170602E-15 ) ) ;
#10838 = ORIENTED_EDGE ( 'NONE', *, *, #29178, .T. ) ;
#10839 = CARTESIAN_POINT ( 'NONE',  ( -59.43788607448336592, -2.385332005665353972, -1.158943404468679494 ) ) ;
#10840 = DIRECTION ( 'NONE',  ( 1.000000000000000000, 0.000000000000000000, 0.000000000000000000 ) ) ;
#10841 = DIRECTION ( 'NONE',  ( 0.000000000000000000, 0.000000000000000000, 1.000000000000000000 ) ) ;
#10842 = LINE ( 'NONE', #22748, #22338 ) ;
#10843 = CARTESIAN_POINT ( 'NONE',  ( -59.39405989232410832, 2.944486372867106461, -1.700000000000198019 ) ) ;
#10844 = LINE ( 'NONE', #28098, #22549 ) ;
#10845 = CARTESIAN_POINT ( 'NONE',  ( 15.71019289815287578, 2.413203405699197557, 4.840238007535781151 ) ) ;
#10846 = FACE_OUTER_BOUND ( 'NONE', #6571, .T. ) ;
#10847 = CARTESIAN_POINT ( 'NONE',  ( -59.69999999999997442, 8.366749974758454467E-15, -2.120534355533670266E-13 ) ) ;
#10849 = PLANE ( 'NONE',  #20493 ) ;
#10848 = DIRECTION ( 'NONE',  ( -3.491481338843133355E-15, -3.491481338843133355E-15, 1.000000000000000000 ) ) ;
#10850 = CARTESIAN_POINT ( 'NONE',  ( -58.44184846062113081, 0.2309624077929140484, 3.875409454552789956 ) ) ;
#10851 = EDGE_CURVE ( 'NONE', #320, #4290, #7046, .T. ) ;
#10852 = CARTESIAN_POINT ( 'NONE',  ( 58.65000000000001279, 1.371849028670515835, 1.278599783849900806 ) ) ;
#10853 = DIRECTION ( 'NONE',  ( 0.000000000000000000, 0.000000000000000000, -1.000000000000000000 ) ) ;
#10854 = ORIENTED_EDGE ( 'NONE', *, *, #25138, .T. ) ;
#10855 = CIRCLE ( 'NONE', #4280, 2.000000000000000000 ) ;
#10856 = AXIS2_PLACEMENT_3D ( 'NONE', #2136, #7064, #26042 ) ;
#10857 = CARTESIAN_POINT ( 'NONE',  ( 54.28867365409861634, 5.640057820322910587, 1.963089969304594895 ) ) ;
#10858 = ORIENTED_EDGE ( 'NONE', *, *, #8251, .T. ) ;
#10859 = CARTESIAN_POINT ( 'NONE',  ( -59.64405989232410832, -2.944486372867071378, -1.700000000000230438 ) ) ;
#10860 = ORIENTED_EDGE ( 'NONE', *, *, #18558, .T. ) ;
#10861 = B_SPLINE_CURVE_WITH_KNOTS ( 'NONE', 3,
 ( #8328, #911, #22766, #20390, #9081, #21299 ),
 .UNSPECIFIED., .F., .F.,
 ( 4, 2, 4 ),
 ( 4.207835982932403546E-19, 0.0001531825249253921327, 0.0003063650498507838318 ),
 .UNSPECIFIED. ) ;
#10862 = CARTESIAN_POINT ( 'NONE',  ( 51.80000005504633975, 4.055700188233500647, 2.007411739157320074 ) ) ;
#10863 = CIRCLE ( 'NONE', #6325, 3.750000000000000444 ) ;
#10864 = CARTESIAN_POINT ( 'NONE',  ( -44.49999999999999289, 0.000000000000000000, 2.168404344971008868E-14 ) ) ;
#10866 = CARTESIAN_POINT ( 'NONE',  ( 51.67759423633589932, -3.662050566052894141, -1.846868639358791864 ) ) ;
#10865 = CARTESIAN_POINT ( 'NONE',  ( 58.75000000000002132, 6.153735859711025284E-13, 3.111507638930570854E-58 ) ) ;
#10867 = ORIENTED_EDGE ( 'NONE', *, *, #11165, .T. ) ;
#10868 = LINE ( 'NONE', #30189, #29075 ) ;
#10869 = EDGE_CURVE ( 'NONE', #22739, #26116, #26243, .T. ) ;
#10870 = CARTESIAN_POINT ( 'NONE',  ( -74.38999999999998636, -2.585162900687033808E-15, 4.707972083073595634E-15 ) ) ;
#10871 = ORIENTED_EDGE ( 'NONE', *, *, #864, .F. ) ;
#10873 = CARTESIAN_POINT ( 'NONE',  ( -54.49999999999996447, -1.433333333333312254, -4.054078878803088593 ) ) ;
#10872 = DIRECTION ( 'NONE',  ( 0.000000000000000000, 0.000000000000000000, -1.000000000000000000 ) ) ;
#10874 = AXIS2_PLACEMENT_3D ( 'NONE', #24705, #3017, #10293 ) ;
#10875 = FACE_OUTER_BOUND ( 'NONE', #4540, .T. ) ;
#10876 = EDGE_LOOP ( 'NONE', ( #18250, #4373, #29486, #28600 ) ) ;
#10877 = CARTESIAN_POINT ( 'NONE',  ( -36.42771574642738841, 4.977801270594329530, -2.126472881633125755 ) ) ;
#10878 = CARTESIAN_POINT ( 'NONE',  ( 69.25000000000000000, 0.4500000000000000111, -1.988246715074081461 ) ) ;
#10879 = CARTESIAN_POINT ( 'NONE',  ( -36.52757395963738674, -2.413203405699269055, 4.840238007535756282 ) ) ;
#10880 = DIRECTION ( 'NONE',  ( -1.000000000000000000, -1.047444401652940007E-14, -0.000000000000000000 ) ) ;
#10881 = CARTESIAN_POINT ( 'NONE',  ( 68.99999999999997158, 4.867971026610729436E-16, -3.950000000000722711 ) ) ;
#10883 = ORIENTED_EDGE ( 'NONE', *, *, #3641, .T. ) ;
#10882 = TOROIDAL_SURFACE ( 'NONE', #24532, 1.375000000000001332, 0.2500000000000000000 ) ;
#10884 = TOROIDAL_SURFACE ( 'NONE', #16987, 4.050000000000000711, 0.05000000000000000278 ) ;
#10885 = CARTESIAN_POINT ( 'NONE',  ( -61.58695197172909985, -2.476857586476660433, -0.4985707676156266865 ) ) ;
#10886 = VECTOR ( 'NONE', #10266, 1000.000000000000000 ) ;
#10887 = CYLINDRICAL_SURFACE ( 'NONE', #10912, 0.1499999999999999667 ) ;
#10888 = EDGE_CURVE ( 'NONE', #2488, #12162, #17082, .T. ) ;
#10889 = CONICAL_SURFACE ( 'NONE', #3792, 3.299999999999999822, 0.03997868712329010615 ) ;
#10890 = CYLINDRICAL_SURFACE ( 'NONE', #802, 4.849999999999999645 ) ;
#10891 = EDGE_CURVE ( 'NONE', #20368, #13704, #13076, .T. ) ;
#10892 = EDGE_CURVE ( 'NONE', #18214, #25246, #20187, .T. ) ;
#10893 = CARTESIAN_POINT ( 'NONE',  ( -56.82202994616205416, -4.156921938165296204, -2.272120436513089232E-13 ) ) ;
#10894 = CARTESIAN_POINT ( 'NONE',  ( 58.75000000694010538, -1.928945400590438730, -0.02494613115224967453 ) ) ;
#10895 = CARTESIAN_POINT ( 'NONE',  ( 33.37803294657273767, 8.220288670912871964, 2.049999999999885247 ) ) ;
#10896 = ORIENTED_EDGE ( 'NONE', *, *, #4817, .T. ) ;
#10897 = PLANE ( 'NONE',  #6240 ) ;
#10898 = VERTEX_POINT ( 'NONE', #2341 ) ;
#10899 = CARTESIAN_POINT ( 'NONE',  ( 58.65000000000001990, 6.143261415694495821E-13, 3.111507638930570854E-58 ) ) ;
#10901 = CARTESIAN_POINT ( 'NONE',  ( -59.69999999999997442, 8.366749974758454467E-15, -2.120534355533670266E-13 ) ) ;
#10900 = DIRECTION ( 'NONE',  ( 1.000000000000000000, 1.047444401652940007E-14, 0.000000000000000000 ) ) ;
#10902 = ORIENTED_EDGE ( 'NONE', *, *, #17181, .F. ) ;
#10903 = AXIS2_PLACEMENT_3D ( 'NONE', #18977, #28625, #13573 ) ;
#10904 = ORIENTED_EDGE ( 'NONE', *, *, #9078, .F. ) ;
#10905 = DIRECTION ( 'NONE',  ( -1.047444401652940007E-14, 0.000000000000000000, -1.000000000000000000 ) ) ;
#10906 = VECTOR ( 'NONE', #26589, 1000.000000000000000 ) ;
#10907 = EDGE_CURVE ( 'NONE', #10218, #1939, #2977, .T. ) ;
#10908 = DIRECTION ( 'NONE',  ( 1.000000000000000000, 1.047444401652940007E-14, 0.000000000000000000 ) ) ;
#10910 = CARTESIAN_POINT ( 'NONE',  ( -55.65835481156724285, 4.108500314926515351, -1.367561758111408565 ) ) ;
#10909 = CARTESIAN_POINT ( 'NONE',  ( -60.88452994616204705, 3.117691453623979481, 1.799999999999795985 ) ) ;
#10911 = CARTESIAN_POINT ( 'NONE',  ( -57.54792740578359656, -1.073804522883517132, -3.225979517392335350 ) ) ;
#10912 = AXIS2_PLACEMENT_3D ( 'NONE', #764, #29747, #17570 ) ;
#10913 = CARTESIAN_POINT ( 'NONE',  ( -54.49999999999997868, -4.276948333784438283, -0.9210526315789476781 ) ) ;
#10914 = ITEM_DEFINED_TRANSFORMATION ( 'NONE', 'NONE', #27773,  #9018 ) ;
#10915 = VECTOR ( 'NONE', #11605, 1000.000000000000000 ) ;
#10916 = CARTESIAN_POINT ( 'NONE',  ( 58.75000000000000000, 2.008165151418861427, -0.5380862305899540843 ) ) ;
#10917 = AXIS2_PLACEMENT_3D ( 'NONE', #25298, #15940, #16118 ) ;
#10918 = ORIENTED_EDGE ( 'NONE', *, *, #2468, .T. ) ;
#10919 = AXIS2_PLACEMENT_3D ( 'NONE', #18257, #3670, #27897 ) ;
#10920 = CARTESIAN_POINT ( 'NONE',  ( -60.59999999999997300, 1.626093840209163176E-15, 1.891350188320046374E-15 ) ) ;
#10921 = CARTESIAN_POINT ( 'NONE',  ( 52.61915120152472269, 4.492597126270304386, -2.050000000000182787 ) ) ;
#10922 = FACE_OUTER_BOUND ( 'NONE', #22457, .T. ) ;
#10923 = CARTESIAN_POINT ( 'NONE',  ( 15.03925126672127810, -0.4576450603546984852, 5.200000000000000178 ) ) ;
#10924 = AXIS2_PLACEMENT_3D ( 'NONE', #13225, #10706, #10853 ) ;
#10925 = FACE_OUTER_BOUND ( 'NONE', #27752, .T. ) ;
#10926 = EDGE_CURVE ( 'NONE', #11953, #5317, #6508, .T. ) ;
#10927 = AXIS2_PLACEMENT_3D ( 'NONE', #25232, #18131, #1019 ) ;
#10929 = DIRECTION ( 'NONE',  ( 1.000000000000000000, -0.000000000000000000, -0.000000000000000000 ) ) ;
#10928 = LINE ( 'NONE', #12822, #2389 ) ;
#10930 = EDGE_CURVE ( 'NONE', #23943, #29251, #17147, .T. ) ;
#10931 = TOROIDAL_SURFACE ( 'NONE', #2846, 4.275000000000000355, 0.1000000000000000056 ) ;
#10932 = LINE ( 'NONE', #8401, #24593 ) ;
#10933 = CIRCLE ( 'NONE', #6404, 0.1000000000000000472 ) ;
#10935 = DIRECTION ( 'NONE',  ( 1.000000000000000000, 3.053848253006669023E-16, -2.042510438544995415E-16 ) ) ;
#10934 = CARTESIAN_POINT ( 'NONE',  ( 58.64999999999999858, 1.782657835995388407, -0.5811678240976838605 ) ) ;
#10936 = VERTEX_POINT ( 'NONE', #30294 ) ;
#10937 = VECTOR ( 'NONE', #14091, 1000.000000000000000 ) ;
#10938 = DIRECTION ( 'NONE',  ( 0.000000000000000000, 0.000000000000000000, 1.000000000000000000 ) ) ;
#10939 = CIRCLE ( 'NONE', #4365, 0.1000000000000001027 ) ;
#10940 = CARTESIAN_POINT ( 'NONE',  ( 15.03925126672132784, 4.383220986679478237, 0.4611378927914913661 ) ) ;
#10942 = DIRECTION ( 'NONE',  ( -1.000000000000000000, 0.000000000000000000, 1.047444401652940007E-14 ) ) ;
#10941 = CARTESIAN_POINT ( 'NONE',  ( 27.72148966843208839, 5.417328426838181166, -1.425000000000096856 ) ) ;
#10943 = CARTESIAN_POINT ( 'NONE',  ( -74.39999999999997726, -1.249612330857420961, -0.03112912734225919270 ) ) ;
#10944 = ORIENTED_EDGE ( 'NONE', *, *, #23598, .T. ) ;
#10945 = CARTESIAN_POINT ( 'NONE',  ( 52.48761841068139233, 8.622213116012012790, 2.049999999999817302 ) ) ;
#10946 = CARTESIAN_POINT ( 'NONE',  ( 50.50000000000002132, -0.6462379109120509613, 4.048750000000023164 ) ) ;
#10947 = EDGE_CURVE ( 'NONE', #26911, #30652, #12575, .T. ) ;
#10948 = ORIENTED_EDGE ( 'NONE', *, *, #20145, .F. ) ;
#10949 = DIRECTION ( 'NONE',  ( -1.000000000000000000, -0.000000000000000000, -0.000000000000000000 ) ) ;
#10950 = ORIENTED_EDGE ( 'NONE', *, *, #9830, .F. ) ;
#10951 = VECTOR ( 'NONE', #16601, 1000.000000000000000 ) ;
#10952 = CARTESIAN_POINT ( 'NONE',  ( 15.70940947763170570, 2.412550141807490611, -4.840569432287314733 ) ) ;
#10953 = LINE ( 'NONE', #10501, #21582 ) ;
#10954 = VERTEX_POINT ( 'NONE', #15740 ) ;
#10955 = CIRCLE ( 'NONE', #2867, 1.000000000000000000 ) ;
#10956 = CARTESIAN_POINT ( 'NONE',  ( -56.13452994616205416, -3.117691453623978592, 1.799999999999785771 ) ) ;
#10957 = CARTESIAN_POINT ( 'NONE',  ( -59.39405989232410832, 2.944486372867106461, -1.700000000000198019 ) ) ;
#10958 = ORIENTED_EDGE ( 'NONE', *, *, #19574, .F. ) ;
#10959 = TOROIDAL_SURFACE ( 'NONE', #11458, 0.2000000000000000111, 0.1000000000000000056 ) ;
#10960 = CARTESIAN_POINT ( 'NONE',  ( -59.29999999999997584, 2.330309927981285032E-15, 4.253626757584724400E-16 ) ) ;
#10961 = ORIENTED_EDGE ( 'NONE', *, *, #22698, .F. ) ;
#10963 = ADVANCED_FACE ( 'NONE', ( #27921 ), #6235, .T. ) ;
#10962 = CIRCLE ( 'NONE', #23611, 1.250000000000000222 ) ;
#10964 = ORIENTED_EDGE ( 'NONE', *, *, #9400, .T. ) ;
#10965 = VECTOR ( 'NONE', #26439, 1000.000000000000000 ) ;
#10966 = CARTESIAN_POINT ( 'NONE',  ( -57.18749999999998579, 1.962990915244722689, 3.399999999999804956 ) ) ;
#10967 = AXIS2_PLACEMENT_3D ( 'NONE', #9234, #21128, #28231 ) ;
#10968 = AXIS2_PLACEMENT_3D ( 'NONE', #25415, #23216, #8939 ) ;
#10969 =( BOUNDED_SURFACE ( )  B_SPLINE_SURFACE ( 3, 2, ( 
 ( #1230, #768, #2998 ),
 ( #22325, #10435, #20117 ),
 ( #613, #29749, #10274 ),
 ( #27218, #13388, #11046 ),
 ( #13098, #10877, #20565 ),
 ( #8978, #23246, #10727 ),
 ( #23397, #11341, #1383 ),
 ( #27834, #8658, #22929 ),
 ( #20870, #3918, #1215 ),
 ( #22788, #30197, #20725 ),
 ( #16116, #8513, #18192 ),
 ( #1076, #6143, #28301 ),
 ( #20408, #27675, #30497 ),
 ( #8802, #18339, #3748 ),
 ( #30352, #5997, #1536 ),
 ( #23087, #18653, #27974 ) ),
 .UNSPECIFIED., .F., .F., .F. ) 
 B_SPLINE_SURFACE_WITH_KNOTS ( ( 4, 2, 2, 2, 2, 2, 2, 4 ),
 ( 3, 3 ),
 ( 0.001780502285214233520, 0.002558945925323761160, 0.002753556835351143178, 0.002948167745378525197, 0.003337389565433289233, 0.003726611385488053270, 0.004115833205542817307, 0.004894276845652345380 ),
 ( 0.000000000000000000, 1.000000000000000000 ),
 .UNSPECIFIED. ) 
 GEOMETRIC_REPRESENTATION_ITEM ( )  RATIONAL_B_SPLINE_SURFACE ( (
 ( 1.000000000000000000, 0.9418517008537252710, 1.000000000000000000),
 ( 1.000000000000000000, 0.9417987965886061019, 1.000000000000000000),
 ( 1.000000000000000000, 0.9418198861732800520, 1.000000000000000000),
 ( 1.000000000000000000, 0.9434060303845909212, 1.000000000000000000),
 ( 1.000000000000000000, 0.9437939819948288900, 1.000000000000000000),
 ( 1.000000000000000000, 0.9445989566712711394, 1.000000000000000000),
 ( 1.000000000000000000, 0.9450169930049940881, 1.000000000000000000),
 ( 1.000000000000000000, 0.9461610507673398063, 1.000000000000000000),
 ( 1.000000000000000000, 0.9467217966426996201, 1.000000000000000000),
 ( 1.000000000000000000, 0.9467345476124578996, 1.000000000000000000),
 ( 1.000000000000000000, 0.9461964028053386766, 1.000000000000000000),
 ( 1.000000000000000000, 0.9446801822473422927, 1.000000000000000000),
 ( 1.000000000000000000, 0.9437582546536400496, 1.000000000000000000),
 ( 1.000000000000000000, 0.9418129560295983582, 1.000000000000000000),
 ( 1.000000000000000000, 0.9418016889777277578, 1.000000000000000000),
 ( 1.000000000000000000, 0.9418517008537247159, 1.000000000000000000) ) ) 
 REPRESENTATION_ITEM ( '' )  SURFACE ( )  );
#10970 = DIRECTION ( 'NONE',  ( 1.000000000000000000, -0.000000000000000000, -0.000000000000000000 ) ) ;
#10971 = CARTESIAN_POINT ( 'NONE',  ( 58.66133336607610005, 1.640092727267837169, 0.9092995659222322669 ) ) ;
#10972 = CYLINDRICAL_SURFACE ( 'NONE', #26610, 3.200000000000000178 ) ;
#10973 = CARTESIAN_POINT ( 'NONE',  ( -54.49999999999996447, -1.993349740317589935, -2.907263629733159327 ) ) ;
#10974 = EDGE_CURVE ( 'NONE', #27518, #9761, #8049, .T. ) ;
#10976 = FACE_OUTER_BOUND ( 'NONE', #3907, .T. ) ;
#10975 = CARTESIAN_POINT ( 'NONE',  ( -44.49999999999998579, 4.529787229198778726E-28, -0.7500000000000185407 ) ) ;
#10977 = EDGE_CURVE ( 'NONE', #17715, #12157, #15882, .T. ) ;
#10978 = CIRCLE ( 'NONE', #28691, 4.100000000000022737 ) ;
#10979 = EDGE_CURVE ( 'NONE', #22153, #7818, #1249, .T. ) ;
#10980 = AXIS2_PLACEMENT_3D ( 'NONE', #439, #17542, #27194 ) ;
#10981 = FILL_AREA_STYLE ('',( #23018 ) ) ;
#10982 = FACE_OUTER_BOUND ( 'NONE', #28895, .T. ) ;
#10983 = DIRECTION ( 'NONE',  ( 1.000000000000000000, 1.047444401652940007E-14, 0.000000000000000000 ) ) ;
#10984 = CARTESIAN_POINT ( 'NONE',  ( 53.91574522235882228, 6.672251602522421443, 1.774295301432037286 ) ) ;
#10986 = DIRECTION ( 'NONE',  ( 0.000000000000000000, 0.000000000000000000, -1.000000000000000000 ) ) ;
#10985 = CIRCLE ( 'NONE', #28699, 0.1500000000000001887 ) ;
#10987 = CARTESIAN_POINT ( 'NONE',  ( -59.29999999999996874, -0.4436653460577585362, 3.502232364094418848 ) ) ;
#10988 = VERTEX_POINT ( 'NONE', #6387 ) ;
#10989 = CARTESIAN_POINT ( 'NONE',  ( -54.49999999999999289, -3.477081265201396931, 0.03376528397541268128 ) ) ;
#10990 = SURFACE_STYLE_USAGE ( .BOTH. , #25538 ) ;
#10991 = AXIS2_PLACEMENT_3D ( 'NONE', #1706, #21228, #25944 ) ;
#10992 = EDGE_LOOP ( 'NONE', ( #19122, #4750, #28323, #28078, #5939, #8820, #19927 ) ) ;
#10993 = CIRCLE ( 'NONE', #28704, 0.4500000000000001221 ) ;
#10994 = DIRECTION ( 'NONE',  ( 0.000000000000000000, -1.000000000000000000, -3.491481338843133355E-15 ) ) ;
#10995 = CARTESIAN_POINT ( 'NONE',  ( 60.97860563121728461, 0.7618031158903413314, -1.436139941719672297 ) ) ;
#10997 = CARTESIAN_POINT ( 'NONE',  ( 48.00000000000002132, -4.319730106884873244, 1.256953381662069269 ) ) ;
#10996 = CARTESIAN_POINT ( 'NONE',  ( -56.93749999999997158, -3.925981830489445379, -2.163561077067149631E-13 ) ) ;
#10998 = ORIENTED_EDGE ( 'NONE', *, *, #6388, .T. ) ;
#10999 = ORIENTED_EDGE ( 'NONE', *, *, #10891, .F. ) ;
#11000 = FACE_OUTER_BOUND ( 'NONE', #3828, .T. ) ;
#11001 = ORIENTED_EDGE ( 'NONE', *, *, #6391, .T. ) ;
#11002 = LINE ( 'NONE', #20683, #18222 ) ;
#11003 = ORIENTED_EDGE ( 'NONE', *, *, #31306, .F. ) ;
#11004 = CARTESIAN_POINT ( 'NONE',  ( 22.61091062207862379, 6.637672121856656560, -2.050000000000011813 ) ) ;
#11005 = AXIS2_PLACEMENT_3D ( 'NONE', #28298, #6606, #23545 ) ;
#11006 = EDGE_CURVE ( 'NONE', #20370, #28796, #3488, .T. ) ;
#11007 = PLANE ( 'NONE',  #17725 ) ;
#11008 = ORIENTED_EDGE ( 'NONE', *, *, #7036, .F. ) ;
#11009 = AXIS2_PLACEMENT_3D ( 'NONE', #24920, #14949, #3085 ) ;
#11010 =( BOUNDED_CURVE ( )  B_SPLINE_CURVE ( 2, ( #8314, #17986, #27635, #3578, #22898, #11017, #18625, #28424, #16558 ),
 .UNSPECIFIED., .F., .T. ) 
 B_SPLINE_CURVE_WITH_KNOTS ( ( 3, 2, 2, 2, 3 ),
 ( 0.5277777777777777901, 0.5370370370370370905, 0.5555555555555555802, 0.5740740740740740700, 0.5833333333333333703 ),
 .UNSPECIFIED. ) 
 CURVE ( )  GEOMETRIC_REPRESENTATION_ITEM ( )  RATIONAL_B_SPLINE_CURVE ( ( 0.9330127018922194093, 0.9330127018922194093, 1.000000000000000000, 0.8660254037844387076, 1.000000000000000000, 0.8660254037844387076, 1.000000000000000000, 0.9330127018922189652, 0.9330127018922194093 ) ) 
 REPRESENTATION_ITEM ( '' )  );
#11011 = AXIS2_PLACEMENT_3D ( 'NONE', #2646, #24337, #22290 ) ;
#11012 = DIRECTION ( 'NONE',  ( 1.000000000000000000, 0.000000000000000000, 0.000000000000000000 ) ) ;
#11013 = EDGE_CURVE ( 'NONE', #14828, #4631, #2237, .T. ) ;
#11014 = CARTESIAN_POINT ( 'NONE',  ( 52.10126625705172643, -0.5195911883732953207, -1.546252172343134390 ) ) ;
#11015 = CARTESIAN_POINT ( 'NONE',  ( 51.35663036796566416, -1.000990641333583175, 1.398271059358102475 ) ) ;
#11016 = B_SPLINE_CURVE_WITH_KNOTS ( 'NONE', 3,
 ( #14281, #42, #7479, #11753 ),
 .UNSPECIFIED., .F., .F.,
 ( 4, 4 ),
 ( 0.000000000000000000, 0.0001956043251250877066 ),
 .UNSPECIFIED. ) ;
#11017 = CARTESIAN_POINT ( 'NONE',  ( -57.90835481156723574, 4.108500314926515351, -1.367561758111408121 ) ) ;
#11018 = CARTESIAN_POINT ( 'NONE',  ( 48.00000000000001421, -4.003661535119149129, -1.269131321892086106 ) ) ;
#11019 = TOROIDAL_SURFACE ( 'NONE', #7093, 1.649144805949033898, 0.05000000000000000278 ) ;
#11020 = CARTESIAN_POINT ( 'NONE',  ( 67.95000000000005969, 5.021051876503122852E-16, 4.099999999999288214 ) ) ;
#11021 = DIRECTION ( 'NONE',  ( 0.000000000000000000, 0.3333333333333378667, -0.9428090415820618020 ) ) ;
#11023 = CARTESIAN_POINT ( 'NONE',  ( 50.80000000000001137, -4.417905791132255899, 1.285520503972564343 ) ) ;
#11022 = CARTESIAN_POINT ( 'NONE',  ( -61.13542439536123396, -2.577561284301780109, 0.8105868630520219886 ) ) ;
#11024 = ADVANCED_FACE ( 'NONE', ( #25706 ), #8605, .F. ) ;
#11025 = FACE_OUTER_BOUND ( 'NONE', #12088, .T. ) ;
#11026 = CARTESIAN_POINT ( 'NONE',  ( -59.09585481156723574, -2.489203624310587504, 2.804704140674918911 ) ) ;
#11027 = DIRECTION ( 'NONE',  ( 3.304235192336781034E-15, 0.000000000000000000, 1.000000000000000000 ) ) ;
#11028 = ORIENTED_EDGE ( 'NONE', *, *, #26483, .F. ) ;
#11029 = CIRCLE ( 'NONE', #25178, 0.04999999999999980849 ) ;
#11030 = CARTESIAN_POINT ( 'NONE',  ( -59.18749999999996447, 0.7533615035078157218, -3.673546848079175309 ) ) ;
#11031 = ORIENTED_EDGE ( 'NONE', *, *, #10059, .F. ) ;
#11032 = CARTESIAN_POINT ( 'NONE',  ( -59.51905989232410121, 2.606710529076650314E-14, -3.400000000000210854 ) ) ;
#11033 = ORIENTED_EDGE ( 'NONE', *, *, #13741, .F. ) ;
#11034 = CARTESIAN_POINT ( 'NONE',  ( 52.80702527127470347, 4.040723488129245311, 2.049999999999815969 ) ) ;
#11035 = CARTESIAN_POINT ( 'NONE',  ( -58.97085481156723574, -3.673546848079176197, -0.7533615035078063960 ) ) ;
#11037 = DIRECTION ( 'NONE',  ( 0.000000000000000000, 0.000000000000000000, -1.000000000000000000 ) ) ;
#11036 = DIRECTION ( 'NONE',  ( -2.459562394685754633E-16, 0.9510565162951565288, -0.3090169943749382919 ) ) ;
#11038 = EDGE_LOOP ( 'NONE', ( #29754, #5729, #2397, #21667 ) ) ;
#11039 = CARTESIAN_POINT ( 'NONE',  ( -71.44999999999998863, 0.4118376219175989839, -2.008205610283281040 ) ) ;
#11040 = LINE ( 'NONE', #7869, #2903 ) ;
#11041 = VERTEX_POINT ( 'NONE', #13657 ) ;
#11043 = DIRECTION ( 'NONE',  ( -1.000000000000000000, 0.000000000000000000, 0.000000000000000000 ) ) ;
#11042 = CARTESIAN_POINT ( 'NONE',  ( -60.49999999999995737, 1.963826825011730345E-15, 6.704595576490977020E-16 ) ) ;
#11044 = CARTESIAN_POINT ( 'NONE',  ( -35.85663232820584767, 3.817150320980632561, 2.203324261490556157 ) ) ;
#11045 = VERTEX_POINT ( 'NONE', #3694 ) ;
#11046 = CARTESIAN_POINT ( 'NONE',  ( -36.21152527658243514, 4.855742670514289649, -1.883114206442289218 ) ) ;
#11047 = EDGE_CURVE ( 'NONE', #11901, #16322, #23339, .T. ) ;
#11048 = DIRECTION ( 'NONE',  ( 1.000000000000000000, 2.586136946169074517E-16, -0.000000000000000000 ) ) ;
#11049 = ADVANCED_FACE ( 'NONE', ( #11282 ), #28539, .T. ) ;
#11050 = SURFACE_STYLE_FILL_AREA ( #4076 ) ;
#11051 = DIRECTION ( 'NONE',  ( -1.000000000000000000, 1.219044193948983948E-29, -3.491481338843133355E-15 ) ) ;
#11052 = EDGE_CURVE ( 'NONE', #22512, #16027, #6026, .T. ) ;
#11053 = AXIS2_PLACEMENT_3D ( 'NONE', #12200, #19487, #2695 ) ;
#11054 = CARTESIAN_POINT ( 'NONE',  ( 57.00000000000001421, -0.6999999999999999556, 1.820027472320129736 ) ) ;
#11055 = CARTESIAN_POINT ( 'NONE',  ( -57.73542740578359656, -3.725040285533367079, 1.239922660687670097 ) ) ;
#11056 = EDGE_CURVE ( 'NONE', #22413, #26613, #24123, .T. ) ;
#11057 = CARTESIAN_POINT ( 'NONE',  ( -56.53335481156723574, 0.7533615035078095046, -3.673546848079178861 ) ) ;
#11058 = DIRECTION ( 'NONE',  ( 0.000000000000000000, -0.2008964009354147484, 0.9796124928211139560 ) ) ;
#11059 = CARTESIAN_POINT ( 'NONE',  ( 58.75000018803721247, -1.936004331707231296, -0.04945370822344325595 ) ) ;
#11060 = DIRECTION ( 'NONE',  ( 1.000000000000000000, -1.219044193948983948E-29, 3.491481338843133355E-15 ) ) ;
#11061 = ORIENTED_EDGE ( 'NONE', *, *, #8987, .F. ) ;
#11062 = FACE_OUTER_BOUND ( 'NONE', #10447, .T. ) ;
#11063 = ORIENTED_EDGE ( 'NONE', *, *, #19157, .T. ) ;
#11064 = CARTESIAN_POINT ( 'NONE',  ( 47.10000000000000853, 2.480048031931718505E-14, -4.200000000000157385 ) ) ;
#11066 = CARTESIAN_POINT ( 'NONE',  ( 41.48619405471885102, -151.3359592902621955, 1.949999999999835865 ) ) ;
#11065 = CARTESIAN_POINT ( 'NONE',  ( -61.34999999999997300, -2.435425537339440449, 0.6665789166144534539 ) ) ;
#11067 = ORIENTED_EDGE ( 'NONE', *, *, #24260, .F. ) ;
#11068 = VERTEX_POINT ( 'NONE', #24277 ) ;
#11069 = CARTESIAN_POINT ( 'NONE',  ( 33.47623932017462778, 1.734723475976807094E-15, 0.000000000000000000 ) ) ;
#11070 = STYLED_ITEM ( 'NONE', ( #20000 ), #27074 ) ;
#11071 = CARTESIAN_POINT ( 'NONE',  ( 56.95000000000001705, 0.000000000000000000, 0.000000000000000000 ) ) ;
#11073 = CARTESIAN_POINT ( 'NONE',  ( -54.49999999999999289, 1.499999999999996003, 3.959797974644419849 ) ) ;
#11072 = DIRECTION ( 'NONE',  ( 3.491481338843133750E-15, 0.000000000000000000, 1.000000000000000000 ) ) ;
#11074 = ORIENTED_EDGE ( 'NONE', *, *, #30476, .F. ) ;
#11075 = CARTESIAN_POINT ( 'NONE',  ( -55.73542740578360366, 2.936324665650206889, 2.606018187048498191 ) ) ;
#11076 = DIRECTION ( 'NONE',  ( 1.983166172879301074E-16, 0.9119702176296790030, -0.4102564102564101312 ) ) ;
#11077 = ITEM_DEFINED_TRANSFORMATION ( 'NONE', 'NONE', #19705,  #9018 ) ;
#11078 = EDGE_CURVE ( 'NONE', #6036, #17943, #19066, .T. ) ;
#11079 = CARTESIAN_POINT ( 'NONE',  ( -54.49999999999996447, -1.993349740317589935, -2.907263629733159327 ) ) ;
#11080 = EDGE_CURVE ( 'NONE', #17704, #11119, #2987, .T. ) ;
#11081 = CIRCLE ( 'NONE', #12592, 5.338914163118009704 ) ;
#11082 = VERTEX_POINT ( 'NONE', #31250 ) ;
#11083 = CARTESIAN_POINT ( 'NONE',  ( 47.09347798666725282, -4.179189514726790122, -0.9999999999996743716 ) ) ;
#11084 = CARTESIAN_POINT ( 'NONE',  ( -35.85663232820579793, 2.199885893005987914, -4.939696249117657700 ) ) ;
#11085 = CARTESIAN_POINT ( 'NONE',  ( 58.65000000000004121, -1.656030381686081743, -0.8799718970820468167 ) ) ;
#11086 = CARTESIAN_POINT ( 'NONE',  ( 67.95000000000003126, -1.025519176787267142E-28, -7.117384709231726808E-13 ) ) ;
#11087 = LINE ( 'NONE', #22833, #25555 ) ;
#11088 = CIRCLE ( 'NONE', #15137, 0.2500000000000002220 ) ;
#11089 = EDGE_CURVE ( 'NONE', #3444, #24741, #29051, .T. ) ;
#11091 = CARTESIAN_POINT ( 'NONE',  ( 51.25000000000001421, 1.100000000000537215, -1.996089927833914146 ) ) ;
#11090 = DIRECTION ( 'NONE',  ( -1.000000000000000000, -3.054025858079668409E-16, 2.042474015755241579E-16 ) ) ;
#11092 = CARTESIAN_POINT ( 'NONE',  ( -60.84484350713348277, -2.449279924104672101, -0.9721809163073110716 ) ) ;
#11094 = CARTESIAN_POINT ( 'NONE',  ( 51.70000000000000995, 4.174380580618773706, -1.932497546739578631 ) ) ;
#11093 = CARTESIAN_POINT ( 'NONE',  ( 58.65000000000000568, 1.022750809562428476, -1.571497941946047083 ) ) ;
#11095 = ORIENTED_EDGE ( 'NONE', *, *, #15831, .T. ) ;
#11096 = CARTESIAN_POINT ( 'NONE',  ( -62.06406286214753010, -2.657709275935192128, -0.3428149037536382671 ) ) ;
#11097 = CARTESIAN_POINT ( 'NONE',  ( -59.92928932188130631, 2.138123341857387114E-15, 5.538933845919563674E-16 ) ) ;
#11099 = CARTESIAN_POINT ( 'NONE',  ( -59.19999999999997442, 4.156921938165309527, 1.250136525132554910 ) ) ;
#11098 = PLANE ( 'NONE',  #16530 ) ;
#11100 = DIRECTION ( 'NONE',  ( -1.000000000000000000, -0.000000000000000000, 3.491481338843133355E-15 ) ) ;
#11101 = ORIENTED_EDGE ( 'NONE', *, *, #27242, .F. ) ;
#11102 = CARTESIAN_POINT ( 'NONE',  ( 52.72267294271967586, 4.003822062839298646, 2.049999999999815969 ) ) ;
#11103 = DIRECTION ( 'NONE',  ( -1.520093157366893960E-16, 0.5877852522924802425, -0.8090169943749422332 ) ) ;
#11104 = VERTEX_POINT ( 'NONE', #21140 ) ;
#11105 = DIRECTION ( 'NONE',  ( 0.000000000000000000, 0.000000000000000000, -1.000000000000000000 ) ) ;
#11106 = EDGE_LOOP ( 'NONE', ( #30910, #15513, #11930, #30456 ) ) ;
#11107 = CARTESIAN_POINT ( 'NONE',  ( -59.19999999999997442, -3.382957286162487698, 0.3399999999999019917 ) ) ;
#11108 = CARTESIAN_POINT ( 'NONE',  ( 47.27480557050417076, -4.265347051556910962, -1.724604836179407075 ) ) ;
#11109 = EDGE_LOOP ( 'NONE', ( #20716, #11743, #26902, #16823, #4969 ) ) ;
#11110 =( NAMED_UNIT ( * ) SI_UNIT ( $, .STERADIAN. ) SOLID_ANGLE_UNIT ( ) );
#11111 = CARTESIAN_POINT ( 'NONE',  ( -55.44702994616206126, -2.078460969082661869, 3.599999999999792255 ) ) ;
#11112 = AXIS2_PLACEMENT_3D ( 'NONE', #29403, #31321, #7715 ) ;
#11113 = ADVANCED_FACE ( 'NONE', ( #4318 ), #28781, .T. ) ;
#11114 = CARTESIAN_POINT ( 'NONE',  ( -59.64405989232410832, -2.944486372867076263, -1.700000000000222222 ) ) ;
#11115 = CIRCLE ( 'NONE', #28825, 0.05000000000000143219 ) ;
#11116 = VERTEX_POINT ( 'NONE', #57 ) ;
#11117 = CARTESIAN_POINT ( 'NONE',  ( 36.55000000000001847, 0.000000000000000000, 0.000000000000000000 ) ) ;
#11118 = ORIENTED_EDGE ( 'NONE', *, *, #28274, .T. ) ;
#11119 = VERTEX_POINT ( 'NONE', #1957 ) ;
#11120 = AXIS2_PLACEMENT_3D ( 'NONE', #17633, #22706, #17936 ) ;
#11121 = CARTESIAN_POINT ( 'NONE',  ( -55.62499999999998579, -3.920666489018346722E-15, 3.399999999999801403 ) ) ;
#11122 = FACE_OUTER_BOUND ( 'NONE', #104, .T. ) ;
#11123 = CARTESIAN_POINT ( 'NONE',  ( 58.65000000000000568, 1.671477153794444392, 0.8495817349409554575 ) ) ;
#11124 = CARTESIAN_POINT ( 'NONE',  ( 56.99150396717417522, -0.7610778266783598811, -1.740907964752457904 ) ) ;
#11125 = ADVANCED_FACE ( 'NONE', ( #21300 ), #31303, .T. ) ;
#11126 = AXIS2_PLACEMENT_3D ( 'NONE', #6718, #1799, #11298 ) ;
#11128 = FACE_OUTER_BOUND ( 'NONE', #2882, .T. ) ;
#11127 = CARTESIAN_POINT ( 'NONE',  ( 58.75000000000003553, -1.470078920827915470, 1.470078920827824209 ) ) ;
#11129 = DIRECTION ( 'NONE',  ( 0.000000000000000000, -0.000000000000000000, -1.000000000000000000 ) ) ;
#11130 = CARTESIAN_POINT ( 'NONE',  ( -59.66583922906154669, 2.374710448338345437, -1.229169263546862734 ) ) ;
#11131 = CARTESIAN_POINT ( 'NONE',  ( -55.77900635094609072, -1.737685414808515016, 3.471684241605562438 ) ) ;
#11132 = CARTESIAN_POINT ( 'NONE',  ( 53.91566439300397917, 6.672259399342800990, 1.839335743490167818 ) ) ;
#11133 = CARTESIAN_POINT ( 'NONE',  ( -54.54999999999998295, 3.780972210569126836E-15, -5.448124817252668230E-16 ) ) ;
#11134 = ORIENTED_EDGE ( 'NONE', *, *, #19319, .F. ) ;
#11135 = CARTESIAN_POINT ( 'NONE',  ( -54.49999999999997158, -3.430639028629426601, -0.8101486624347474796 ) ) ;
#11136 = EDGE_CURVE ( 'NONE', #7227, #11119, #3994, .T. ) ;
#11137 = CARTESIAN_POINT ( 'NONE',  ( -36.00201293083839005, -1.123735532908842760, -5.289358697221507200 ) ) ;
#11138 = AXIS2_PLACEMENT_3D ( 'NONE', #3423, #30312, #13351 ) ;
#11139 = ORIENTED_EDGE ( 'NONE', *, *, #18178, .T. ) ;
#11140 = SPHERICAL_SURFACE ( 'NONE', #22005, 0.05000000000000000278 ) ;
#11141 = DIRECTION ( 'NONE',  ( 3.002035892788117952E-16, -0.9996898646859344595, -0.02490330187381124480 ) ) ;
#11143 = DIRECTION ( 'NONE',  ( 0.000000000000000000, -0.9996898646859343485, -0.02490330187381123786 ) ) ;
#11142 = CARTESIAN_POINT ( 'NONE',  ( -57.06249999999997868, -1.962990915244731793, 3.399999999999788969 ) ) ;
#11144 = ORIENTED_EDGE ( 'NONE', *, *, #2726, .T. ) ;
#11145 = ORIENTED_EDGE ( 'NONE', *, *, #27012, .T. ) ;
#11146 = DIRECTION ( 'NONE',  ( 1.000000000000000000, -0.000000000000000000, -1.047444401652940007E-14 ) ) ;
#11147 = ORIENTED_EDGE ( 'NONE', *, *, #8086, .T. ) ;
#11148 = DIRECTION ( 'NONE',  ( 3.491481338843133355E-15, 3.491481338843133355E-15, -1.000000000000000000 ) ) ;
#11149 = EDGE_CURVE ( 'NONE', #4925, #19375, #21727, .T. ) ;
#11150 = CARTESIAN_POINT ( 'NONE',  ( 51.25000000000001421, 1.100000000000537215, -1.996089927833914146 ) ) ;
#11151 = EDGE_LOOP ( 'NONE', ( #17018, #12548 ) ) ;
#11152 = CARTESIAN_POINT ( 'NONE',  ( 25.06719628360101737, 5.330953183167694398, -2.050000000000087752 ) ) ;
#11153 = ADVANCED_FACE ( 'NONE', ( #24732 ), #5727, .T. ) ;
#11154 =( BOUNDED_SURFACE ( )  B_SPLINE_SURFACE ( 3, 2, ( 
 ( #5605, #27289, #30279 ),
 ( #20190, #8589, #6076 ),
 ( #13179, #13032, #8730 ),
 ( #22544, #30113, #1152 ),
 ( #22865, #15727, #25224 ),
 ( #20488, #25055, #12860 ) ),
 .UNSPECIFIED., .F., .F., .F. ) 
 B_SPLINE_SURFACE_WITH_KNOTS ( ( 4, 2, 4 ),
 ( 3, 3 ),
 ( 7.318364664277154930E-19, 0.0002091250881941232294, 0.0004182501763882457541 ),
 ( 0.000000000000000000, 1.000000000000000000 ),
 .UNSPECIFIED. ) 
 GEOMETRIC_REPRESENTATION_ITEM ( )  RATIONAL_B_SPLINE_SURFACE ( (
 ( 1.000000000000000000, 0.8366600265340756737, 1.000000000000000000),
 ( 1.000000000000000000, 0.8366252886216574147, 1.000000000000000000),
 ( 1.000000000000000000, 0.8275698663185694359, 1.000000000000000000),
 ( 1.000000000000000000, 0.7855086314082263543, 1.000000000000000000),
 ( 1.000000000000000000, 0.7518972359451066012, 1.000000000000000000),
 ( 1.000000000000000000, 0.7071067811865354713, 1.000000000000000000) ) ) 
 REPRESENTATION_ITEM ( '' )  SURFACE ( )  );
#11155 = CARTESIAN_POINT ( 'NONE',  ( -59.41132486540516311, 4.156921938165309527, 1.250136525132554244 ) ) ;
#11156 = EDGE_CURVE ( 'NONE', #3746, #4182, #13876, .T. ) ;
#11157 = CARTESIAN_POINT ( 'NONE',  ( 58.75000000000002132, 6.153735859711025284E-13, 3.111507638930570854E-58 ) ) ;
#11158 = ORIENTED_EDGE ( 'NONE', *, *, #28082, .T. ) ;
#11159 = DIRECTION ( 'NONE',  ( 1.027984282060330001E-14, 0.000000000000000000, 1.000000000000000000 ) ) ;
#11160 = CARTESIAN_POINT ( 'NONE',  ( 69.20000000000001705, 0.7500000000000000000, -1.988246715074081017 ) ) ;
#11161 = CARTESIAN_POINT ( 'NONE',  ( 50.80000000000001137, -4.291790910095608425, -1.352971095042658778 ) ) ;
#11162 = CARTESIAN_POINT ( 'NONE',  ( 47.02938631638114941, -3.672971185000220906, 1.825899123715450934 ) ) ;
#11163 = DIRECTION ( 'NONE',  ( 1.000000000000000000, 3.054025858079668409E-16, -2.042474015755241579E-16 ) ) ;
#11164 = VECTOR ( 'NONE', #12855, 1000.000000000000000 ) ;
#11165 = EDGE_CURVE ( 'NONE', #19028, #23041, #9607, .T. ) ;
#11166 = DIRECTION ( 'NONE',  ( -1.000000000000000000, 1.219044193948983948E-29, -3.491481338843133355E-15 ) ) ;
#11167 = CARTESIAN_POINT ( 'NONE',  ( 54.06654434747343885, 5.714581503706766874, -2.050000000000188116 ) ) ;
#11169 = CARTESIAN_POINT ( 'NONE',  ( -44.59999999999996589, -1.399999999999979039, -3.959797974644846619 ) ) ;
#11168 = CARTESIAN_POINT ( 'NONE',  ( 51.70000000000003837, 2.428612866367529932E-14, 4.199999999999812772 ) ) ;
#11170 = CARTESIAN_POINT ( 'NONE',  ( -59.46662241479518229, -2.211912709635374785, 1.464285061855378656 ) ) ;
#11171 = DIRECTION ( 'NONE',  ( -2.117927888850090838E-16, 0.02490330187381123786, -0.9996898646859343485 ) ) ;
#11172 = CARTESIAN_POINT ( 'NONE',  ( 51.25000000000002842, -0.6499999999994634514, 1.489337100860647967 ) ) ;
#11173 = EDGE_LOOP ( 'NONE', ( #9548, #1025 ) ) ;
#11174 = ADVANCED_FACE ( 'NONE', ( #17451 ), #19987, .T. ) ;
#11175 = AXIS2_PLACEMENT_3D ( 'NONE', #15308, #2971, #20082 ) ;
#11176 = CARTESIAN_POINT ( 'NONE',  ( -59.12499999999997158, 2.489203624310598162, -2.804704140674910473 ) ) ;
#11177 = ORIENTED_EDGE ( 'NONE', *, *, #9940, .F. ) ;
#11178 = B_SPLINE_CURVE_WITH_KNOTS ( 'NONE', 3,
 ( #16408, #11668, #7078, #19423, #26383, #29069 ),
 .UNSPECIFIED., .F., .F.,
 ( 4, 2, 4 ),
 ( 0.000000000000000000, 0.0001966045864160461917, 0.0003932091728320923833 ),
 .UNSPECIFIED. ) ;
#11179 = CARTESIAN_POINT ( 'NONE',  ( 52.06628335902944826, 0.5434431642986583544, 1.718465885608440491 ) ) ;
#11180 = VERTEX_POINT ( 'NONE', #2731 ) ;
#11181 = EDGE_CURVE ( 'NONE', #2793, #207, #29628, .T. ) ;
#11182 = CARTESIAN_POINT ( 'NONE',  ( 53.25508263676794485, 8.249290793645352338, 2.049999999999814193 ) ) ;
#11183 = CARTESIAN_POINT ( 'NONE',  ( -56.72085481156723574, -3.673546848079175753, -0.7533615035078068400 ) ) ;
#11185 = CARTESIAN_POINT ( 'NONE',  ( -36.89250464418361020, 2.917650619476140239, 4.554978966839756005 ) ) ;
#11184 = LINE ( 'NONE', #15638, #13494 ) ;
#11186 = ORIENTED_EDGE ( 'NONE', *, *, #26083, .F. ) ;
#11187 = CARTESIAN_POINT ( 'NONE',  ( 28.66498512588421477, 5.839168430874288163, -2.050000000000100631 ) ) ;
#11188 = DIRECTION ( 'NONE',  ( 0.000000000000000000, 0.2008964009354147484, -0.9796124928211139560 ) ) ;
#11189 =( BOUNDED_CURVE ( )  B_SPLINE_CURVE ( 3, ( #2335, #12002, #21832, #5314 ),
 .UNSPECIFIED., .F., .T. ) 
 B_SPLINE_CURVE_WITH_KNOTS ( ( 4, 4 ),
 ( 0.9419121880553512627, 1.065287454991164173 ),
 .UNSPECIFIED. ) 
 CURVE ( )  GEOMETRIC_REPRESENTATION_ITEM ( )  RATIONAL_B_SPLINE_CURVE ( ( 1.000000000000000000, 0.9987319474856933832, 0.9987319474856933832, 1.000000000000000000 ) ) 
 REPRESENTATION_ITEM ( '' )  );
#11190 = VERTEX_POINT ( 'NONE', #7954 ) ;
#11192 = CARTESIAN_POINT ( 'NONE',  ( -67.92156587216960872, 1.648633347906700797, 0.04106915093618024315 ) ) ;
#11191 = FACE_OUTER_BOUND ( 'NONE', #16584, .T. ) ;
#11193 = CARTESIAN_POINT ( 'NONE',  ( -56.33155989232412963, 3.400000000000008349, -1.856946929144785632E-13 ) ) ;
#11194 = ADVANCED_FACE ( 'NONE', ( #24877 ), #7558, .T. ) ;
#11195 = ORIENTED_EDGE ( 'NONE', *, *, #17439, .F. ) ;
#11196 = CARTESIAN_POINT ( 'NONE',  ( 36.50000000000002132, -0.7794871794871797155, -1.732743413496390161 ) ) ;
#11197 = ADVANCED_FACE ( 'NONE', ( #22224 ), #17159, .T. ) ;
#11198 = CARTESIAN_POINT ( 'NONE',  ( 58.65838214097839654, 1.802220213626245515, -0.5175938701871466430 ) ) ;
#11199 = SURFACE_SIDE_STYLE ('',( #11050 ) ) ;
#11200 = DIRECTION ( 'NONE',  ( 0.000000000000000000, -1.000000000000000000, -3.491481338843132961E-15 ) ) ;
#11201 = CARTESIAN_POINT ( 'NONE',  ( -58.25952994616203284, -3.117691453623963938, -1.800000000000218092 ) ) ;
#11202 = B_SPLINE_CURVE_WITH_KNOTS ( 'NONE', 3,
 ( #28795, #14212, #4708, #31315, #4871, #23888, #26736, #28940, #9651, #9491, #19305, #9941, #16616, #2178, #7107, #28474, #132, #12010, #21692 ),
 .UNSPECIFIED., .F., .F.,
 ( 4, 3, 3, 3, 3, 3, 4 ),
 ( -1.463115107851837610E-06, -2.117582368135750848E-22, 2.244303852771090691E-05, 4.060544239443321531E-05, 5.609829020924228863E-05, 7.063629490958457896E-05, 8.524507318609980048E-05 ),
 .UNSPECIFIED. ) ;
#11203 = VECTOR ( 'NONE', #8311, 1000.000000000000000 ) ;
#11204 = DIRECTION ( 'NONE',  ( 1.000000000000000000, 1.047444401652940007E-14, -0.000000000000000000 ) ) ;
#11205 = CARTESIAN_POINT ( 'NONE',  ( -57.29792740578360366, 3.330682475591789427, 0.6830477631804139360 ) ) ;
#11206 = CARTESIAN_POINT ( 'NONE',  ( -55.89405989232412253, -2.944486372867073598, -1.700000000000213563 ) ) ;
#11207 = EDGE_CURVE ( 'NONE', #17943, #23827, #23746, .T. ) ;
#11208 = CARTESIAN_POINT ( 'NONE',  ( 58.45000000000001705, 0.7794871794871796045, 1.732743413496389939 ) ) ;
#11209 = CARTESIAN_POINT ( 'NONE',  ( 53.32659978131828638, 4.996751601655196495, 1.614826230506383409 ) ) ;
#11210 = LINE ( 'NONE', #21371, #24156 ) ;
#11211 = ADVANCED_FACE ( 'NONE', ( #12376 ), #30807, .F. ) ;
#11212 = ORIENTED_EDGE ( 'NONE', *, *, #12849, .T. ) ;
#11213 = CARTESIAN_POINT ( 'NONE',  ( 58.75000000000000711, 1.655311165516932803, 1.077297519405395310 ) ) ;
#11214 = ORIENTED_EDGE ( 'NONE', *, *, #2212, .T. ) ;
#11215 = CARTESIAN_POINT ( 'NONE',  ( -57.72499999999997300, 2.811319000628834039E-15, 1.036730182770210180E-16 ) ) ;
#11216 = CARTESIAN_POINT ( 'NONE',  ( 48.50000000000002132, 1.409901620910219311, 3.850000000000021849 ) ) ;
#11217 = ORIENTED_EDGE ( 'NONE', *, *, #21967, .F. ) ;
#11218 = FACE_OUTER_BOUND ( 'NONE', #8917, .T. ) ;
#11219 = CIRCLE ( 'NONE', #6172, 2.525000000001611511 ) ;
#11220 = CARTESIAN_POINT ( 'NONE',  ( -62.04999999999998295, 1.183285843523195887E-15, 2.187514201909070562E-15 ) ) ;
#11222 = CARTESIAN_POINT ( 'NONE',  ( -67.88621053311027254, -5.990042905486032463E-16, 3.379566295451473069E-15 ) ) ;
#11221 = CARTESIAN_POINT ( 'NONE',  ( -60.32202994616201863, 2.078460969082674747, -3.600000000000205258 ) ) ;
#11223 = VERTEX_POINT ( 'NONE', #22517 ) ;
#11224 = CARTESIAN_POINT ( 'NONE',  ( -58.98542740578360366, 0.7887156198831661857, -3.845940847736173840 ) ) ;
#11225 = CARTESIAN_POINT ( 'NONE',  ( 58.50000000000001421, 0.000000000000000000, 0.000000000000000000 ) ) ;
#11226 = SHAPE_DEFINITION_REPRESENTATION ( #12578, #9258 ) ;
#11227 = DIRECTION ( 'NONE',  ( 1.047444401652940007E-14, 0.000000000000000000, 1.000000000000000000 ) ) ;
#11228 = DIRECTION ( 'NONE',  ( 3.491481338843133355E-15, 3.491481338843133355E-15, -1.000000000000000000 ) ) ;
#11229 = CARTESIAN_POINT ( 'NONE',  ( -54.48118151432741030, 1.510613940323803916, -4.037256667234632168 ) ) ;
#11230 = VERTEX_POINT ( 'NONE', #820 ) ;
#11231 = CARTESIAN_POINT ( 'NONE',  ( -71.49999999999998579, -1.395601618875910821E-15, 2.917180974979867506E-15 ) ) ;
#11232 = CARTESIAN_POINT ( 'NONE',  ( -36.31414349454749413, 3.010474646410376653, -4.240315621469644469 ) ) ;
#11233 = CARTESIAN_POINT ( 'NONE',  ( 51.21569492700660930, 0.9844681138065065618, 1.555342057744142581 ) ) ;
#11234 = SPHERICAL_SURFACE ( 'NONE', #16475, 0.1000000000000000056 ) ;
#11235 = CARTESIAN_POINT ( 'NONE',  ( -73.89999999999997726, -2.435524336289708093E-15, 4.607889071584891164E-15 ) ) ;
#11237 = CARTESIAN_POINT ( 'NONE',  ( -54.68749999999997868, 0.7533615035078081723, -3.673546848079177973 ) ) ;
#11236 = DIRECTION ( 'NONE',  ( 1.000000000000000000, 1.047444401652940007E-14, 0.000000000000000000 ) ) ;
#11238 = DIRECTION ( 'NONE',  ( 1.000000000000000000, 3.054025858079668409E-16, -2.042474015755241579E-16 ) ) ;
#11240 = CARTESIAN_POINT ( 'NONE',  ( 61.00000000000003553, -0.8111533433287256845, 1.409596402460999487 ) ) ;
#11239 = CARTESIAN_POINT ( 'NONE',  ( -44.59999999999998721, -1.400000000000006795, 3.959797974644484242 ) ) ;
#11241 = ADVANCED_FACE ( 'NONE', ( #10488 ), #20163, .F. ) ;
#11242 = ORIENTED_EDGE ( 'NONE', *, *, #19388, .T. ) ;
#11243 = CARTESIAN_POINT ( 'NONE',  ( -62.06727109562227440, -2.629110561070149288, -0.3274874463776150102 ) ) ;
#11244 = EDGE_CURVE ( 'NONE', #25393, #27342, #1991, .T. ) ;
#11245 = PLANE ( 'NONE',  #6503 ) ;
#11246 = TOROIDAL_SURFACE ( 'NONE', #28960, 4.650000000000000355, 0.05000000000000000278 ) ;
#11248 = CARTESIAN_POINT ( 'NONE',  ( 58.65000000000004121, -1.834410884275050169, 0.3880228184668811364 ) ) ;
#11247 = CARTESIAN_POINT ( 'NONE',  ( 58.75000018803716273, 1.857237022264430326, 0.5488434064270322210 ) ) ;
#11249 = CARTESIAN_POINT ( 'NONE',  ( 15.39414421509789754, -5.035245099686910031, 1.330662535294788951 ) ) ;
#11250 = EDGE_LOOP ( 'NONE', ( #8124, #282, #19422, #18354 ) ) ;
#11251 = CARTESIAN_POINT ( 'NONE',  ( 52.02306152107794901, 3.830941655646745936, 2.049999999999818190 ) ) ;
#11252 = LINE ( 'NONE', #3815, #4224 ) ;
#11253 = VERTEX_POINT ( 'NONE', #25354 ) ;
#11254 = DIRECTION ( 'NONE',  ( -1.000000000000000000, 1.219044193948983948E-29, -3.491481338843133355E-15 ) ) ;
#11255 = ORIENTED_EDGE ( 'NONE', *, *, #5257, .F. ) ;
#11256 = CARTESIAN_POINT ( 'NONE',  ( -56.72499999999997300, 0.9241234443029111567, -4.506217466977124886 ) ) ;
#11257 = ORIENTED_EDGE ( 'NONE', *, *, #23836, .F. ) ;
#11258 =( NAMED_UNIT ( * ) SI_UNIT ( $, .STERADIAN. ) SOLID_ANGLE_UNIT ( ) );
#11259 = CARTESIAN_POINT ( 'NONE',  ( 54.40000000000001990, 0.000000000000000000, -3.200000000000000178 ) ) ;
#11260 = EDGE_CURVE ( 'NONE', #10453, #23943, #27279, .T. ) ;
#11261 = CARTESIAN_POINT ( 'NONE',  ( -57.70655989232413674, 1.962990915244722245, 3.399999999999802291 ) ) ;
#11262 = VERTEX_POINT ( 'NONE', #11248 ) ;
#11263 = VERTEX_POINT ( 'NONE', #13157 ) ;
#11264 = ORIENTED_EDGE ( 'NONE', *, *, #22994, .T. ) ;
#11265 = CARTESIAN_POINT ( 'NONE',  ( -55.87499999999996447, 2.944486372867106905, -1.700000000000186029 ) ) ;
#11266 = CARTESIAN_POINT ( 'NONE',  ( 52.13000000000001677, 0.5000000000005460077, -1.718465885608440269 ) ) ;
#11267 = CARTESIAN_POINT ( 'NONE',  ( -59.69999999999998153, 2.914965204491517081, 1.750136525132549137 ) ) ;
#11268 = CIRCLE ( 'NONE', #1657, 1.975000000000001865 ) ;
#11269 = CARTESIAN_POINT ( 'NONE',  ( 60.75000000000002842, -0.7499999999993639532, 1.718465885608440047 ) ) ;
#11270 = DIRECTION ( 'NONE',  ( 1.000000000000000000, -1.219044193948983948E-29, 3.491481338843133355E-15 ) ) ;
#11272 = FACE_OUTER_BOUND ( 'NONE', #14587, .T. ) ;
#11271 = CARTESIAN_POINT ( 'NONE',  ( -36.00201293083839715, 4.683225679163155242, -2.703237727951674607 ) ) ;
#11273 = FACE_OUTER_BOUND ( 'NONE', #28250, .T. ) ;
#11274 = DIRECTION ( 'NONE',  ( -1.000000000000000000, 1.219044193948983948E-29, -3.491481338843133355E-15 ) ) ;
#11275 = DIRECTION ( 'NONE',  ( 0.000000000000000000, 0.000000000000000000, 1.000000000000000000 ) ) ;
#11276 = EDGE_CURVE ( 'NONE', #9817, #3419, #19708, .T. ) ;
#11277 = CARTESIAN_POINT ( 'NONE',  ( 56.98109951608436319, 0.7885528131279547770, 2.477553856021609491 ) ) ;
#11278 = CARTESIAN_POINT ( 'NONE',  ( -59.35358983848620795, 2.308634493194285486, 1.301040651491357503 ) ) ;
#11279 = DIRECTION ( 'NONE',  ( 0.000000000000000000, 0.9996898646859345705, 0.02490330187381124133 ) ) ;
#11280 = ORIENTED_EDGE ( 'NONE', *, *, #19388, .F. ) ;
#11282 = FACE_OUTER_BOUND ( 'NONE', #2262, .T. ) ;
#11281 = CARTESIAN_POINT ( 'NONE',  ( 58.45000000000001705, 0.000000000000000000, 0.000000000000000000 ) ) ;
#11283 = CARTESIAN_POINT ( 'NONE',  ( 65.05000000000001137, -1.025519176787267142E-28, -6.813625832752373386E-13 ) ) ;
#11284 = ORIENTED_EDGE ( 'NONE', *, *, #8089, .F. ) ;
#11285 = CIRCLE ( 'NONE', #12798, 0.05000000000000010686 ) ;
#11286 = DIRECTION ( 'NONE',  ( 1.000000000000000000, 1.047444401652940007E-14, 0.000000000000000000 ) ) ;
#11287 = CARTESIAN_POINT ( 'NONE',  ( -58.87499999999996447, 2.944486372867106905, -1.700000000000196465 ) ) ;
#11288 = ORIENTED_EDGE ( 'NONE', *, *, #16689, .F. ) ;
#11289 = AXIS2_PLACEMENT_3D ( 'NONE', #7951, #17616, #22515 ) ;
#11290 = ORIENTED_EDGE ( 'NONE', *, *, #18963, .F. ) ;
#11291 = DIRECTION ( 'NONE',  ( -1.000000000000000000, -1.047444401652940007E-14, -0.000000000000000000 ) ) ;
#11292 = ORIENTED_EDGE ( 'NONE', *, *, #17433, .T. ) ;
#11293 = CARTESIAN_POINT ( 'NONE',  ( 58.65000000000001990, 6.143261415694495821E-13, 3.111507638930570854E-58 ) ) ;
#11294 = FACE_OUTER_BOUND ( 'NONE', #30994, .T. ) ;
#11295 = EDGE_LOOP ( 'NONE', ( #6014, #2597, #11666, #27365 ) ) ;
#11296 = CARTESIAN_POINT ( 'NONE',  ( 25.08803375997270990, 5.428914793826271179, -2.050000000000086864 ) ) ;
#11297 = CARTESIAN_POINT ( 'NONE',  ( 57.05000000000001847, -0.7794871794871796045, -1.732743413496389939 ) ) ;
#11298 = DIRECTION ( 'NONE',  ( 3.002035892788116966E-16, -0.9996898646859343485, -0.02490330187381123786 ) ) ;
#11299 = EDGE_LOOP ( 'NONE', ( #15687, #11597, #1208, #4161 ) ) ;
#11300 = ORIENTED_EDGE ( 'NONE', *, *, #6050, .F. ) ;
#11301 = CARTESIAN_POINT ( 'NONE',  ( -73.84999999999996589, -2.420255095024673698E-15, 4.597676519392165349E-15 ) ) ;
#11302 = CARTESIAN_POINT ( 'NONE',  ( -55.56249999999999289, -1.962990915244736234, 3.399999999999792522 ) ) ;
#11303 = CARTESIAN_POINT ( 'NONE',  ( 61.25000000000000000, 0.8716090598197026029, -1.626546686965558264 ) ) ;
#11304 = EDGE_CURVE ( 'NONE', #15189, #29731, #26267, .T. ) ;
#11305 = PLANE ( 'NONE',  #6851 ) ;
#11306 = CARTESIAN_POINT ( 'NONE',  ( 58.74154451056414672, 1.258335925860078364, 1.390058629629135956 ) ) ;
#11307 = DIRECTION ( 'NONE',  ( 0.000000000000000000, -0.2008964009354147484, 0.9796124928211139560 ) ) ;
#11308 = CARTESIAN_POINT ( 'NONE',  ( 57.00108727371435435, 0.7119914823645937529, -1.810661949215600863 ) ) ;
#11310 = DIRECTION ( 'NONE',  ( -1.000000000000000000, -0.000000000000000000, 0.000000000000000000 ) ) ;
#11309 = CARTESIAN_POINT ( 'NONE',  ( -36.56242893520548165, -3.003531019938339597, 4.498666779076304856 ) ) ;
#11311 = DIRECTION ( 'NONE',  ( 3.489354422748178582E-15, -1.218509414717996338E-16, 1.000000000000000000 ) ) ;
#11312 = FACE_OUTER_BOUND ( 'NONE', #5685, .T. ) ;
#11313 = ADVANCED_FACE ( 'NONE', ( #25027 ), #17172, .T. ) ;
#11314 = CARTESIAN_POINT ( 'NONE',  ( 50.28942560560668795, 8.224494709121804803, -2.050000000000174794 ) ) ;
#11315 = CARTESIAN_POINT ( 'NONE',  ( 48.30000000000001847, -0.6462379109120514054, -4.048750000000023164 ) ) ;
#11316 = EDGE_CURVE ( 'NONE', #14207, #4452, #14638, .T. ) ;
#11317 = ORIENTED_EDGE ( 'NONE', *, *, #7724, .F. ) ;
#11318 = EDGE_CURVE ( 'NONE', #17824, #21074, #23331, .T. ) ;
#11319 = AXIS2_PLACEMENT_3D ( 'NONE', #26731, #4561, #23883 ) ;
#11320 = ORIENTED_EDGE ( 'NONE', *, *, #9051, .F. ) ;
#11321 = CARTESIAN_POINT ( 'NONE',  ( 51.03702166449080835, -3.901511898670509737, 1.261029562208011212 ) ) ;
#11322 = ORIENTED_EDGE ( 'NONE', *, *, #26476, .T. ) ;
#11323 =( BOUNDED_SURFACE ( )  B_SPLINE_SURFACE ( 3, 2, ( 
 ( #13045, #20199, #10526 ),
 ( #24608, #20351, #20502 ),
 ( #27604, #12872, #8140 ),
 ( #22556, #545, #12723 ),
 ( #29830, #17813, #17655 ),
 ( #30128, #10201, #15264 ),
 ( #8289, #3077, #27450 ),
 ( #17958, #24911, #15588 ),
 ( #10350, #5764, #5930 ),
 ( #861, #3552, #3398 ) ),
 .UNSPECIFIED., .F., .F., .T. ) 
 B_SPLINE_SURFACE_WITH_KNOTS ( ( 4, 2, 2, 2, 4 ),
 ( 3, 3 ),
 ( 0.0001706658715691072165, 0.0002229276920778219600, 0.0002751895125865367036, 0.0003274513330952514472, 0.0003797131536039661907 ),
 ( 0.000000000000000000, 1.000000000000000000 ),
 .UNSPECIFIED. ) 
 GEOMETRIC_REPRESENTATION_ITEM ( )  RATIONAL_B_SPLINE_SURFACE ( (
 ( 1.000000000000000000, 0.7071067811865444641, 1.000000000000000000),
 ( 1.000000000000000000, 0.7375607040702822914, 1.000000000000000000),
 ( 1.000000000000000000, 0.7730431127429990834, 1.000000000000000000),
 ( 1.000000000000000000, 0.8321012486994672219, 1.000000000000000000),
 ( 1.000000000000000000, 0.8541932017419723300, 1.000000000000000000),
 ( 1.000000000000000000, 0.8545723906072110188, 1.000000000000000000),
 ( 1.000000000000000000, 0.8327032135058637374, 1.000000000000000000),
 ( 1.000000000000000000, 0.7734559727065434265, 1.000000000000000000),
 ( 1.000000000000000000, 0.7377766653997924751, 1.000000000000000000),
 ( 1.000000000000000000, 0.7071067811865456854, 1.000000000000000000) ) ) 
 REPRESENTATION_ITEM ( '' )  SURFACE ( )  );
#11324 = CARTESIAN_POINT ( 'NONE',  ( 52.98658227084826677, 8.418175601153722099, 2.049999999999815081 ) ) ;
#11325 = CARTESIAN_POINT ( 'NONE',  ( -56.59585481156723574, -1.184343223768586251, -3.558065644182725862 ) ) ;
#11327 = CARTESIAN_POINT ( 'NONE',  ( -36.77443515226919857, 2.672993279333530925, 4.702725322014869924 ) ) ;
#11326 = CARTESIAN_POINT ( 'NONE',  ( 60.75000000000002842, -0.4999999999993606226, 1.554802467931481802 ) ) ;
#11328 = ORIENTED_EDGE ( 'NONE', *, *, #23721, .F. ) ;
#11329 = ORIENTED_EDGE ( 'NONE', *, *, #1937, .T. ) ;
#11330 = DIRECTION ( 'NONE',  ( -1.000000000000000000, -3.053848253006669023E-16, 2.042510438544995415E-16 ) ) ;
#11331 = ORIENTED_EDGE ( 'NONE', *, *, #15801, .F. ) ;
#11332 = CIRCLE ( 'NONE', #26511, 2.650000000000000799 ) ;
#11333 = DIRECTION ( 'NONE',  ( 0.000000000000000000, 1.000000000000000000, 3.491481338843130594E-15 ) ) ;
#11334 = ADVANCED_FACE ( 'NONE', ( #15846 ), #27563, .F. ) ;
#11335 = ORIENTED_EDGE ( 'NONE', *, *, #29349, .F. ) ;
#11337 = DIRECTION ( 'NONE',  ( 1.000000000000000000, -1.219044193948983948E-29, 3.491481338843133355E-15 ) ) ;
#11336 = CARTESIAN_POINT ( 'NONE',  ( 51.80000000000001847, -3.726179070414207928, 1.710435481158852244 ) ) ;
#11338 = DIRECTION ( 'NONE',  ( 0.000000000000000000, 0.000000000000000000, 1.000000000000000000 ) ) ;
#11339 = ORIENTED_EDGE ( 'NONE', *, *, #19091, .F. ) ;
#11340 = CIRCLE ( 'NONE', #716, 0.1499999999999999667 ) ;
#11341 = CARTESIAN_POINT ( 'NONE',  ( -36.50489844130380135, 5.024465639092071889, -2.007392901578094691 ) ) ;
#11342 = CARTESIAN_POINT ( 'NONE',  ( 51.25000000000002842, -0.9938153758920951208, -1.589954715908409977 ) ) ;
#11343 = CARTESIAN_POINT ( 'NONE',  ( -54.49999477219272848, -1.549165129012789466, -3.331602747802265174 ) ) ;
#11344 = CARTESIAN_POINT ( 'NONE',  ( 56.95000053796676553, 0.7321038892619347038, 1.754109389045036771 ) ) ;
#11345 = CARTESIAN_POINT ( 'NONE',  ( -59.32202994616204705, 2.078460969082646770, 3.599999999999797140 ) ) ;
#11346 = AXIS2_PLACEMENT_3D ( 'NONE', #31326, #9666, #24223 ) ;
#11347 = ADVANCED_FACE ( 'NONE', ( #3810 ), #23155, .T. ) ;
#11348 = CARTESIAN_POINT ( 'NONE',  ( 51.85600457075751990, 0.1551120032652606173, 4.362278500573884443 ) ) ;
#11349 = DIRECTION ( 'NONE',  ( 0.000000000000000000, 0.000000000000000000, 1.000000000000000000 ) ) ;
#11350 = CARTESIAN_POINT ( 'NONE',  ( 50.41049980741060921, 0.7811435014051845149, -4.027217152858574956 ) ) ;
#11351 = VECTOR ( 'NONE', #29366, 1000.000000000000000 ) ;
#11352 = AXIS2_PLACEMENT_3D ( 'NONE', #8284, #13492, #29972 ) ;
#11353 = FACE_OUTER_BOUND ( 'NONE', #13026, .T. ) ;
#11354 = EDGE_CURVE ( 'NONE', #4199, #3631, #17677, .T. ) ;
#11355 = CARTESIAN_POINT ( 'NONE',  ( 65.00000000000002842, 1.401298464324817071E-42, -6.808388610744111684E-13 ) ) ;
#11356 = EDGE_CURVE ( 'NONE', #11041, #5230, #6346, .T. ) ;
#11357 = AXIS2_PLACEMENT_3D ( 'NONE', #12770, #17859, #27497 ) ;
#11358 = ORIENTED_EDGE ( 'NONE', *, *, #10557, .F. ) ;
#11359 = EDGE_CURVE ( 'NONE', #3896, #12339, #6043, .T. ) ;
#11360 = DIRECTION ( 'NONE',  ( 1.000000000000000000, -0.000000000000000000, -0.000000000000000000 ) ) ;
#11361 = DIRECTION ( 'NONE',  ( -0.9993908270190956511, 0.03489949670250089980, 3.469446951951485842E-15 ) ) ;
#11362 = CARTESIAN_POINT ( 'NONE',  ( 50.50000000000002132, 5.291762632692320630E-13, -1.996089927833914146 ) ) ;
#11363 = CARTESIAN_POINT ( 'NONE',  ( 48.30268563551750560, 0.9333771270347341886, -3.994943142064453667 ) ) ;
#11364 = ORIENTED_EDGE ( 'NONE', *, *, #8014, .F. ) ;
#11365 = CARTESIAN_POINT ( 'NONE',  ( -57.27900635094609072, 3.400000000000004352, 0.9110272542656309147 ) ) ;
#11366 = ORIENTED_EDGE ( 'NONE', *, *, #5908, .T. ) ;
#11367 = CIRCLE ( 'NONE', #29080, 0.1500000000000001887 ) ;
#11368 = FILL_AREA_STYLE ('',( #4567 ) ) ;
#11369 = CARTESIAN_POINT ( 'NONE',  ( 69.20000000000000284, 4.557543281186736018E-17, -2.729289321882063302 ) ) ;
#11370 = PRODUCT ( 'Body', 'Body', '', ( #5555 ) ) ;
#11371 = ORIENTED_EDGE ( 'NONE', *, *, #3615, .F. ) ;
#11372 = EDGE_LOOP ( 'NONE', ( #17825, #17964, #24614, #13431 ) ) ;
#11373 = CARTESIAN_POINT ( 'NONE',  ( 53.91582462592152325, 6.672259099522118930, 0.8960135317204955818 ) ) ;
#11374 = CARTESIAN_POINT ( 'NONE',  ( 58.64999999999992042, -1.320082690054604546, 1.469015551795364916 ) ) ;
#11376 = DIRECTION ( 'NONE',  ( -0.000000000000000000, 0.000000000000000000, 1.000000000000000000 ) ) ;
#11375 = CARTESIAN_POINT ( 'NONE',  ( -60.44702994616202574, -2.078460969082631227, -3.600000000000220801 ) ) ;
#11377 = EDGE_LOOP ( 'NONE', ( #16266, #19178, #16739, #19123, #11425 ) ) ;
#11378 = CARTESIAN_POINT ( 'NONE',  ( -54.87499999999997868, -3.673546848079173532, -0.7533615035078067290 ) ) ;
#11379 = AXIS2_PLACEMENT_3D ( 'NONE', #9031, #30882, #9200 ) ;
#11380 = CARTESIAN_POINT ( 'NONE',  ( -36.14490256869204643, 2.228039998204367933, 4.927410888447855797 ) ) ;
#11381 = CONTEXT_DEPENDENT_SHAPE_REPRESENTATION ( #25775, #9118 ) ;
#11382 = CARTESIAN_POINT ( 'NONE',  ( 58.65000000000002700, -0.5811678240974692544, 1.782657835994643447 ) ) ;
#11383 = CARTESIAN_POINT ( 'NONE',  ( 51.45655683570189609, 0.9591657938401617622, -1.468576096419531352 ) ) ;
#11384 = CIRCLE ( 'NONE', #3302, 0.05000000000000009298 ) ;
#11385 = DIRECTION ( 'NONE',  ( 0.000000000000000000, 0.000000000000000000, -1.000000000000000000 ) ) ;
#11386 = EDGE_CURVE ( 'NONE', #29844, #6742, #2220, .T. ) ;
#11387 = ORIENTED_EDGE ( 'NONE', *, *, #20324, .T. ) ;
#11388 = AXIS2_PLACEMENT_3D ( 'NONE', #12400, #14928, #7520 ) ;
#11389 = CARTESIAN_POINT ( 'NONE',  ( 57.04534525700438508, -0.7498361808180106225, 1.778489416763646025 ) ) ;
#11390 = AXIS2_PLACEMENT_3D ( 'NONE', #30069, #30711, #23432 ) ;
#11391 = ADVANCED_FACE ( 'NONE', ( #21565 ), #3657, .T. ) ;
#11392 = CARTESIAN_POINT ( 'NONE',  ( -36.39645873810205501, 2.743848709681631970, -4.666930520580605979 ) ) ;
#11393 = FACE_OUTER_BOUND ( 'NONE', #26489, .T. ) ;
#11394 = CARTESIAN_POINT ( 'NONE',  ( 52.20711756518984714, -0.7499999999994533262, -1.996089927833914146 ) ) ;
#11395 = CARTESIAN_POINT ( 'NONE',  ( 15.97944027357902108, 0.5584590966806891599, -5.380195666604552507 ) ) ;
#11397 = DIRECTION ( 'NONE',  ( 0.000000000000000000, -7.228014483236697541E-16, -1.000000000000000000 ) ) ;
#11396 = CARTESIAN_POINT ( 'NONE',  ( 51.12687253673781385, -0.9194130538815391551, -1.491219977510798600 ) ) ;
#11398 = ADVANCED_FACE ( 'NONE', ( #11581 ), #19346, .T. ) ;
#11399 = CIRCLE ( 'NONE', #25050, 4.100000000000000533 ) ;
#11400 = CARTESIAN_POINT ( 'NONE',  ( 47.19197484456741876, -4.291220349888532404, -1.660930850246812307 ) ) ;
#11402 = CARTESIAN_POINT ( 'NONE',  ( 50.31565037626138803, -1.386108502191528924, -3.851082811767820413 ) ) ;
#11401 = LINE ( 'NONE', #25966, #2869 ) ;
#11403 = AXIS2_PLACEMENT_3D ( 'NONE', #7029, #16691, #12371 ) ;
#11404 = ORIENTED_EDGE ( 'NONE', *, *, #21476, .F. ) ;
#11405 = CARTESIAN_POINT ( 'NONE',  ( 51.45655683570189609, 0.9591657938401617622, 1.468576096419531352 ) ) ;
#11406 = DIRECTION ( 'NONE',  ( -1.000000000000000000, -0.000000000000000000, 0.000000000000000000 ) ) ;
#11408 = CARTESIAN_POINT ( 'NONE',  ( -36.58413561666694847, 5.110933801299781365, 1.769007076670967793 ) ) ;
#11407 = CARTESIAN_POINT ( 'NONE',  ( 58.72419296898066676, 1.799118770101964859, 0.5284032650199490533 ) ) ;
#11409 = CARTESIAN_POINT ( 'NONE',  ( 15.49702763512081560, -4.928592478218981832, 1.658905555082623717 ) ) ;
#11410 = B_SPLINE_CURVE_WITH_KNOTS ( 'NONE', 3,
 ( #43, #31234, #19676, #24715, #5096, #16833, #14746, #26471, #19515, #5402, #29315, #9706, #343, #26930, #29453, #22206, #4772, #24406, #7627 ),
 .UNSPECIFIED., .F., .F.,
 ( 4, 3, 3, 3, 3, 3, 4 ),
 ( -1.485273975135398565E-06, 0.000000000000000000, 2.074191569004160408E-05, 3.882553518188197389E-05, 5.450508821808563542E-05, 6.929665250580404950E-05, 8.415228772525318584E-05 ),
 .UNSPECIFIED. ) ;
#11411 = AXIS2_PLACEMENT_3D ( 'NONE', #18310, #16246, #18631 ) ;
#11412 = EDGE_LOOP ( 'NONE', ( #27053, #10999, #23287, #21102, #23082 ) ) ;
#11413 = VERTEX_POINT ( 'NONE', #25972 ) ;
#11414 = CARTESIAN_POINT ( 'NONE',  ( 48.50000000000002132, 1.426739617975221641, 3.843750000000023093 ) ) ;
#11415 = CARTESIAN_POINT ( 'NONE',  ( 50.38699024846546592, -1.088846059295756286, 3.899771020632008423 ) ) ;
#11416 = AXIS2_PLACEMENT_3D ( 'NONE', #25883, #26204, #4511 ) ;
#11417 = VERTEX_POINT ( 'NONE', #13925 ) ;
#11418 = VECTOR ( 'NONE', #26393, 999.9999999999998863 ) ;
#11419 = DIRECTION ( 'NONE',  ( 1.000000000000000000, 8.626663965456006092E-17, 1.494526870159786164E-16 ) ) ;
#11420 = ORIENTED_EDGE ( 'NONE', *, *, #12981, .T. ) ;
#11421 = CARTESIAN_POINT ( 'NONE',  ( 57.05000000000001847, 0.8000000000000000444, 2.471260002560649927 ) ) ;
#11422 = EDGE_LOOP ( 'NONE', ( #1057, #19618, #12110, #25052, #17207, #4952, #8003, #26995 ) ) ;
#11423 = CARTESIAN_POINT ( 'NONE',  ( -55.50952994616206126, -5.525201388156016014E-15, 3.599999999999801581 ) ) ;
#11424 = CARTESIAN_POINT ( 'NONE',  ( -55.89405989232412253, -2.944486372867076263, -1.700000000000208900 ) ) ;
#11425 = ORIENTED_EDGE ( 'NONE', *, *, #28171, .T. ) ;
#11426 = ORIENTED_EDGE ( 'NONE', *, *, #17729, .F. ) ;
#11427 = ADVANCED_FACE ( 'NONE', ( #23622 ), #21881, .T. ) ;
#11428 = AXIS2_PLACEMENT_3D ( 'NONE', #29621, #10023, #29462 ) ;
#11429 = ORIENTED_EDGE ( 'NONE', *, *, #27672, .T. ) ;
#11430 = ADVANCED_FACE ( 'NONE', ( #12337 ), #29586, .T. ) ;
#11431 = AXIS2_PLACEMENT_3D ( 'NONE', #23324, #13788, #26792 ) ;
#11432 = CARTESIAN_POINT ( 'NONE',  ( -60.68749999999996447, -3.925981830489445379, -2.294491627273766911E-13 ) ) ;
#11433 = EDGE_CURVE ( 'NONE', #28767, #6209, #3507, .T. ) ;
#11434 = CARTESIAN_POINT ( 'NONE',  ( -55.17306624327023457, -3.399999999999988365, -0.9110272542660268202 ) ) ;
#11435 = CARTESIAN_POINT ( 'NONE',  ( 27.10659297677967317, 5.279073180725292858, -1.425000000000094413 ) ) ;
#11436 = DIRECTION ( 'NONE',  ( 0.000000000000000000, 0.000000000000000000, 1.000000000000000000 ) ) ;
#11437 = MECHANICAL_DESIGN_GEOMETRIC_PRESENTATION_REPRESENTATION (  '', ( #7396 ), #7937 ) ;
#11438 = DIRECTION ( 'NONE',  ( 0.000000000000000000, 0.3333333333333287629, 0.9428090415820650216 ) ) ;
#11439 = AXIS2_PLACEMENT_3D ( 'NONE', #22394, #12257, #536 ) ;
#11440 = CIRCLE ( 'NONE', #4362, 2.000000000000000000 ) ;
#11441 = COLOUR_RGB ( '', 0.40784314, 0.44705882, 0.49803922) ;
#11443 = DIRECTION ( 'NONE',  ( 0.000000000000000000, -1.000000000000000000, -3.491481338843132961E-15 ) ) ;
#11442 = CARTESIAN_POINT ( 'NONE',  ( -36.40793637698146767, 5.360541651686750342, -0.7128348320083691680 ) ) ;
#11444 = DIRECTION ( 'NONE',  ( 1.000000000000000000, 3.053848253006669023E-16, -2.042510438544995415E-16 ) ) ;
#11445 = DIRECTION ( 'NONE',  ( -1.000000000000000000, -0.000000000000000000, 3.491481338843133355E-15 ) ) ;
#11446 = CARTESIAN_POINT ( 'NONE',  ( -36.92405921417685732, -3.294441450831190110, -4.290383166762150147 ) ) ;
#11447 = EDGE_CURVE ( 'NONE', #17367, #27461, #27867, .T. ) ;
#11448 = CARTESIAN_POINT ( 'NONE',  ( 58.75000000000003553, -1.655311165516605509, -1.077297519404007087 ) ) ;
#11449 = CARTESIAN_POINT ( 'NONE',  ( -59.59999999999998721, 2.022492213459062160, 1.712315755489264513 ) ) ;
#11450 = AXIS2_PLACEMENT_3D ( 'NONE', #15415, #13187, #1160 ) ;
#11451 = CARTESIAN_POINT ( 'NONE',  ( 50.31550977796903368, 1.386241252175322014, -3.851058308531627450 ) ) ;
#11452 = ORIENTED_EDGE ( 'NONE', *, *, #29823, .F. ) ;
#11454 = CARTESIAN_POINT ( 'NONE',  ( 48.46963600013424411, -1.366688880095576319, -3.854642372925540350 ) ) ;
#11453 = LINE ( 'NONE', #18000, #4455 ) ;
#11455 = AXIS2_PLACEMENT_3D ( 'NONE', #13864, #2166, #28926 ) ;
#11456 = LINE ( 'NONE', #21141, #28117 ) ;
#11457 = CIRCLE ( 'NONE', #14048, 4.600000000000036948 ) ;
#11458 = AXIS2_PLACEMENT_3D ( 'NONE', #20920, #9035, #28196 ) ;
#11459 = VERTEX_POINT ( 'NONE', #7290 ) ;
#11460 = DIRECTION ( 'NONE',  ( 1.000000000000000000, 0.000000000000000000, 0.000000000000000000 ) ) ;
#11461 = CARTESIAN_POINT ( 'NONE',  ( -60.98542740578359656, 2.936324665650206445, 2.606018187048499968 ) ) ;
#11462 = CARTESIAN_POINT ( 'NONE',  ( -55.88452994616203995, 2.093608279459368564E-14, -3.600000000000198597 ) ) ;
#11463 = EDGE_LOOP ( 'NONE', ( #1283, #15001, #26197, #10325 ) ) ;
#11464 = AXIS2_PLACEMENT_3D ( 'NONE', #12366, #5719, #7945 ) ;
#11465 = ORIENTED_EDGE ( 'NONE', *, *, #29803, .F. ) ;
#11466 = CARTESIAN_POINT ( 'NONE',  ( 58.65000000000001990, 6.143261415694495821E-13, 3.111507638930570854E-58 ) ) ;
#11467 = ORIENTED_EDGE ( 'NONE', *, *, #26483, .T. ) ;
#11468 = AXIS2_PLACEMENT_3D ( 'NONE', #10553, #12904, #22430 ) ;
#11469 = CARTESIAN_POINT ( 'NONE',  ( 58.74160516400039711, -1.575205926126199252, 1.017053542742779149 ) ) ;
#11470 = LINE ( 'NONE', #30786, #21522 ) ;
#11471 = VERTEX_POINT ( 'NONE', #471 ) ;
#11472 = CARTESIAN_POINT ( 'NONE',  ( -59.27103329757905925, -2.428242106091486274, -1.066113908650147879 ) ) ;
#11473 = AXIS2_PLACEMENT_3D ( 'NONE', #19567, #22721, #10809 ) ;
#11474 = CIRCLE ( 'NONE', #20603, 0.05000000000000012768 ) ;
#11475 = DIRECTION ( 'NONE',  ( 1.000000000000000000, -0.000000000000000000, -0.000000000000000000 ) ) ;
#11476 = CARTESIAN_POINT ( 'NONE',  ( 33.47623932017462778, 4.375000000000001776, 5.357829746269670620E-16 ) ) ;
#11477 = ORIENTED_EDGE ( 'NONE', *, *, #3503, .F. ) ;
#11478 = ORIENTED_EDGE ( 'NONE', *, *, #21827, .T. ) ;
#11479 = EDGE_CURVE ( 'NONE', #30820, #23063, #466, .T. ) ;
#11480 = CARTESIAN_POINT ( 'NONE',  ( -60.49999999999997868, 1.656632322739229403E-15, 1.870925083934595927E-15 ) ) ;
#11481 = CARTESIAN_POINT ( 'NONE',  ( -55.47099364905386665, -3.399999999999995026, 0.9110272542656059347 ) ) ;
#11482 = CARTESIAN_POINT ( 'NONE',  ( -56.18749999999997868, -3.399999999999991029, -2.152687225432237718E-13 ) ) ;
#11483 = ORIENTED_EDGE ( 'NONE', *, *, #26317, .T. ) ;
#11484 = AXIS2_PLACEMENT_3D ( 'NONE', #27707, #8832, #5858 ) ;
#11485 = LINE ( 'NONE', #20990, #24544 ) ;
#11486 = CARTESIAN_POINT ( 'NONE',  ( 58.65000045311410304, 1.265716300432286223, 1.383426348887691448 ) ) ;
#11487 = AXIS2_PLACEMENT_3D ( 'NONE', #16406, #26058, #16886 ) ;
#11488 = DIRECTION ( 'NONE',  ( 0.000000000000000000, 1.000000000000000000, 3.491481338843137694E-15 ) ) ;
#11489 = AXIS2_PLACEMENT_3D ( 'NONE', #30260, #27564, #27886 ) ;
#11490 = CARTESIAN_POINT ( 'NONE',  ( 57.05000000000001847, 0.7500000000000000000, -1.778341924377873751 ) ) ;
#11492 = CARTESIAN_POINT ( 'NONE',  ( 51.31572262954152563, 0.7526089581382734428, -1.996089927833914146 ) ) ;
#11491 = FACE_OUTER_BOUND ( 'NONE', #5389, .T. ) ;
#11493 = VECTOR ( 'NONE', #29730, 1000.000000000000000 ) ;
#11494 = CARTESIAN_POINT ( 'NONE',  ( -59.67277382079201686, -2.169063742562021613, 1.523092617832624729 ) ) ;
#11495 = CARTESIAN_POINT ( 'NONE',  ( -59.19999999999996732, 4.156921938165317520, -0.9498634748674451567 ) ) ;
#11496 = AXIS2_PLACEMENT_3D ( 'NONE', #5042, #22307, #14697 ) ;
#11497 = EDGE_CURVE ( 'NONE', #11984, #23827, #14122, .T. ) ;
#11498 = CARTESIAN_POINT ( 'NONE',  ( 15.03925126672132961, 2.686240680702206785, -4.475885388010691912 ) ) ;
#11499 = TOROIDAL_SURFACE ( 'NONE', #29199, 4.200000000000016165, 0.1000000000000000056 ) ;
#11500 = LINE ( 'NONE', #11172, #10434 ) ;
#11501 = TOROIDAL_SURFACE ( 'NONE', #29200, 1.875000000000000222, 0.2500000000000000000 ) ;
#11502 = ORIENTED_EDGE ( 'NONE', *, *, #28754, .T. ) ;
#11503 = VERTEX_POINT ( 'NONE', #27056 ) ;
#11504 = CARTESIAN_POINT ( 'NONE',  ( -59.11126200777224682, -2.334442485522809196, 1.255257642634187043 ) ) ;
#11505 = VERTEX_POINT ( 'NONE', #5541 ) ;
#11506 = CARTESIAN_POINT ( 'NONE',  ( 53.13060515908007631, 4.213974700431092124, 2.049999999999814637 ) ) ;
#11507 = CARTESIAN_POINT ( 'NONE',  ( -55.84585481156723574, -1.184343223768586029, -3.558065644182725862 ) ) ;
#11509 = CARTESIAN_POINT ( 'NONE',  ( -36.56242893520592219, 3.350344226587738561, 4.246692235171849461 ) ) ;
#11508 = SPHERICAL_SURFACE ( 'NONE', #28149, 0.2500000000000000000 ) ;
#11510 = AXIS2_PLACEMENT_3D ( 'NONE', #25231, #18275, #8287 ) ;
#11511 = ORIENTED_EDGE ( 'NONE', *, *, #1270, .T. ) ;
#11512 = EDGE_LOOP ( 'NONE', ( #24838, #2629, #4281, #23834 ) ) ;
#11513 = CARTESIAN_POINT ( 'NONE',  ( -44.49999999999997868, 6.542789527549899840E-15, -1.397091617737396343E-15 ) ) ;
#11514 = CIRCLE ( 'NONE', #30211, 0.09999999999999942268 ) ;
#11515 = ORIENTED_EDGE ( 'NONE', *, *, #10268, .T. ) ;
#11516 = DIRECTION ( 'NONE',  ( 0.000000000000000000, 0.000000000000000000, -1.000000000000000000 ) ) ;
#11517 = AXIS2_PLACEMENT_3D ( 'NONE', #12499, #24389, #472 ) ;
#11518 = ORIENTED_EDGE ( 'NONE', *, *, #23721, .T. ) ;
#11520 = FACE_OUTER_BOUND ( 'NONE', #7499, .T. ) ;
#11519 = CARTESIAN_POINT ( 'NONE',  ( 50.37798322691364916, 1.327156576403631272, 3.879406274192440218 ) ) ;
#11521 = VERTEX_POINT ( 'NONE', #10136 ) ;
#11522 = CARTESIAN_POINT ( 'NONE',  ( 53.36555380356171696, 7.911905146458437343, 1.886361318289319522 ) ) ;
#11523 = DIRECTION ( 'NONE',  ( 0.8262273428075421755, 0.5633368246415175751, 0.000000000000000000 ) ) ;
#11524 = EDGE_CURVE ( 'NONE', #20372, #5085, #20204, .T. ) ;
#11525 = CARTESIAN_POINT ( 'NONE',  ( -54.49999999999997868, -1.549582583372307809, -3.331868970650947226 ) ) ;
#11526 = CARTESIAN_POINT ( 'NONE',  ( -37.18272003341174781, -5.407411300779149776, 6.622168941172400026E-16 ) ) ;
#11527 = CARTESIAN_POINT ( 'NONE',  ( -59.75952994616203284, -3.117691453623963938, -1.800000000000223199 ) ) ;
#11528 = CARTESIAN_POINT ( 'NONE',  ( 51.80351136591793448, 1.029101438728343254, 4.191235921151213795 ) ) ;
#11529 = CARTESIAN_POINT ( 'NONE',  ( 15.29449157529459136, 3.378578820314266817, 3.972872285093464129 ) ) ;
#11530 = CARTESIAN_POINT ( 'NONE',  ( -56.49986116251334778, 1.737685414808521678, -3.471684241605565546 ) ) ;
#11531 = VECTOR ( 'NONE', #24550, 1000.000000000000000 ) ;
#11532 = CIRCLE ( 'NONE', #1418, 3.286176633967618166 ) ;
#11533 = CARTESIAN_POINT ( 'NONE',  ( -56.79792740578360366, -1.073804522883507140, -3.225979517392339346 ) ) ;
#11534 = ADVANCED_FACE ( 'NONE', ( #5374 ), #3008, .T. ) ;
#11535 = CIRCLE ( 'NONE', #7420, 0.05000000000000012768 ) ;
#11536 = DIRECTION ( 'NONE',  ( -1.000000000000000000, -3.053848253006669023E-16, 2.042510438544995415E-16 ) ) ;
#11537 =( BOUNDED_CURVE ( )  B_SPLINE_CURVE ( 3, ( #17886, #8220, #1405, #3769 ),
 .UNSPECIFIED., .F., .T. ) 
 B_SPLINE_CURVE_WITH_KNOTS ( ( 4, 4 ),
 ( 5.006444828673937586, 5.249382619234884473 ),
 .UNSPECIFIED. ) 
 CURVE ( )  GEOMETRIC_REPRESENTATION_ITEM ( )  RATIONAL_B_SPLINE_CURVE ( ( 1.000000000000000000, 0.9950878134350367166, 0.9950878134350367166, 1.000000000000000000 ) ) 
 REPRESENTATION_ITEM ( '' )  );
#11538 = ORIENTED_EDGE ( 'NONE', *, *, #6394, .F. ) ;
#11539 = DIRECTION ( 'NONE',  ( 1.000000000000000000, -0.000000000000000000, -1.047444401652940007E-14 ) ) ;
#11540 = CARTESIAN_POINT ( 'NONE',  ( 54.36607077795601839, 6.714235712056786376, -2.039222690361167434 ) ) ;
#11541 = CARTESIAN_POINT ( 'NONE',  ( -36.56242893520594350, 0.2143423494566060183, 5.404929114625701914 ) ) ;
#11542 = CARTESIAN_POINT ( 'NONE',  ( 51.70000000000002416, 4.174380580618757719, 1.932497546739255556 ) ) ;
#11543 = EDGE_LOOP ( 'NONE', ( #11932, #21937, #20865, #27993 ) ) ;
#11544 = CARTESIAN_POINT ( 'NONE',  ( 58.72427158855720819, 1.646019958201105915, 0.8981388483289288738 ) ) ;
#11545 = ORIENTED_EDGE ( 'NONE', *, *, #19499, .F. ) ;
#11547 = PLANE ( 'NONE',  #17191 ) ;
#11546 = CARTESIAN_POINT ( 'NONE',  ( 58.65266784251151932, 0.9945725797260249745, -1.589569034372600775 ) ) ;
#11548 = ADVANCED_FACE ( 'NONE', ( #24241 ), #3002, .T. ) ;
#11549 = ORIENTED_EDGE ( 'NONE', *, *, #13003, .T. ) ;
#11550 = DIRECTION ( 'NONE',  ( -1.000000000000000000, -3.054025858079668409E-16, 2.042474015755241579E-16 ) ) ;
#11551 = B_SPLINE_CURVE_WITH_KNOTS ( 'NONE', 3,
 ( #26523, #30966, #24166, #19415, #7368, #17047, #5424, #15080, #1830, #11659, #21183, #9130, #18948, #26221, #25031, #10492 ),
 .UNSPECIFIED., .F., .F.,
 ( 4, 2, 2, 2, 2, 2, 2, 4 ),
 ( 5.358925739243605177E-21, 2.526926994603774344E-05, 5.053853989207548011E-05, 0.0001010770797841452004, 0.0002021541595682849798, 0.0004043083191365616112, 0.0008086166382731149824, 0.001617233276546221291 ),
 .UNSPECIFIED. ) ;
#11552 = DIRECTION ( 'NONE',  ( 0.000000000000000000, -0.6683962987621306917, 0.7438053426811914726 ) ) ;
#11554 = CARTESIAN_POINT ( 'NONE',  ( 60.94140446608462014, 0.5380862305989584371, -1.858165151370887669 ) ) ;
#11553 = CARTESIAN_POINT ( 'NONE',  ( 58.75000000000002132, 6.153735859711025284E-13, 3.111507638930570854E-58 ) ) ;
#11555 = EDGE_LOOP ( 'NONE', ( #884, #27229, #10998, #22075 ) ) ;
#11556 = CARTESIAN_POINT ( 'NONE',  ( -56.74999999999997158, 3.673546848079180638, 0.7533615035078058408 ) ) ;
#11557 = VECTOR ( 'NONE', #21729, 1000.000000000000000 ) ;
#11558 = CARTESIAN_POINT ( 'NONE',  ( -55.26905989232413674, -2.944486372867090473, 1.699999999999790345 ) ) ;
#11559 = ITEM_DEFINED_TRANSFORMATION ( 'NONE', 'NONE', #999,  #9018 ) ;
#11560 = ADVANCED_FACE ( 'NONE', ( #15194 ), #25240, .T. ) ;
#11561 = DIRECTION ( 'NONE',  ( 0.000000000000000000, 0.000000000000000000, -1.000000000000000000 ) ) ;
#11562 = DIRECTION ( 'NONE',  ( -1.000000000000000000, -0.000000000000000000, 0.000000000000000000 ) ) ;
#11563 = EDGE_CURVE ( 'NONE', #4137, #31086, #26767, .T. ) ;
#11564 = CARTESIAN_POINT ( 'NONE',  ( -62.09999999999998010, -2.698422353084989123, 0.1478368950964479289 ) ) ;
#11565 = ADVANCED_FACE ( 'NONE', ( #12202 ), #5075, .T. ) ;
#11566 = ORIENTED_EDGE ( 'NONE', *, *, #501, .T. ) ;
#11567 = CARTESIAN_POINT ( 'NONE',  ( 64.99999999999998579, 1.401298464324817071E-42, -3.500000000000680789 ) ) ;
#11568 = CARTESIAN_POINT ( 'NONE',  ( -36.22818246778666662, 2.595266697484551521, -4.757426534476516089 ) ) ;
#11569 = CARTESIAN_POINT ( 'NONE',  ( 48.34282069333976040, 1.210123066480781606, -3.917958458743180827 ) ) ;
#11570 = DIRECTION ( 'NONE',  ( 1.000000000000000000, 1.047444401652940007E-14, 0.000000000000000000 ) ) ;
#11571 = DIRECTION ( 'NONE',  ( 2.117927888850091331E-16, -0.02490330187381135929, 0.9996898646859343485 ) ) ;
#11573 = CARTESIAN_POINT ( 'NONE',  ( 41.48619405471885102, -151.3359592902622239, 2.049999999999835953 ) ) ;
#11572 = FACE_OUTER_BOUND ( 'NONE', #9224, .T. ) ;
#11574 = CARTESIAN_POINT ( 'NONE',  ( 58.75000000000003553, -1.320082690054267704, 1.469015551795647356 ) ) ;
#11575 = CARTESIAN_POINT ( 'NONE',  ( 50.34137136386935651, -1.344608935533137206, -3.858631320448701718 ) ) ;
#11576 = ORIENTED_EDGE ( 'NONE', *, *, #6628, .F. ) ;
#11577 = AXIS2_PLACEMENT_3D ( 'NONE', #19379, #4958, #14611 ) ;
#11578 = DIRECTION ( 'NONE',  ( 0.000000000000000000, 0.000000000000000000, 1.000000000000000000 ) ) ;
#11579 = DIRECTION ( 'NONE',  ( -0.000000000000000000, 1.000000000000000000, 0.000000000000000000 ) ) ;
#11581 = FACE_OUTER_BOUND ( 'NONE', #30180, .T. ) ;
#11580 = CARTESIAN_POINT ( 'NONE',  ( 58.75000000000000000, 1.932246131437593162, 0.4087173687853760673 ) ) ;
#11582 = CARTESIAN_POINT ( 'NONE',  ( 15.74652664997095286, -5.076023720898155567, 1.868859051106972036 ) ) ;
#11583 = EDGE_CURVE ( 'NONE', #1670, #24820, #4523, .T. ) ;
#11584 = ORIENTED_EDGE ( 'NONE', *, *, #5136, .T. ) ;
#11585 = ORIENTED_EDGE ( 'NONE', *, *, #10250, .F. ) ;
#11586 = CARTESIAN_POINT ( 'NONE',  ( 15.03925126672132961, -2.199885893005931070, -4.939696249117691451 ) ) ;
#11587 = CARTESIAN_POINT ( 'NONE',  ( 50.32622512580983454, -1.373801017329605578, 3.853344662332956361 ) ) ;
#11588 = ORIENTED_EDGE ( 'NONE', *, *, #3028, .T. ) ;
#11589 = ADVANCED_FACE ( 'NONE', ( #8074 ), #8554, .F. ) ;
#11590 = CARTESIAN_POINT ( 'NONE',  ( 58.75000000000000711, 0.8897917884438335534, 1.791164585743606041 ) ) ;
#11591 = ORIENTED_EDGE ( 'NONE', *, *, #19481, .T. ) ;
#11592 = CARTESIAN_POINT ( 'NONE',  ( 58.65000038048045639, 1.873220289783266601, -0.08335421200033678313 ) ) ;
#11593 = VERTEX_POINT ( 'NONE', #13410 ) ;
#11594 = CARTESIAN_POINT ( 'NONE',  ( -60.39405989232410121, -2.944486372867076263, -1.700000000000224665 ) ) ;
#11595 = ORIENTED_EDGE ( 'NONE', *, *, #15854, .T. ) ;
#11596 = DIRECTION ( 'NONE',  ( 1.000000000000000000, 0.000000000000000000, 0.000000000000000000 ) ) ;
#11597 = ORIENTED_EDGE ( 'NONE', *, *, #708, .T. ) ;
#11598 = EDGE_CURVE ( 'NONE', #24542, #21838, #11088, .T. ) ;
#11599 = VERTEX_POINT ( 'NONE', #22952 ) ;
#11600 = PRODUCT_DEFINITION_FORMATION_WITH_SPECIFIED_SOURCE ( 'ANY', '', #26984, .NOT_KNOWN. ) ;
#11601 = AXIS2_PLACEMENT_3D ( 'NONE', #19489, #29137, #17125 ) ;
#11602 = CARTESIAN_POINT ( 'NONE',  ( -59.93749999999996447, -3.925981830489445379, -2.268305517232443506E-13 ) ) ;
#11603 = CARTESIAN_POINT ( 'NONE',  ( 56.99824518417612751, -0.8016297048612398557, 2.473345119325445651 ) ) ;
#11604 = CARTESIAN_POINT ( 'NONE',  ( 28.44937284992262150, 5.648694717987697622, -1.425000000000099298 ) ) ;
#11605 = DIRECTION ( 'NONE',  ( 1.000000000000000000, 3.053848253006669023E-16, -2.042510438544995415E-16 ) ) ;
#11606 = DIRECTION ( 'NONE',  ( 0.000000000000000000, 0.000000000000000000, 1.000000000000000000 ) ) ;
#11607 = DIRECTION ( 'NONE',  ( 0.000000000000000000, 0.000000000000000000, 1.000000000000000000 ) ) ;
#11608 = CARTESIAN_POINT ( 'NONE',  ( 47.10000000000002984, -4.276948333784437395, 0.9210526315789471230 ) ) ;
#11609 = CARTESIAN_POINT ( 'NONE',  ( 59.00000000000006395, 4.898587196589412829E-16, 3.999999999999382716 ) ) ;
#11610 = CARTESIAN_POINT ( 'NONE',  ( -36.89831264271882105, -3.408535483610560579, -4.200031884472264387 ) ) ;
#11611 = CARTESIAN_POINT ( 'NONE',  ( 56.95206911348624601, 0.7375298837344119729, 2.493227876267903653 ) ) ;
#11613 = VECTOR ( 'NONE', #325, 1000.000000000000000 ) ;
#11612 = DIRECTION ( 'NONE',  ( 0.000000000000000000, 4.440892098500626951E-15, -1.000000000000000000 ) ) ;
#11614 = CARTESIAN_POINT ( 'NONE',  ( 52.91409500010723121, 8.434844866547615894, 2.049999999999815525 ) ) ;
#11615 = VERTEX_POINT ( 'NONE', #10749 ) ;
#11617 = CARTESIAN_POINT ( 'NONE',  ( 48.40115653635459125, -0.8930148142854139603, -3.925689827643446428 ) ) ;
#11616 = CARTESIAN_POINT ( 'NONE',  ( 51.17290532404553716, -0.9646187004837835088, -1.462925393634369353 ) ) ;
#11618 = ADVANCED_FACE ( 'NONE', ( #17889 ), #15652, .T. ) ;
#11619 = CARTESIAN_POINT ( 'NONE',  ( 51.67696994838494362, -3.663337715290890362, -1.844354128036493234 ) ) ;
#11620 = PRODUCT_DEFINITION_FORMATION_WITH_SPECIFIED_SOURCE ( 'ANY', '', #10308, .NOT_KNOWN. ) ;
#11621 = ADVANCED_FACE ( 'NONE', ( #12967 ), #18681, .T. ) ;
#11622 = AXIS2_PLACEMENT_3D ( 'NONE', #9948, #5185, #12458 ) ;
#11623 = TOROIDAL_SURFACE ( 'NONE', #19731, 0.3000000000000000444, 0.05000000000000000278 ) ;
#11624 = VERTEX_POINT ( 'NONE', #3941 ) ;
#11625 = EDGE_CURVE ( 'NONE', #5886, #2222, #1507, .T. ) ;
#11626 = CARTESIAN_POINT ( 'NONE',  ( 51.64281244548084970, 0.8321733326272462428, 1.569379851958426331 ) ) ;
#11627 = FACE_OUTER_BOUND ( 'NONE', #23579, .T. ) ;
#11628 = CARTESIAN_POINT ( 'NONE',  ( -58.99999999999995737, 2.023778652682509683E-14, -3.400000000000209521 ) ) ;
#11629 = ORIENTED_EDGE ( 'NONE', *, *, #5092, .F. ) ;
#11630 = VERTEX_POINT ( 'NONE', #27525 ) ;
#11631 = CARTESIAN_POINT ( 'NONE',  ( 15.29954477411523506, 4.683225668089404437, 2.703237747136276070 ) ) ;
#11632 = VERTEX_POINT ( 'NONE', #15510 ) ;
#11633 = CARTESIAN_POINT ( 'NONE',  ( 58.74154451056427462, -1.668374833162466153, 0.8556855217791524693 ) ) ;
#11634 = CARTESIAN_POINT ( 'NONE',  ( -54.44702994616203995, -2.078460969082631227, -3.600000000000199485 ) ) ;
#11635 = ORIENTED_EDGE ( 'NONE', *, *, #540, .F. ) ;
#11636 = CARTESIAN_POINT ( 'NONE',  ( -59.09999999999997300, -2.465712773623968790, -0.9709585562669303949 ) ) ;
#11637 = DIRECTION ( 'NONE',  ( 1.047444401652940007E-14, 0.000000000000000000, 1.000000000000000000 ) ) ;
#11638 = FACE_OUTER_BOUND ( 'NONE', #17866, .T. ) ;
#11639 = ORIENTED_EDGE ( 'NONE', *, *, #20587, .F. ) ;
#11640 = VERTEX_POINT ( 'NONE', #17740 ) ;
#11641 = EDGE_CURVE ( 'NONE', #14026, #4137, #25168, .T. ) ;
#11642 = CARTESIAN_POINT ( 'NONE',  ( 15.03925126672132784, 4.383220986679485343, -0.4611378927914090986 ) ) ;
#11643 = CARTESIAN_POINT ( 'NONE',  ( -55.49999999999997868, -2.944486372867090473, 1.699999999999789679 ) ) ;
#11644 = CARTESIAN_POINT ( 'NONE',  ( 58.64999999999999858, 1.655311165517639349, -1.077297519404308179 ) ) ;
#11645 = ORIENTED_EDGE ( 'NONE', *, *, #25955, .T. ) ;
#11646 = CARTESIAN_POINT ( 'NONE',  ( -77.28999999999996362, -3.470778894058966809E-15, 5.300300110251643219E-15 ) ) ;
#11647 = DIRECTION ( 'NONE',  ( 1.000000000000000000, 1.047444401652940007E-14, -0.000000000000000000 ) ) ;
#11648 = CARTESIAN_POINT ( 'NONE',  ( -57.77499999999997016, -0.9743475445367594245, 4.751120590182401848 ) ) ;
#11650 = CARTESIAN_POINT ( 'NONE',  ( 15.03925126672132961, -4.018128179617543871, 3.618665901676652918 ) ) ;
#11649 = CARTESIAN_POINT ( 'NONE',  ( -35.85663232820581925, -2.686240680702169481, 4.475885388010719446 ) ) ;
#11651 = PRODUCT_DEFINITION ( 'UNKNOWN', '', #11620, #9819 ) ;
#11652 = PRODUCT ( 'MAS-683', 'MAS-683', '', ( #634 ) ) ;
#11653 = VECTOR ( 'NONE', #25405, 999.9999999999998863 ) ;
#11654 = CARTESIAN_POINT ( 'NONE',  ( 60.94140446606686368, -0.5380862305903196807, -1.858165151418244010 ) ) ;
#11655 = CARTESIAN_POINT ( 'NONE',  ( 47.10000000000002274, -4.276948333784438283, 0.9210526315789470120 ) ) ;
#11656 = CARTESIAN_POINT ( 'NONE',  ( 58.75000000000002132, 6.153735859711025284E-13, 3.111507638930570854E-58 ) ) ;
#11657 = ORIENTED_EDGE ( 'NONE', *, *, #15444, .T. ) ;
#11658 = ADVANCED_FACE ( 'NONE', ( #25466 ), #3771, .T. ) ;
#11659 = CARTESIAN_POINT ( 'NONE',  ( 51.84418490562190129, 0.2543151237804266995, -4.351520533650278466 ) ) ;
#11660 =( BOUNDED_SURFACE ( )  B_SPLINE_SURFACE ( 3, 2, ( 
 ( #22122, #12279, #19888 ),
 ( #29378, #24786, #416 ),
 ( #5157, #27162, #21963 ),
 ( #12589, #5007, #24628 ),
 ( #7689, #27319, #10370 ),
 ( #14665, #251, #9915 ),
 ( #2945, #14807, #7833 ),
 ( #12891, #3249, #12429 ),
 ( #5632, #10073, #8160 ),
 ( #24928, #22581, #24328 ),
 ( #29236, #885, #19747 ),
 ( #17349, #20051, #10544 ),
 ( #17509, #15282, #26996 ),
 ( #10219, #7547, #5301 ),
 ( #15126, #29690, #19595 ),
 ( #20217, #17208, #29848 ),
 ( #14959, #24467, #22276 ),
 ( #17830, #3093, #561 ),
 ( #29518, #5478, #12741 ),
 ( #22418, #710, #8010 ),
 ( #17673, #6105, #23042 ),
 ( #20523, #11152, #11296 ),
 ( #1636, #6409, #30457 ),
 ( #16070, #18449, #23355 ),
 ( #10690, #6251, #20978 ),
 ( #15435, #25088, #20828 ),
 ( #8760, #30151, #20373 ),
 ( #28087, #25403, #3422 ),
 ( #8619, #11004, #13673 ),
 ( #1495, #8473, #27466 ),
 ( #27935, #20685, #13061 ),
 ( #22744, #3710, #30310 ),
 ( #13349, #18296, #30613 ),
 ( #5954, #15756, #25723 ) ),
 .UNSPECIFIED., .F., .F., .T. ) 
 B_SPLINE_SURFACE_WITH_KNOTS ( ( 4, 2, 2, 2, 2, 2, 2, 2, 2, 2, 2, 2, 2, 2, 2, 2, 4 ),
 ( 3, 3 ),
 ( -1.734723475976807094E-18, 0.001741451497654476635, 0.002612177246481715929, 0.003047540120895335467, 0.003482902995308955005, 0.004353628744136194516, 0.005224354492963433592, 0.006965805990617911746, 0.007836531739445151690, 0.008707257488272390766, 0.009577983237099629843, 0.01044870898592686892, 0.01131943473475410800, 0.01219016048358134707, 0.01262552335799496661, 0.01306088623240858615, 0.01393161198123582523 ),
 ( 0.000000000000000000, 1.000000000000000000 ),
 .UNSPECIFIED. ) 
 GEOMETRIC_REPRESENTATION_ITEM ( )  RATIONAL_B_SPLINE_SURFACE ( (
 ( 1.000000000000000000, 0.7071067811865475727, 1.000000000000000000),
 ( 1.000000000000000000, 0.7071067811865475727, 1.000000000000000000),
 ( 1.000000000000000000, 0.7071067811865475727, 1.000000000000000000),
 ( 1.000000000000000000, 0.7071067811865475727, 1.000000000000000000),
 ( 1.000000000000000000, 0.7071067811865467956, 1.000000000000000000),
 ( 1.000000000000000000, 0.7071067811865467956, 1.000000000000000000),
 ( 1.000000000000000000, 0.7071067811865494601, 1.000000000000000000),
 ( 1.000000000000000000, 0.7071067811865494601, 1.000000000000000000),
 ( 1.000000000000000000, 0.7071067811865490160, 1.000000000000000000),
 ( 1.000000000000000000, 0.7071067811865490160, 1.000000000000000000),
 ( 1.000000000000000000, 0.7071067811865490160, 1.000000000000000000),
 ( 1.000000000000000000, 0.7071067811865490160, 1.000000000000000000),
 ( 1.000000000000000000, 0.7071067811865490160, 1.000000000000000000),
 ( 1.000000000000000000, 0.7071067811865490160, 1.000000000000000000),
 ( 1.000000000000000000, 0.7071067811865482389, 1.000000000000000000),
 ( 1.000000000000000000, 0.7071067811865482389, 1.000000000000000000),
 ( 1.000000000000000000, 0.7071067811865452413, 1.000000000000000000),
 ( 1.000000000000000000, 0.7071067811865452413, 1.000000000000000000),
 ( 1.000000000000000000, 0.7071067811865475727, 1.000000000000000000),
 ( 1.000000000000000000, 0.7071067811865475727, 1.000000000000000000),
 ( 1.000000000000000000, 0.7071067811865482389, 1.000000000000000000),
 ( 1.000000000000000000, 0.7071067811865482389, 1.000000000000000000),
 ( 1.000000000000000000, 0.7071067811865436870, 1.000000000000000000),
 ( 1.000000000000000000, 0.7071067811865436870, 1.000000000000000000),
 ( 1.000000000000000000, 0.7071067811865460184, 1.000000000000000000),
 ( 1.000000000000000000, 0.7071067811865460184, 1.000000000000000000),
 ( 1.000000000000000000, 0.7071067811865460184, 1.000000000000000000),
 ( 1.000000000000000000, 0.7071067811865460184, 1.000000000000000000),
 ( 1.000000000000000000, 0.7071067811865471286, 1.000000000000000000),
 ( 1.000000000000000000, 0.7071067811865471286, 1.000000000000000000),
 ( 1.000000000000000000, 0.7071067811865467956, 1.000000000000000000),
 ( 1.000000000000000000, 0.7071067811865467956, 1.000000000000000000),
 ( 1.000000000000000000, 0.7071067811865467956, 1.000000000000000000),
 ( 1.000000000000000000, 0.7071067811865467956, 1.000000000000000000) ) ) 
 REPRESENTATION_ITEM ( '' )  SURFACE ( )  );
#11661 = ORIENTED_EDGE ( 'NONE', *, *, #24738, .T. ) ;
#11662 = CARTESIAN_POINT ( 'NONE',  ( 53.53640187423186347, 5.215699251213393950, 2.049999999999812861 ) ) ;
#11663 = CARTESIAN_POINT ( 'NONE',  ( -55.47085481156723574, 1.184343223768591580, 3.558065644182726750 ) ) ;
#11665 = CARTESIAN_POINT ( 'NONE',  ( 51.25604564026579624, -3.873096995916275098, -1.345769568645377223 ) ) ;
#11664 = CARTESIAN_POINT ( 'NONE',  ( -54.39999999999996305, 1.500000000000023759, -3.959797974644871044 ) ) ;
#11666 = ORIENTED_EDGE ( 'NONE', *, *, #17537, .F. ) ;
#11667 = VERTEX_POINT ( 'NONE', #22812 ) ;
#11668 = CARTESIAN_POINT ( 'NONE',  ( 60.81561938753818453, 0.6500000000006365131, -1.489337100860648633 ) ) ;
#11669 = ORIENTED_EDGE ( 'NONE', *, *, #26819, .F. ) ;
#11670 = CARTESIAN_POINT ( 'NONE',  ( -62.29999999999998295, -2.749147127886318653, -0.06848408015297868801 ) ) ;
#11671 = ORIENTED_EDGE ( 'NONE', *, *, #9233, .T. ) ;
#11673 = CARTESIAN_POINT ( 'NONE',  ( -35.85663232820584057, -2.199885893005967041, 4.939696249117680793 ) ) ;
#11672 = CARTESIAN_POINT ( 'NONE',  ( 58.75000000000003553, -1.932246131436463843, -0.4087173687848976722 ) ) ;
#11674 = ORIENTED_EDGE ( 'NONE', *, *, #26865, .T. ) ;
#11675 = CARTESIAN_POINT ( 'NONE',  ( 58.65000038048045639, 1.787818198675105386, -0.5653390727695211115 ) ) ;
#11676 = B_SPLINE_CURVE_WITH_KNOTS ( 'NONE', 3,
 ( #10676, #27302, #29091, #3234, #14684, #31312, #17658 ),
 .UNSPECIFIED., .F., .F.,
 ( 4, 3, 4 ),
 ( 0.000000000000000000, 3.134674146556711401E-05, 4.413594575983409879E-05 ),
 .UNSPECIFIED. ) ;
#11677 = CIRCLE ( 'NONE', #23314, 0.2600000000000000644 ) ;
#11678 = EDGE_CURVE ( 'NONE', #15593, #4345, #20432, .T. ) ;
#11679 = CARTESIAN_POINT ( 'NONE',  ( -54.46462222424374033, -1.502185874895793694, -3.301501926143236787 ) ) ;
#11680 = DIRECTION ( 'NONE',  ( 0.000000000000000000, -4.336808689942024836E-15, 1.000000000000000000 ) ) ;
#11681 = CARTESIAN_POINT ( 'NONE',  ( -58.75952994616203284, 3.117691453623994580, -1.800000000000195000 ) ) ;
#11682 = CARTESIAN_POINT ( 'NONE',  ( -59.12853372169517741, -2.475303475092485606, -0.9578223113486030726 ) ) ;
#11683 = CARTESIAN_POINT ( 'NONE',  ( -59.19999999999997442, -3.317600071788705307, 0.9555264641437645201 ) ) ;
#11684 = DIRECTION ( 'NONE',  ( 0.000000000000000000, 0.2008964009354162750, -0.9796124928211136229 ) ) ;
#11685 = CARTESIAN_POINT ( 'NONE',  ( -57.92292740578360366, 1.073804522883512691, 3.225979517392339346 ) ) ;
#11686 = CARTESIAN_POINT ( 'NONE',  ( 50.87477060347374902, 8.633605004118187765, 1.949999999999822320 ) ) ;
#11687 = VERTEX_POINT ( 'NONE', #20593 ) ;
#11688 = CARTESIAN_POINT ( 'NONE',  ( 58.45000000000001705, 0.8000000000000000444, 2.421260002560649660 ) ) ;
#11689 = CARTESIAN_POINT ( 'NONE',  ( -36.50489844130379424, 0.3564988296780842725, 5.398869307934828221 ) ) ;
#11690 = DIRECTION ( 'NONE',  ( -4.270088556250598741E-15, 0.000000000000000000, -1.000000000000000000 ) ) ;
#11691 = EDGE_LOOP ( 'NONE', ( #11429, #7294, #6828, #30178 ) ) ;
#11692 = EDGE_CURVE ( 'NONE', #9227, #2190, #2522, .T. ) ;
#11693 = CARTESIAN_POINT ( 'NONE',  ( 47.00000000000002132, 2.428612866367529932E-14, 0.000000000000000000 ) ) ;
#11694 = ORIENTED_EDGE ( 'NONE', *, *, #9811, .F. ) ;
#11695 = EDGE_CURVE ( 'NONE', #20184, #25246, #18704, .T. ) ;
#11696 = CARTESIAN_POINT ( 'NONE',  ( 34.56269065792917417, 8.313757757582560970, 1.949999999999879607 ) ) ;
#11698 = FACE_OUTER_BOUND ( 'NONE', #14116, .T. ) ;
#11697 = CARTESIAN_POINT ( 'NONE',  ( 51.88812122917402547, 8.998461838226445408, 2.049999999999819522 ) ) ;
#11699 = EDGE_LOOP ( 'NONE', ( #11292, #17698, #16181, #30483 ) ) ;
#11700 = CARTESIAN_POINT ( 'NONE',  ( 50.59602332238209499, -0.1408342061598474859, 0.8215393206232036727 ) ) ;
#11701 = DIRECTION ( 'NONE',  ( 1.000000000000000000, 3.053848253006669023E-16, -2.042510438544995415E-16 ) ) ;
#11703 = DIRECTION ( 'NONE',  ( 0.000000000000000000, 0.9996898646859343485, 0.02490330187381123439 ) ) ;
#11702 = DIRECTION ( 'NONE',  ( 0.000000000000000000, -1.000000000000000000, 0.000000000000000000 ) ) ;
#11704 = ORIENTED_EDGE ( 'NONE', *, *, #2967, .F. ) ;
#11705 = CARTESIAN_POINT ( 'NONE',  ( -60.54792740578359656, -1.073804522883517576, -3.225979517392334905 ) ) ;
#11706 = CARTESIAN_POINT ( 'NONE',  ( 51.70000000000002416, 6.982261990806648555E-14, -1.793082891011605378E-13 ) ) ;
#11707 = DIRECTION ( 'NONE',  ( -0.000000000000000000, -0.000000000000000000, -1.000000000000000000 ) ) ;
#11708 = CARTESIAN_POINT ( 'NONE',  ( -36.00197790576392265, 2.199885893005899096, 4.939696249117698557 ) ) ;
#11709 = AXIS2_PLACEMENT_3D ( 'NONE', #22149, #26873, #24491 ) ;
#11710 = AXIS2_PLACEMENT_3D ( 'NONE', #19895, #24790, #27323 ) ;
#11711 = EDGE_CURVE ( 'NONE', #133, #4604, #7578, .T. ) ;
#11712 = DIRECTION ( 'NONE',  ( 0.5633368246415186853, -0.8262273428075416204, 0.000000000000000000 ) ) ;
#11713 = DIRECTION ( 'NONE',  ( -0.4772254810013855097, 0.8787808829753844808, 1.772289120718281137E-15 ) ) ;
#11714 = CARTESIAN_POINT ( 'NONE',  ( -54.46439202372638277, 1.502116081466616793, -4.031358338852112588 ) ) ;
#11715 = VERTEX_POINT ( 'NONE', #20282 ) ;
#11716 = FACE_OUTER_BOUND ( 'NONE', #11173, .T. ) ;
#11717 = CARTESIAN_POINT ( 'NONE',  ( -36.89017861347080185, 2.910597594660179421, -4.559461819278051387 ) ) ;
#11718 = DIRECTION ( 'NONE',  ( 0.000000000000000000, 0.000000000000000000, 1.000000000000000000 ) ) ;
#11719 = DIRECTION ( 'NONE',  ( 1.000000000000000000, 3.054025858079668409E-16, -2.042474015755241579E-16 ) ) ;
#11720 = EDGE_CURVE ( 'NONE', #28796, #10216, #15961, .T. ) ;
#11721 = CARTESIAN_POINT ( 'NONE',  ( 57.00797408584070070, -0.7277374606022131154, -2.435538690626270597 ) ) ;
#11722 = CIRCLE ( 'NONE', #21357, 0.1000000000000000472 ) ;
#11724 = DIRECTION ( 'NONE',  ( 1.000000000000000000, 3.053848253006669023E-16, -2.042510438544995415E-16 ) ) ;
#11723 = CARTESIAN_POINT ( 'NONE',  ( 50.25000000000004263, -1.791164585743077797, 0.8897917884442223535 ) ) ;
#11725 = CARTESIAN_POINT ( 'NONE',  ( 51.94586448161385306, 3.919599535333307294, -2.045267140517447402 ) ) ;
#11727 = PLANE ( 'NONE',  #8422 ) ;
#11726 = CARTESIAN_POINT ( 'NONE',  ( -64.28602961791190751, 5.004363292900432036E-16, 2.644225585457161048E-15 ) ) ;
#11728 = ORIENTED_EDGE ( 'NONE', *, *, #18038, .F. ) ;
#11729 = CIRCLE ( 'NONE', #22356, 0.1000000000000000472 ) ;
#11730 = ADVANCED_FACE ( 'NONE', ( #6311 ), #27151, .F. ) ;
#11731 = CARTESIAN_POINT ( 'NONE',  ( 58.65000038048068376, -1.787818198674085757, 0.5653390727688525352 ) ) ;
#11732 = EDGE_CURVE ( 'NONE', #30383, #21345, #4042, .T. ) ;
#11733 = FACE_OUTER_BOUND ( 'NONE', #24885, .T. ) ;
#11735 = CARTESIAN_POINT ( 'NONE',  ( -35.98952425903310370, 5.086913993735653783, 1.171642046065924481 ) ) ;
#11734 = CARTESIAN_POINT ( 'NONE',  ( 15.03925126672125856, -2.525801270006271082, -4.794550352686344219 ) ) ;
#11736 = CARTESIAN_POINT ( 'NONE',  ( 15.61033468494287924, -5.277035221755875583, 1.205525476379309735 ) ) ;
#11737 = ORIENTED_EDGE ( 'NONE', *, *, #2062, .T. ) ;
#11738 = ORIENTED_EDGE ( 'NONE', *, *, #18563, .F. ) ;
#11739 = LINE ( 'NONE', #28365, #16900 ) ;
#11740 = EDGE_LOOP ( 'NONE', ( #14276, #20668, #11095, #30661 ) ) ;
#11741 = CARTESIAN_POINT ( 'NONE',  ( 56.98981708175836758, 0.7951539052630037796, -2.475425269917271187 ) ) ;
#11742 = DIRECTION ( 'NONE',  ( 0.000000000000000000, -0.2745098039215673746, -0.9615843008030769967 ) ) ;
#11743 = ORIENTED_EDGE ( 'NONE', *, *, #17031, .F. ) ;
#11744 = CARTESIAN_POINT ( 'NONE',  ( 58.66118217212520136, 1.874997884620083211, -0.01689491344017308647 ) ) ;
#11745 = ORIENTED_EDGE ( 'NONE', *, *, #16089, .F. ) ;
#11746 = EDGE_CURVE ( 'NONE', #22512, #30820, #15161, .T. ) ;
#11747 = CARTESIAN_POINT ( 'NONE',  ( -61.01905989232410121, 2.023778652682512207E-14, -3.400000000000216183 ) ) ;
#11748 = EDGE_LOOP ( 'NONE', ( #25935, #14443, #13208, #16703 ) ) ;
#11749 = ORIENTED_EDGE ( 'NONE', *, *, #19270, .F. ) ;
#11750 = ORIENTED_EDGE ( 'NONE', *, *, #9489, .F. ) ;
#11751 = CARTESIAN_POINT ( 'NONE',  ( -59.87499999999995737, -2.944486372867076707, -1.700000000000223332 ) ) ;
#11752 = DIRECTION ( 'NONE',  ( 1.000000000000000000, -1.219044193948983948E-29, 3.491481338843133355E-15 ) ) ;
#11753 = CARTESIAN_POINT ( 'NONE',  ( 60.94140446606686368, -0.5380862305903196807, -1.858165151418244010 ) ) ;
#11754 = DIRECTION ( 'NONE',  ( 1.000000000000000000, 1.047444401652940007E-14, 0.000000000000000000 ) ) ;
#11755 = B_SPLINE_CURVE_WITH_KNOTS ( 'NONE', 3,
 ( #2288, #31273, #23365, #1646 ),
 .UNSPECIFIED., .F., .F.,
 ( 4, 4 ),
 ( 0.000000000000000000, 2.777217045962147943E-05 ),
 .UNSPECIFIED. ) ;
#11756 = EDGE_CURVE ( 'NONE', #9597, #5233, #27802, .T. ) ;
#11757 = CARTESIAN_POINT ( 'NONE',  ( -61.11832338958127053, -2.488248221111335923, -0.8735822397580453869 ) ) ;
#11758 = EDGE_CURVE ( 'NONE', #30450, #19424, #14061, .T. ) ;
#11759 = CARTESIAN_POINT ( 'NONE',  ( 51.73504510627559938, 4.165466613856895428, -1.939072597264996700 ) ) ;
#11760 = VECTOR ( 'NONE', #9333, 1000.000000000000000 ) ;
#11761 = CARTESIAN_POINT ( 'NONE',  ( 47.00000000000002132, -4.227689052994015206, 1.125730994152047026 ) ) ;
#11762 = DIRECTION ( 'NONE',  ( 0.000000000000000000, 0.000000000000000000, -1.000000000000000000 ) ) ;
#11763 = ORIENTED_EDGE ( 'NONE', *, *, #18125, .F. ) ;
#11764 = DIRECTION ( 'NONE',  ( 0.000000000000000000, 0.000000000000000000, 1.000000000000000000 ) ) ;
#11765 = EDGE_CURVE ( 'NONE', #26730, #23673, #20228, .T. ) ;
#11766 = CARTESIAN_POINT ( 'NONE',  ( 33.47623932017462778, 1.734723475976807094E-15, 0.000000000000000000 ) ) ;
#11767 = ORIENTED_EDGE ( 'NONE', *, *, #30200, .T. ) ;
#11769 = CARTESIAN_POINT ( 'NONE',  ( 50.36581974271289397, -1.399739523915384698, 3.853780793998482945 ) ) ;
#11768 = LINE ( 'NONE', #23812, #18045 ) ;
#11771 = ADVANCED_FACE ( 'NONE', ( #7111 ), #14368, .F. ) ;
#11770 = CARTESIAN_POINT ( 'NONE',  ( 54.28500427175510623, 6.002439417116981701, -2.050000000000186784 ) ) ;
#11772 = CARTESIAN_POINT ( 'NONE',  ( -62.09999999999997300, 2.699162634652024551, 0.06723891505929256718 ) ) ;
#11773 = EDGE_LOOP ( 'NONE', ( #27705, #14338, #25948, #30270 ) ) ;
#11774 = DIRECTION ( 'NONE',  ( -1.000000000000000000, 0.000000000000000000, 0.000000000000000000 ) ) ;
#11775 = CARTESIAN_POINT ( 'NONE',  ( 51.77478101728125637, -4.051679580537264513, 1.951144708070448708 ) ) ;
#11776 = CARTESIAN_POINT ( 'NONE',  ( -60.99999999999997158, 2.944486372867092250, 1.699999999999795008 ) ) ;
#11777 = ORIENTED_EDGE ( 'NONE', *, *, #12126, .T. ) ;
#11778 = EDGE_LOOP ( 'NONE', ( #7622, #3335 ) ) ;
#11779 = CARTESIAN_POINT ( 'NONE',  ( 22.54717926605044909, 7.740376438784151603, 1.424999999999921663 ) ) ;
#11780 = EDGE_LOOP ( 'NONE', ( #18926, #11815, #11585, #26991 ) ) ;
#11781 = CARTESIAN_POINT ( 'NONE',  ( 51.82286850391904665, 4.509570184545037108, -0.9171356268414241342 ) ) ;
#11782 = CARTESIAN_POINT ( 'NONE',  ( -58.00952994616203284, 3.117691453623994580, -1.800000000000192557 ) ) ;
#11783 = ORIENTED_EDGE ( 'NONE', *, *, #27509, .F. ) ;
#11784 = FACE_OUTER_BOUND ( 'NONE', #109, .T. ) ;
#11785 = AXIS2_PLACEMENT_3D ( 'NONE', #1325, #30300, #8915 ) ;
#11786 = CARTESIAN_POINT ( 'NONE',  ( 36.50000000000002132, -0.7794871794871797155, 1.732743413496390161 ) ) ;
#11787 = CARTESIAN_POINT ( 'NONE',  ( 31.90749320846298431, 7.645246315295118222, 1.949999999999919797 ) ) ;
#11788 = ORIENTED_EDGE ( 'NONE', *, *, #11078, .T. ) ;
#11789 = ORIENTED_EDGE ( 'NONE', *, *, #324, .T. ) ;
#11790 = CYLINDRICAL_SURFACE ( 'NONE', #5671, 3.750000000000000444 ) ;
#11791 = CARTESIAN_POINT ( 'NONE',  ( -62.09999999999997300, -2.657853763656952140, 0.1506955384656827324 ) ) ;
#11792 = CARTESIAN_POINT ( 'NONE',  ( 58.75000000000002842, -0.8980135333480974147, -1.749295403805072757 ) ) ;
#11793 = ORIENTED_EDGE ( 'NONE', *, *, #1505, .F. ) ;
#11794 = DIRECTION ( 'NONE',  ( 1.344447539785323523E-44, -1.000000000000000000, -3.491481338843137300E-15 ) ) ;
#11795 = ADVANCED_FACE ( 'NONE', ( #21377 ), #11547, .T. ) ;
#11796 = DIRECTION ( 'NONE',  ( 0.000000000000000000, -1.000000000000000000, 0.000000000000000000 ) ) ;
#11797 = EDGE_CURVE ( 'NONE', #25939, #28152, #18211, .T. ) ;
#11798 = ADVANCED_FACE ( 'NONE', ( #11698 ), #30321, .F. ) ;
#11799 = DIRECTION ( 'NONE',  ( -1.000000000000000000, -3.053848253006669023E-16, 2.042510438544995415E-16 ) ) ;
#11801 = CARTESIAN_POINT ( 'NONE',  ( 58.65000000000004121, -1.834410884275093911, -0.3880228184666750235 ) ) ;
#11800 = CARTESIAN_POINT ( 'NONE',  ( -59.50035777917753421, 3.117067508592329617, 1.404346055332197585 ) ) ;
#11802 = CARTESIAN_POINT ( 'NONE',  ( 51.22715433738865443, 0.9941391646906797552, 1.410349289489640556 ) ) ;
#11803 = DIRECTION ( 'NONE',  ( 1.000000000000000000, 1.047444401652940007E-14, 0.000000000000000000 ) ) ;
#11804 = DIRECTION ( 'NONE',  ( 0.000000000000000000, 0.000000000000000000, 1.000000000000000000 ) ) ;
#11805 = AXIS2_PLACEMENT_3D ( 'NONE', #5536, #3478, #5844 ) ;
#11806 = ORIENTED_EDGE ( 'NONE', *, *, #30479, .T. ) ;
#11807 = VECTOR ( 'NONE', #25858, 1000.000000000000114 ) ;
#11808 = ORIENTED_EDGE ( 'NONE', *, *, #21725, .T. ) ;
#11809 = CARTESIAN_POINT ( 'NONE',  ( 58.72973946704998127, 0.5000000000006151746, -1.835413506853449395 ) ) ;
#11810 = VERTEX_POINT ( 'NONE', #16136 ) ;
#11811 = CARTESIAN_POINT ( 'NONE',  ( 56.95000000000001705, 0.000000000000000000, -1.899999999999999911 ) ) ;
#11812 = CARTESIAN_POINT ( 'NONE',  ( -56.54792740578360366, 3.330682475591790315, 0.6830477631804106053 ) ) ;
#11814 = CARTESIAN_POINT ( 'NONE',  ( 50.80000000000001847, -3.937842575352405117, -1.145831896685998830 ) ) ;
#11813 = FACE_OUTER_BOUND ( 'NONE', #25033, .T. ) ;
#11815 = ORIENTED_EDGE ( 'NONE', *, *, #6365, .F. ) ;
#11816 = ORIENTED_EDGE ( 'NONE', *, *, #14041, .T. ) ;
#11817 = CARTESIAN_POINT ( 'NONE',  ( 22.26297291748177898, 7.344068067229269303, -2.050000000000077094 ) ) ;
#11818 = ORIENTED_EDGE ( 'NONE', *, *, #6230, .T. ) ;
#11819 = LINE ( 'NONE', #6281, #10504 ) ;
#11820 = EDGE_LOOP ( 'NONE', ( #14618, #21618, #13125, #9766, #14794 ) ) ;
#11822 = CARTESIAN_POINT ( 'NONE',  ( -35.85663232820584057, 4.945493884734801782, -1.606888370749687933 ) ) ;
#11821 = CARTESIAN_POINT ( 'NONE',  ( 50.50000000000001421, 0.6462379109120994780, 4.048750000000022276 ) ) ;
#11823 = ORIENTED_EDGE ( 'NONE', *, *, #17334, .F. ) ;
#11824 = CARTESIAN_POINT ( 'NONE',  ( 52.10571136498352018, 8.590619605527507474, 1.949999390375997343 ) ) ;
#11825 = CARTESIAN_POINT ( 'NONE',  ( 57.03513260258041839, 0.7477432062408043700, 1.780365573899210574 ) ) ;
#11826 = CARTESIAN_POINT ( 'NONE',  ( -54.48531357662248809, -1.514292094527452504, -3.309285685900293483 ) ) ;
#11827 = CARTESIAN_POINT ( 'NONE',  ( -59.63860681421865451, 2.978809096019410685, 1.643800408120751566 ) ) ;
#11828 = CARTESIAN_POINT ( 'NONE',  ( -57.63452994616205416, -3.117691453623976816, 1.799999999999783329 ) ) ;
#11829 = LINE ( 'NONE', #18659, #23606 ) ;
#11830 = EDGE_CURVE ( 'NONE', #26302, #24008, #4412, .T. ) ;
#11831 = EDGE_CURVE ( 'NONE', #21960, #2526, #490, .T. ) ;
#11832 = EDGE_CURVE ( 'NONE', #13515, #22777, #24259, .T. ) ;
#11833 = CARTESIAN_POINT ( 'NONE',  ( -54.44999999999997442, 1.499999999999999556, -4.029888335921975262 ) ) ;
#11834 = DIRECTION ( 'NONE',  ( 0.000000000000000000, -0.9996898646859343485, -0.02490330187381123786 ) ) ;
#11835 = CARTESIAN_POINT ( 'NONE',  ( 57.00000000000001421, -0.7500000000000000000, 3.499999999999999556 ) ) ;
#11836 =( BOUNDED_CURVE ( )  B_SPLINE_CURVE ( 2, ( #18974, #2168, #26547, #26402, #6767, #14353, #13866, #11530, #21363 ),
 .UNSPECIFIED., .F., .T. ) 
 B_SPLINE_CURVE_WITH_KNOTS ( ( 3, 2, 2, 2, 3 ),
 ( 0.3055555555555555802, 0.3148148148148148251, 0.3333333333333333148, 0.3518518518518518601, 0.3611111111111111049 ),
 .UNSPECIFIED. ) 
 CURVE ( )  GEOMETRIC_REPRESENTATION_ITEM ( )  RATIONAL_B_SPLINE_CURVE ( ( 0.9330127018922194093, 0.9330127018922195203, 1.000000000000000000, 0.8660254037844387076, 1.000000000000000000, 0.8660254037844387076, 1.000000000000000000, 0.9330127018922194093, 0.9330127018922194093 ) ) 
 REPRESENTATION_ITEM ( '' )  );
#11837 = CARTESIAN_POINT ( 'NONE',  ( -35.85663232820584057, -1.123735532908286316, 5.289358697221548944 ) ) ;
#11838 = ORIENTED_EDGE ( 'NONE', *, *, #14924, .F. ) ;
#11839 = CARTESIAN_POINT ( 'NONE',  ( 50.25000000000004263, -1.895722432252775924, -0.6373668173469783094 ) ) ;
#11840 = CARTESIAN_POINT ( 'NONE',  ( -36.63359589171323449, 0.7811288459610937762, 5.350925378100968466 ) ) ;
#11841 = CARTESIAN_POINT ( 'NONE',  ( 53.96114084830844604, 6.379385664344251694, 1.889910665294559422 ) ) ;
#11842 = ORIENTED_EDGE ( 'NONE', *, *, #8184, .T. ) ;
#11843 = EDGE_CURVE ( 'NONE', #15867, #704, #19624, .T. ) ;
#11844 = CARTESIAN_POINT ( 'NONE',  ( 68.00000000000004263, -0.8382352941176474115, 2.222158093316569438 ) ) ;
#11845 = ORIENTED_EDGE ( 'NONE', *, *, #10051, .T. ) ;
#11846 = AXIS2_PLACEMENT_3D ( 'NONE', #23894, #24042, #19164 ) ;
#11848 = DIRECTION ( 'NONE',  ( 0.000000000000000000, -1.000000000000000000, -0.000000000000000000 ) ) ;
#11847 = CARTESIAN_POINT ( 'NONE',  ( 58.65000045311411014, 1.008695754911338227, -1.580645149930956617 ) ) ;
#11849 = VERTEX_POINT ( 'NONE', #21988 ) ;
#11850 = DIRECTION ( 'NONE',  ( -0.000000000000000000, 1.000000000000000000, 3.491481338843133355E-15 ) ) ;
#11851 = DIRECTION ( 'NONE',  ( 0.000000000000000000, 0.000000000000000000, -1.000000000000000000 ) ) ;
#11853 = FACE_OUTER_BOUND ( 'NONE', #15251, .T. ) ;
#11852 = DIRECTION ( 'NONE',  ( 0.000000000000000000, 0.000000000000000000, 1.000000000000000000 ) ) ;
#11854 = VERTEX_POINT ( 'NONE', #7574 ) ;
#11855 = CARTESIAN_POINT ( 'NONE',  ( -60.79792740578359656, -2.256877952708263635, 2.542931754211925188 ) ) ;
#11856 = AXIS2_PLACEMENT_3D ( 'NONE', #26279, #28340, #2199 ) ;
#11857 = CARTESIAN_POINT ( 'NONE',  ( 61.24473505568541754, 0.9276313280772279235, 1.700547749641277084 ) ) ;
#11858 = FACE_OUTER_BOUND ( 'NONE', #2905, .T. ) ;
#11859 = CARTESIAN_POINT ( 'NONE',  ( 60.75000000000001421, 0.5000000000006363798, 1.718465885608440047 ) ) ;
#11860 = CARTESIAN_POINT ( 'NONE',  ( -61.35074338551757478, -2.593275822190189039, -0.5912877971683896394 ) ) ;
#11861 = CARTESIAN_POINT ( 'NONE',  ( -59.24999999999997158, -1.184343223768572706, -3.558065644182728082 ) ) ;
#11862 = CARTESIAN_POINT ( 'NONE',  ( -62.09999999999998010, -2.699336478251256111, 0.2304543901385250337 ) ) ;
#11863 = AXIS2_PLACEMENT_3D ( 'NONE', #2625, #17197, #26841 ) ;
#11864 = ORIENTED_EDGE ( 'NONE', *, *, #18991, .T. ) ;
#11865 = EDGE_CURVE ( 'NONE', #7647, #19414, #4876, .T. ) ;
#11866 = CARTESIAN_POINT ( 'NONE',  ( -56.93749999999996447, 0.7533615035078061739, -3.673546848079177973 ) ) ;
#11867 = EDGE_CURVE ( 'NONE', #24179, #21603, #20740, .T. ) ;
#11868 = DIRECTION ( 'NONE',  ( -4.275831445896958607E-31, 1.000000000000000000, -1.224646799147353207E-16 ) ) ;
#11869 = CARTESIAN_POINT ( 'NONE',  ( 56.95000000000001705, 0.000000000000000000, 0.000000000000000000 ) ) ;
#11870 = AXIS2_PLACEMENT_3D ( 'NONE', #1069, #8340, #18013 ) ;
#11871 = CARTESIAN_POINT ( 'NONE',  ( 27.72596399900197994, 5.416480400817087038, -1.950000000000096101 ) ) ;
#11872 = CARTESIAN_POINT ( 'NONE',  ( -74.38999999999998636, 1.239615432210556367, 0.03088009432353080660 ) ) ;
#11873 = CIRCLE ( 'NONE', #31078, 1.975000000000001865 ) ;
#11875 = DIRECTION ( 'NONE',  ( 0.000000000000000000, 0.000000000000000000, 1.000000000000000000 ) ) ;
#11874 = CARTESIAN_POINT ( 'NONE',  ( -61.84504909419678143, -2.680454941414578851, 0.3368274758861355966 ) ) ;
#11876 = CARTESIAN_POINT ( 'NONE',  ( 47.76174270024939261, -4.379902212273319329, -1.406632791261494653 ) ) ;
#11878 = DIRECTION ( 'NONE',  ( 1.000000000000000000, -0.000000000000000000, -1.047444401652940007E-14 ) ) ;
#11877 = FACE_OUTER_BOUND ( 'NONE', #23617, .T. ) ;
#11879 = ORIENTED_EDGE ( 'NONE', *, *, #9839, .F. ) ;
#11880 = ADVANCED_FACE ( 'NONE', ( #27195 ), #16186, .T. ) ;
#11881 = CARTESIAN_POINT ( 'NONE',  ( 34.50000000000001421, 3.918869757271530460E-16, 3.200000000000000178 ) ) ;
#11882 = CARTESIAN_POINT ( 'NONE',  ( 54.22146708689643191, 6.361260388417356637, -2.050000000000189004 ) ) ;
#11884 = CARTESIAN_POINT ( 'NONE',  ( -36.58361892165972762, 5.175840503946175453, 1.569056257078830008 ) ) ;
#11883 = CARTESIAN_POINT ( 'NONE',  ( 51.84772254680354564, -0.6924618999061498137, -1.653428777428161300 ) ) ;
#11885 = CARTESIAN_POINT ( 'NONE',  ( 15.03925126672133494, -4.683225679163354194, 2.703237727951214975 ) ) ;
#11886 = ORIENTED_EDGE ( 'NONE', *, *, #20186, .F. ) ;
#11887 = AXIS2_PLACEMENT_3D ( 'NONE', #11169, #11310, #8632 ) ;
#11888 = EDGE_LOOP ( 'NONE', ( #2672, #13049, #1845, #3462 ) ) ;
#11889 = CARTESIAN_POINT ( 'NONE',  ( 51.45655683570189609, 0.9591657938401617622, -1.468576096419531352 ) ) ;
#11890 = EDGE_LOOP ( 'NONE', ( #10441, #3001, #19473, #17139 ) ) ;
#11891 = CARTESIAN_POINT ( 'NONE',  ( 57.05000000000001847, 0.8156862745098041323, -2.468735688885368873 ) ) ;
#11892 = AXIS2_PLACEMENT_3D ( 'NONE', #11466, #11291, #27621 ) ;
#11893 = CARTESIAN_POINT ( 'NONE',  ( 56.95000000000001705, -0.7000000000000000666, -2.452039967047845437 ) ) ;
#11894 = EDGE_LOOP ( 'NONE', ( #3371, #15312, #14652, #13153 ) ) ;
#11895 = CARTESIAN_POINT ( 'NONE',  ( 51.31572262954152563, 1.002608958138273554, -1.996089927833914146 ) ) ;
#11896 = ORIENTED_EDGE ( 'NONE', *, *, #16016, .T. ) ;
#11897 = CARTESIAN_POINT ( 'NONE',  ( -60.83155989232411542, 3.925981830489463142, -2.015755723410760408E-13 ) ) ;
#11898 = ORIENTED_EDGE ( 'NONE', *, *, #10892, .T. ) ;
#11899 = AXIS2_PLACEMENT_3D ( 'NONE', #26429, #28492, #9186 ) ;
#11900 = VERTEX_POINT ( 'NONE', #27022 ) ;
#11901 = VERTEX_POINT ( 'NONE', #22303 ) ;
#11902 = ADVANCED_FACE ( 'NONE', ( #5035 ), #30382, .T. ) ;
#11903 = CARTESIAN_POINT ( 'NONE',  ( -59.18749999999996447, -3.925981830489445379, -2.242119407191119848E-13 ) ) ;
#11904 = LINE ( 'NONE', #11266, #1917 ) ;
#11905 = CARTESIAN_POINT ( 'NONE',  ( 58.45000000000001705, -0.8000000000000002665, -2.421260002560650104 ) ) ;
#11907 = ADVANCED_FACE ( 'NONE', ( #2518 ), #24495, .T. ) ;
#11906 = CYLINDRICAL_SURFACE ( 'NONE', #27588, 4.700000000000000178 ) ;
#11908 = AXIS2_PLACEMENT_3D ( 'NONE', #18084, #1264, #3798 ) ;
#11909 = CARTESIAN_POINT ( 'NONE',  ( -58.06684846062112371, -0.2309624077929089692, -3.875409454552789512 ) ) ;
#11910 = VECTOR ( 'NONE', #12534, 999.9999999999998863 ) ;
#11912 = DIRECTION ( 'NONE',  ( -1.000000000000000000, -2.586136946169074517E-16, 0.000000000000000000 ) ) ;
#11911 = CARTESIAN_POINT ( 'NONE',  ( 68.95000000000003126, 1.401298464324817071E-42, -7.222129149397022450E-13 ) ) ;
#11913 = AXIS2_PLACEMENT_3D ( 'NONE', #23914, #9524, #16647 ) ;
#11914 = CARTESIAN_POINT ( 'NONE',  ( -58.43749999999997158, -3.399999999999991029, -2.253785087031484148E-13 ) ) ;
#11915 = DIRECTION ( 'NONE',  ( 1.000000000000000000, 4.939082069373447378E-17, 1.520093157366847861E-16 ) ) ;
#11916 = CARTESIAN_POINT ( 'NONE',  ( -44.49999999999997868, -6.938893903907228378E-14, 0.000000000000000000 ) ) ;
#11917 = ORIENTED_EDGE ( 'NONE', *, *, #26043, .F. ) ;
#11918 = ADVANCED_FACE ( 'NONE', ( #24811 ), #29102, .F. ) ;
#11919 = DIRECTION ( 'NONE',  ( 0.000000000000000000, 0.2008964009354141933, -0.9796124928211140670 ) ) ;
#11920 = CIRCLE ( 'NONE', #10917, 4.650000000000000355 ) ;
#11921 = CARTESIAN_POINT ( 'NONE',  ( -60.59999999999997300, -2.476825173781434852, 0.9422510591782664591 ) ) ;
#11923 = DIRECTION ( 'NONE',  ( 1.000000000000000000, -1.219044193948983948E-29, 3.491481338843133355E-15 ) ) ;
#11922 = CARTESIAN_POINT ( 'NONE',  ( 48.39258289184584783, -1.342093792059618762, 3.874237195466570416 ) ) ;
#11924 = CARTESIAN_POINT ( 'NONE',  ( 54.27565932475310717, 6.003153976823456972, -2.050000000000189893 ) ) ;
#11925 = CARTESIAN_POINT ( 'NONE',  ( 50.80000000000001847, -3.908336260473453727, -1.238913909466097474 ) ) ;
#11926 = VERTEX_POINT ( 'NONE', #589 ) ;
#11927 = DIRECTION ( 'NONE',  ( 0.000000000000000000, 0.000000000000000000, 1.000000000000000000 ) ) ;
#11928 = CARTESIAN_POINT ( 'NONE',  ( 58.75000000000000711, 1.800471618824943221, -1.039502773795712987 ) ) ;
#11929 = CARTESIAN_POINT ( 'NONE',  ( -55.63452994616205416, 3.117691453623979481, 1.799999999999814415 ) ) ;
#11930 = ORIENTED_EDGE ( 'NONE', *, *, #12981, .F. ) ;
#11931 = EDGE_CURVE ( 'NONE', #30450, #16732, #23265, .T. ) ;
#11932 = ORIENTED_EDGE ( 'NONE', *, *, #18532, .T. ) ;
#11933 = AXIS2_PLACEMENT_3D ( 'NONE', #25154, #22324, #8063 ) ;
#11934 = CARTESIAN_POINT ( 'NONE',  ( 15.86395258069111414, 4.872718122832685239, 2.345308583460563590 ) ) ;
#11935 = EDGE_LOOP ( 'NONE', ( #22188, #10854 ) ) ;
#11936 = TOROIDAL_SURFACE ( 'NONE', #2817, 4.275000000000000355, 0.1000000000000000056 ) ;
#11937 = CARTESIAN_POINT ( 'NONE',  ( 51.87992451262095983, 4.432176970433021168, -1.232860998884740766 ) ) ;
#11938 = CARTESIAN_POINT ( 'NONE',  ( -58.44702994616205416, -2.078460969082657872, 3.599999999999784261 ) ) ;
#11939 = ORIENTED_EDGE ( 'NONE', *, *, #13248, .T. ) ;
#11940 = DIRECTION ( 'NONE',  ( 0.000000000000000000, 0.000000000000000000, -1.000000000000000000 ) ) ;
#11941 = CARTESIAN_POINT ( 'NONE',  ( 51.49472959044967268, -1.070956530527746864, 1.224612562803249594 ) ) ;
#11942 = AXIS2_PLACEMENT_3D ( 'NONE', #2170, #21683, #21511 ) ;
#11943 = CARTESIAN_POINT ( 'NONE',  ( 30.17828911090722954, 6.795520168002859407, 2.049999999999894129 ) ) ;
#11944 = ORIENTED_EDGE ( 'NONE', *, *, #16853, .F. ) ;
#11945 = VECTOR ( 'NONE', #7355, 1000.000000000000114 ) ;
#11946 = CIRCLE ( 'NONE', #29145, 2.624999999999998668 ) ;
#11947 = EDGE_CURVE ( 'NONE', #24689, #6742, #24765, .T. ) ;
#11948 = DIRECTION ( 'NONE',  ( -1.000000000000000000, -3.053848253006669023E-16, 2.042510438544995415E-16 ) ) ;
#11949 = AXIS2_PLACEMENT_3D ( 'NONE', #7644, #17304, #24735 ) ;
#11950 = EDGE_CURVE ( 'NONE', #30600, #19284, #25229, .T. ) ;
#11951 = DIRECTION ( 'NONE',  ( 0.000000000000000000, -0.9996898646859343485, -0.02490330187381124133 ) ) ;
#11952 = CARTESIAN_POINT ( 'NONE',  ( 58.72204580543405683, -0.9570475208903724829, -1.612507782425579350 ) ) ;
#11953 = VERTEX_POINT ( 'NONE', #14693 ) ;
#11955 = EDGE_CURVE ( 'NONE', #8932, #16106, #27297, .T. ) ;
#11954 = CARTESIAN_POINT ( 'NONE',  ( -44.59999999999998010, 8.366749974758271452E-15, -1.593320673368357319E-13 ) ) ;
#11956 = CARTESIAN_POINT ( 'NONE',  ( 56.95442145253466038, 0.7107037530308675244, 1.762072693003282398 ) ) ;
#11957 = AXIS2_PLACEMENT_3D ( 'NONE', #4612, #23632, #4459 ) ;
#11959 = DIRECTION ( 'NONE',  ( 1.000000000000000000, 0.000000000000000000, -0.000000000000000000 ) ) ;
#11958 = CARTESIAN_POINT ( 'NONE',  ( -35.85663232820584057, -1.793057972832186486, -4.026191436122056544 ) ) ;
#11960 = AXIS2_PLACEMENT_3D ( 'NONE', #13078, #10236, #22602 ) ;
#11961 = DIRECTION ( 'NONE',  ( 1.000000000000000000, 3.053848253006669023E-16, -2.042510438544995415E-16 ) ) ;
#11962 = DIRECTION ( 'NONE',  ( 1.000000000000000000, -0.000000000000000000, -0.000000000000000000 ) ) ;
#11964 = CARTESIAN_POINT ( 'NONE',  ( 53.49139514279642782, 5.155866831720373966, 1.635615235160198466 ) ) ;
#11963 = CIRCLE ( 'NONE', #29646, 2.000000000000000000 ) ;
#11965 = ORIENTED_EDGE ( 'NONE', *, *, #17328, .T. ) ;
#11966 = VECTOR ( 'NONE', #9928, 1000.000000000000000 ) ;
#11967 = VERTEX_POINT ( 'NONE', #3736 ) ;
#11968 = CARTESIAN_POINT ( 'NONE',  ( 58.66324791596939292, 0.5000000000006143974, -1.807104036850105677 ) ) ;
#11969 = ORIENTED_EDGE ( 'NONE', *, *, #30124, .T. ) ;
#11970 =( GEOMETRIC_REPRESENTATION_CONTEXT ( 3 ) GLOBAL_UNCERTAINTY_ASSIGNED_CONTEXT ( ( #9534 ) ) GLOBAL_UNIT_ASSIGNED_CONTEXT ( ( #24603, #391, #85 ) ) REPRESENTATION_CONTEXT ( 'NONE', 'WORKASPACE' ) );
#11971 = CARTESIAN_POINT ( 'NONE',  ( 50.30000000000001847, 1.426739617975221641, -3.843750000000023093 ) ) ;
#11972 = CARTESIAN_POINT ( 'NONE',  ( -55.98542740578361077, 0.7887156198831667409, -3.845940847736174728 ) ) ;
#11974 = DIRECTION ( 'NONE',  ( -0.4772254810013855097, 0.8787808829753843698, 1.772289120718281137E-15 ) ) ;
#11973 = FACE_OUTER_BOUND ( 'NONE', #12806, .T. ) ;
#11975 = EDGE_LOOP ( 'NONE', ( #14358, #7740, #5118, #12478 ) ) ;
#11976 = EDGE_CURVE ( 'NONE', #12204, #21976, #3534, .T. ) ;
#11977 = ORIENTED_EDGE ( 'NONE', *, *, #5080, .F. ) ;
#11978 = CARTESIAN_POINT ( 'NONE',  ( 58.65000000000001990, 6.143261415694495821E-13, 3.111507638930570854E-58 ) ) ;
#11979 = ORIENTED_EDGE ( 'NONE', *, *, #11447, .F. ) ;
#11980 = DIRECTION ( 'NONE',  ( -1.000000000000000000, -3.053848253006669023E-16, 2.042510438544995415E-16 ) ) ;
#11981 = VERTEX_POINT ( 'NONE', #20246 ) ;
#11982 = CARTESIAN_POINT ( 'NONE',  ( -54.39999999999999147, -1.400000000000006795, 3.959797974644448715 ) ) ;
#11983 = EDGE_CURVE ( 'NONE', #28572, #5002, #21775, .T. ) ;
#11984 = VERTEX_POINT ( 'NONE', #30021 ) ;
#11985 = B_SPLINE_CURVE_WITH_KNOTS ( 'NONE', 3,
 ( #29314, #22043, #24404, #27080, #29162, #341, #9704, #26790, #22204, #4769, #5400, #15058 ),
 .UNSPECIFIED., .F., .F.,
 ( 4, 2, 2, 2, 2, 4 ),
 ( 0.000000000000000000, 5.522938194211708289E-05, 0.0001104587638842341658, 0.0002209175277684793091, 0.0004418350555369705986, 0.0008836701110739516056 ),
 .UNSPECIFIED. ) ;
#11986 = CARTESIAN_POINT ( 'NONE',  ( -59.36488781976483864, 2.508594352967818963, -1.045061501994789976 ) ) ;
#11987 = VECTOR ( 'NONE', #16144, 1000.000000000000000 ) ;
#11988 = VECTOR ( 'NONE', #10818, 1000.000000000000000 ) ;
#11989 = CARTESIAN_POINT ( 'NONE',  ( 50.25000000000000000, 2.079005547593327119, 1.004182178118534636E-12 ) ) ;
#11990 = AXIS2_PLACEMENT_3D ( 'NONE', #16619, #2517, #31002 ) ;
#11991 = AXIS2_PLACEMENT_3D ( 'NONE', #19793, #24687, #19649 ) ;
#11992 = DIRECTION ( 'NONE',  ( 0.000000000000000000, 0.000000000000000000, 1.000000000000000000 ) ) ;
#11993 = CARTESIAN_POINT ( 'NONE',  ( -60.75952994616205416, -4.643455692769856999E-15, 3.599999999999783373 ) ) ;
#11994 = CARTESIAN_POINT ( 'NONE',  ( -59.16607095580928899, -2.501426125405462386, -0.9458072644521190453 ) ) ;
#11995 = VECTOR ( 'NONE', #30029, 1000.000000000000000 ) ;
#11996 = TOROIDAL_SURFACE ( 'NONE', #15947, 4.000000000000022204, 0.1000000000000000056 ) ;
#11997 = CIRCLE ( 'NONE', #27680, 0.05000000000000002359 ) ;
#11999 = CIRCLE ( 'NONE', #9478, 0.1500000000000001887 ) ;
#11998 = CARTESIAN_POINT ( 'NONE',  ( 58.65000000000001279, 0.5539202450380567022, 1.791540873398024036 ) ) ;
#12000 =( BOUNDED_SURFACE ( )  B_SPLINE_SURFACE ( 3, 2, ( 
 ( #15468, #8647, #17703 ),
 ( #25124, #1207, #18327 ),
 ( #10866, #27348, #3280 ),
 ( #743, #10404, #15311 ),
 ( #20085, #8036, #24956 ),
 ( #6746, #28121, #19120 ),
 ( #11665, #13553, #28765 ),
 ( #20859, #26059, #18800 ),
 ( #21189, #6444, #14018 ),
 ( #9136, #11814, #13847 ) ),
 .UNSPECIFIED., .F., .F., .T. ) 
 B_SPLINE_SURFACE_WITH_KNOTS ( ( 4, 2, 2, 2, 4 ),
 ( 3, 3 ),
 ( -1.029992063861229212E-18, 0.0003537660104434870454, 0.0007075320208869751749, 0.001061298031330463413, 0.001415064041773951434 ),
 ( 0.000000000000000000, 1.000000000000000000 ),
 .UNSPECIFIED. ) 
 GEOMETRIC_REPRESENTATION_ITEM ( )  RATIONAL_B_SPLINE_SURFACE ( (
 ( 1.000000000000000000, 0.7071067811865712205, 1.000000000000000000),
 ( 1.000000000000000000, 0.7179295922952823039, 1.000000000000000000),
 ( 1.000000000000000000, 0.7246425758715334675, 1.000000000000000000),
 ( 1.000000000000000000, 0.7309548279203578192, 1.000000000000000000),
 ( 1.000000000000000000, 0.7305336397956169181, 1.000000000000000000),
 ( 1.000000000000000000, 0.7264835597194815309, 1.000000000000000000),
 ( 1.000000000000000000, 0.7229248932012791728, 1.000000000000000000),
 ( 1.000000000000000000, 0.7174039707101230734, 1.000000000000000000),
 ( 1.000000000000000000, 0.7154085637344075321, 1.000000000000000000),
 ( 1.000000000000000000, 0.7154752000627011554, 1.000000000000000000) ) ) 
 REPRESENTATION_ITEM ( '' )  SURFACE ( )  );
#12001 = DIRECTION ( 'NONE',  ( -1.000000000000000000, 0.000000000000000000, 1.047444401652940007E-14 ) ) ;
#12002 = CARTESIAN_POINT ( 'NONE',  ( -59.52807307762599720, -2.290451074298654799, 1.439549604813781913 ) ) ;
#12003 = DIRECTION ( 'NONE',  ( 0.000000000000000000, 0.000000000000000000, -1.000000000000000000 ) ) ;
#12004 = EDGE_LOOP ( 'NONE', ( #781, #22924, #26536, #28224 ) ) ;
#12005 = LINE ( 'NONE', #18980, #21482 ) ;
#12006 = CIRCLE ( 'NONE', #20609, 0.2500000000000000000 ) ;
#12007 = CARTESIAN_POINT ( 'NONE',  ( 58.65000000000000568, 1.394635017529600507, -1.253243060177047896 ) ) ;
#12008 = CARTESIAN_POINT ( 'NONE',  ( 53.90845325060750071, 6.078717535930443283, 0.8364386040616162976 ) ) ;
#12009 = VERTEX_POINT ( 'NONE', #20555 ) ;
#12010 = CARTESIAN_POINT ( 'NONE',  ( -54.45487361440510909, 1.499999999999999556, 4.029888335921975262 ) ) ;
#12011 = CIRCLE ( 'NONE', #16048, 0.09999999999999990841 ) ;
#12012 = ORIENTED_EDGE ( 'NONE', *, *, #10268, .F. ) ;
#12013 = CARTESIAN_POINT ( 'NONE',  ( 15.76675455518219593, -0.1030603059131519339, -5.407440145940146436 ) ) ;
#12015 = DIRECTION ( 'NONE',  ( -1.000000000000000000, 0.000000000000000000, 0.000000000000000000 ) ) ;
#12014 = CARTESIAN_POINT ( 'NONE',  ( 58.72427158855710161, 0.8981388483285237534, -1.646019958201040190 ) ) ;
#12016 = ORIENTED_EDGE ( 'NONE', *, *, #24316, .F. ) ;
#12017 = EDGE_CURVE ( 'NONE', #7673, #19795, #21248, .T. ) ;
#12018 = CARTESIAN_POINT ( 'NONE',  ( 51.25000000000002842, -1.099999999999459410, 1.001327244211406953 ) ) ;
#12019 = EDGE_CURVE ( 'NONE', #10802, #20370, #20399, .T. ) ;
#12020 = VECTOR ( 'NONE', #28163, 1000.000000000000000 ) ;
#12021 = DIRECTION ( 'NONE',  ( -1.510019896901732094E-45, -1.000000000000000000, -3.491481338843132566E-15 ) ) ;
#12022 = CIRCLE ( 'NONE', #6462, 0.1500000000000003830 ) ;
#12024 = CARTESIAN_POINT ( 'NONE',  ( 58.74999999305995857, 0.9867593359915998175, 1.657788420846524557 ) ) ;
#12023 = DIRECTION ( 'NONE',  ( 1.000000000000000000, 3.053848253006669023E-16, -2.042510438544995415E-16 ) ) ;
#12025 = EDGE_CURVE ( 'NONE', #16439, #12125, #29878, .T. ) ;
#12026 = ORIENTED_EDGE ( 'NONE', *, *, #6616, .F. ) ;
#12027 = CARTESIAN_POINT ( 'NONE',  ( -54.62499999999997868, 2.489203624310591501, -2.804704140674918467 ) ) ;
#12028 = DIRECTION ( 'NONE',  ( 0.000000000000000000, 0.000000000000000000, -1.000000000000000000 ) ) ;
#12029 = DIRECTION ( 'NONE',  ( 1.168655815394902336E-14, 3.552713678800500929E-15, 1.000000000000000000 ) ) ;
#12030 = CARTESIAN_POINT ( 'NONE',  ( -44.49999999999996447, 1.500000000000021538, -3.363870538531645416 ) ) ;
#12031 = CARTESIAN_POINT ( 'NONE',  ( -44.59999999999996589, 1.400000000000023670, -3.959797974644836405 ) ) ;
#12032 = CARTESIAN_POINT ( 'NONE',  ( -57.87499999999997868, -1.933093229062082319E-14, 3.399999999999793854 ) ) ;
#12033 = DIRECTION ( 'NONE',  ( -1.168655815394902336E-14, 0.000000000000000000, -1.000000000000000000 ) ) ;
#12034 = AXIS2_PLACEMENT_3D ( 'NONE', #28054, #28706, #23469 ) ;
#12035 = VERTEX_POINT ( 'NONE', #13379 ) ;
#12036 = CIRCLE ( 'NONE', #6448, 0.09999999999999982514 ) ;
#12037 = ADVANCED_FACE ( 'NONE', ( #15925 ), #10600, .F. ) ;
#12038 =( BOUNDED_SURFACE ( )  B_SPLINE_SURFACE ( 3, 2, ( 
 ( #15228, #984, #12685 ),
 ( #5724, #22365, #8252 ),
 ( #15546, #27733, #17772 ),
 ( #20160, #25199, #3515 ),
 ( #8409, #18090, #6052 ),
 ( #3656, #13292, #10165 ),
 ( #29464, #7780, #29624 ),
 ( #17447, #655, #17615 ),
 ( #27260, #5578, #24874 ),
 ( #12832, #18390, #8562 ) ),
 .UNSPECIFIED., .F., .F., .F. ) 
 B_SPLINE_SURFACE_WITH_KNOTS ( ( 4, 2, 2, 2, 4 ),
 ( 3, 3 ),
 ( 0.0002526260074104870901, 0.0003606909493797115550, 0.0004687558913489359657, 0.0006848857752873848412, 0.001117145543164282592 ),
 ( 0.000000000000000000, 1.000000000000000000 ),
 .UNSPECIFIED. ) 
 GEOMETRIC_REPRESENTATION_ITEM ( )  RATIONAL_B_SPLINE_SURFACE ( (
 ( 1.000000000000000000, 0.9842509842511785179, 1.000000000000000000),
 ( 1.000000000000000000, 0.9838268088398964828, 1.000000000000000000),
 ( 1.000000000000000000, 0.9731519947952215199, 1.000000000000000000),
 ( 1.000000000000000000, 0.9499473078865533493, 1.000000000000000000),
 ( 1.000000000000000000, 0.9371632344323691521, 1.000000000000000000),
 ( 1.000000000000000000, 0.8981767195495000689, 1.000000000000000000),
 ( 1.000000000000000000, 0.8714317066438477255, 1.000000000000000000),
 ( 1.000000000000000000, 0.7945716934681549271, 1.000000000000000000),
 ( 1.000000000000000000, 0.7462340517456440558, 1.000000000000000000),
 ( 1.000000000000000000, 0.7071067811865505703, 1.000000000000000000) ) ) 
 REPRESENTATION_ITEM ( '' )  SURFACE ( )  );
#12039 = AXIS2_PLACEMENT_3D ( 'NONE', #16904, #28783, #28463 ) ;
#12040 = CARTESIAN_POINT ( 'NONE',  ( 15.98305126557428935, -3.597789892641458209, 4.037455662930108602 ) ) ;
#12041 = CARTESIAN_POINT ( 'NONE',  ( -69.19999999999998863, 0.4218824419643700252, -2.057186234924337054 ) ) ;
#12042 = DIRECTION ( 'NONE',  ( -1.000000000000000000, -0.000000000000000000, 0.000000000000000000 ) ) ;
#12043 = FACE_OUTER_BOUND ( 'NONE', #4494, .T. ) ;
#12045 = CARTESIAN_POINT ( 'NONE',  ( 51.87416143049283335, 8.598705507415685290, -1.950000000000180256 ) ) ;
#12044 = CARTESIAN_POINT ( 'NONE',  ( 57.00000000000001421, 0.7500000000000000000, 1.778341924377873751 ) ) ;
#12046 = PRODUCT_RELATED_PRODUCT_CATEGORY ( 'part', '', ( #8054 ) ) ;
#12047 = CARTESIAN_POINT ( 'NONE',  ( 61.24504608472945932, -0.9290853280804240999, 1.697615787671056697 ) ) ;
#12049 = CARTESIAN_POINT ( 'NONE',  ( 22.25735896772343025, 7.137076052088948686, 1.424999999999921885 ) ) ;
#12048 = DIRECTION ( 'NONE',  ( -1.000000000000000000, -3.054025858079668409E-16, 2.042474015755241579E-16 ) ) ;
#12050 = ORIENTED_EDGE ( 'NONE', *, *, #29281, .F. ) ;
#12051 = CARTESIAN_POINT ( 'NONE',  ( -44.49999999999998579, 2.395752775956332847, 1.350136525132600296 ) ) ;
#12052 = UNCERTAINTY_MEASURE_WITH_UNIT (LENGTH_MEASURE( 1.000000000000000082E-05 ), #25837, 'distance_accuracy_value', 'NONE');
#12053 = CARTESIAN_POINT ( 'NONE',  ( -59.69999999999997442, -3.399999999999991473, -2.235080921937235780E-13 ) ) ;
#12055 = CARTESIAN_POINT ( 'NONE',  ( -36.92362342067168868, 5.192953935288548095, 1.516181439821858268 ) ) ;
#12054 = CARTESIAN_POINT ( 'NONE',  ( 15.61033468494288279, -2.777216423308003002, -4.646230875016937212 ) ) ;
#12056 = DIRECTION ( 'NONE',  ( -1.000000000000000000, -0.000000000000000000, -0.000000000000000000 ) ) ;
#12057 = ORIENTED_EDGE ( 'NONE', *, *, #23521, .F. ) ;
#12058 = VERTEX_POINT ( 'NONE', #12926 ) ;
#12059 = CARTESIAN_POINT ( 'NONE',  ( 58.75000000000000711, 1.039502773797200019, -1.800471618823823450 ) ) ;
#12060 = VECTOR ( 'NONE', #15165, 1000.000000000000000 ) ;
#12061 = ADVANCED_FACE ( 'NONE', ( #30186 ), #10716, .T. ) ;
#12062 = ORIENTED_EDGE ( 'NONE', *, *, #30957, .T. ) ;
#12063 = CARTESIAN_POINT ( 'NONE',  ( 56.96751809705963154, 0.7713737938325972987, -2.482938273535672646 ) ) ;
#12064 = CARTESIAN_POINT ( 'NONE',  ( 58.74472430272347623, 0.5000000000006152856, 1.853787220596809782 ) ) ;
#12065 = EDGE_LOOP ( 'NONE', ( #26134, #20941, #20796, #7365 ) ) ;
#12066 = CARTESIAN_POINT ( 'NONE',  ( -36.38139716712353788, -4.735424960531383398, -2.618558234550535602 ) ) ;
#12067 = EDGE_LOOP ( 'NONE', ( #9341, #6660, #5146, #26521, #20004 ) ) ;
#12068 = PRESENTATION_STYLE_ASSIGNMENT (( #19358 ) ) ;
#12069 = FACE_OUTER_BOUND ( 'NONE', #1149, .T. ) ;
#12070 =( NAMED_UNIT ( * ) PLANE_ANGLE_UNIT ( ) SI_UNIT ( $, .RADIAN. ) );
#12071 = VERTEX_POINT ( 'NONE', #8501 ) ;
#12072 = ORIENTED_EDGE ( 'NONE', *, *, #1847, .F. ) ;
#12073 = EDGE_CURVE ( 'NONE', #19387, #9397, #30342, .T. ) ;
#12074 = CARTESIAN_POINT ( 'NONE',  ( -55.50952994616206126, -4.643455692769921685E-15, 3.599999999999801581 ) ) ;
#12075 = CARTESIAN_POINT ( 'NONE',  ( 53.13060515908006920, 4.213974700431092124, -2.050000000000185008 ) ) ;
#12076 = CARTESIAN_POINT ( 'NONE',  ( 51.70000000000000995, -3.637377585518695611, -2.099877210783217318 ) ) ;
#12077 = CARTESIAN_POINT ( 'NONE',  ( 51.70000000000001705, -4.276948333784438283, -0.9210526315789475671 ) ) ;
#12078 = TOROIDAL_SURFACE ( 'NONE', #425, 1.975000000000001865, 0.1000000000000000056 ) ;
#12079 = CARTESIAN_POINT ( 'NONE',  ( -54.39999999999996305, -1.399999999999979039, -3.959797974644881258 ) ) ;
#12080 = CIRCLE ( 'NONE', #7020, 0.04999999999999991257 ) ;
#12081 = VECTOR ( 'NONE', #7282, 1000.000000000000000 ) ;
#12083 = CARTESIAN_POINT ( 'NONE',  ( -36.58413561666693425, 0.1030603059130986848, -5.407440145940149989 ) ) ;
#12082 = DIRECTION ( 'NONE',  ( 0.000000000000000000, -0.2008964009354147484, 0.9796124928211139560 ) ) ;
#12084 = CARTESIAN_POINT ( 'NONE',  ( 47.03762875446323477, -4.256129153948961630, 1.015733033895002357 ) ) ;
#12085 = CARTESIAN_POINT ( 'NONE',  ( -54.49999999999997868, 1.549999999999999600, 4.064480286580312907 ) ) ;
#12087 = DIRECTION ( 'NONE',  ( -1.000000000000000000, -3.053848253006669023E-16, 2.042510438544995415E-16 ) ) ;
#12086 = CARTESIAN_POINT ( 'NONE',  ( 54.47118315602192951, -0.0009370910484279708656, -4.346120462634435633 ) ) ;
#12088 = EDGE_LOOP ( 'NONE', ( #14260, #19881, #14923, #26410 ) ) ;
#12089 = CARTESIAN_POINT ( 'NONE',  ( 58.75000000000002132, -0.5380862305913116650, 2.008165151418990213 ) ) ;
#12090 = CARTESIAN_POINT ( 'NONE',  ( 47.49416525120574306, -4.280467579807392120, -1.378329539257057368 ) ) ;
#12092 = DIRECTION ( 'NONE',  ( -1.000000000000000000, -3.054025858079668409E-16, 2.042474015755241579E-16 ) ) ;
#12091 = CARTESIAN_POINT ( 'NONE',  ( 48.40000000000002700, -0.7707709757764150682, 3.938803467580344719 ) ) ;
#12093 = CARTESIAN_POINT ( 'NONE',  ( -58.87499999999997158, 1.184343223768566933, 3.558065644182732967 ) ) ;
#12094 = EDGE_LOOP ( 'NONE', ( #28660, #10961, #10357, #22879, #15918 ) ) ;
#12095 = LINE ( 'NONE', #17006, #13935 ) ;
#12096 = EDGE_CURVE ( 'NONE', #3236, #19668, #22918, .T. ) ;
#12097 = VERTEX_POINT ( 'NONE', #3124 ) ;
#12098 = CYLINDRICAL_SURFACE ( 'NONE', #30991, 3.625000000000024869 ) ;
#12099 = CARTESIAN_POINT ( 'NONE',  ( -57.44702994616203284, -2.078460969082631227, -3.600000000000210587 ) ) ;
#12100 = EDGE_LOOP ( 'NONE', ( #6639, #25577, #29441 ) ) ;
#12101 = ORIENTED_EDGE ( 'NONE', *, *, #23940, .F. ) ;
#12102 = CARTESIAN_POINT ( 'NONE',  ( -59.54613710108586844, 3.305219929794498857, -1.149705823355897438 ) ) ;
#12103 = EDGE_LOOP ( 'NONE', ( #13117, #3144, #10645, #7750 ) ) ;
#12104 = AXIS2_PLACEMENT_3D ( 'NONE', #7746, #2698, #12650 ) ;
#12105 = CARTESIAN_POINT ( 'NONE',  ( -55.44702994616206126, -2.078460969082657872, 3.599999999999794920 ) ) ;
#12106 = ORIENTED_EDGE ( 'NONE', *, *, #19645, .F. ) ;
#12107 = DIRECTION ( 'NONE',  ( -8.673617379883787770E-15, 0.000000000000000000, 1.000000000000000000 ) ) ;
#12108 = CARTESIAN_POINT ( 'NONE',  ( 69.25000000000004263, 0.7500000000000000000, 1.988246715072630844 ) ) ;
#12109 = DIRECTION ( 'NONE',  ( -7.637891338979715149E-45, -1.000000000000000000, -3.491481338843131383E-15 ) ) ;
#12110 = ORIENTED_EDGE ( 'NONE', *, *, #16640, .T. ) ;
#12111 = CARTESIAN_POINT ( 'NONE',  ( -44.59999999999996589, -1.399999999999981037, -3.363870538531656962 ) ) ;
#12112 = FACE_OUTER_BOUND ( 'NONE', #2114, .T. ) ;
#12113 = FACE_OUTER_BOUND ( 'NONE', #14471, .T. ) ;
#12114 = AXIS2_PLACEMENT_3D ( 'NONE', #24641, #22287, #23765 ) ;
#12115 = DIRECTION ( 'NONE',  ( 0.000000000000000000, 0.000000000000000000, 1.000000000000000000 ) ) ;
#12116 = CARTESIAN_POINT ( 'NONE',  ( 15.03925126672132961, 2.199885893005992799, -4.939696249117662141 ) ) ;
#12117 = CIRCLE ( 'NONE', #28295, 2.700000000000000178 ) ;
#12119 = CARTESIAN_POINT ( 'NONE',  ( 61.25000000000001421, 1.106298139390920365, -1.666164585742239357 ) ) ;
#12118 = CARTESIAN_POINT ( 'NONE',  ( -35.85663232820597557, -3.779372838781795529, 3.883777296072546736 ) ) ;
#12120 = EDGE_CURVE ( 'NONE', #13545, #1571, #22776, .T. ) ;
#12121 = CARTESIAN_POINT ( 'NONE',  ( 51.70000000000001705, -4.179189514726513899, 0.9999999999999995559 ) ) ;
#12122 = CARTESIAN_POINT ( 'NONE',  ( 51.70000000000001705, -3.826179070414207573, 1.000000000000000222 ) ) ;
#12123 = EDGE_LOOP ( 'NONE', ( #22946, #242, #16331 ) ) ;
#12124 = AXIS2_PLACEMENT_3D ( 'NONE', #24926, #22742, #10688 ) ;
#12125 = VERTEX_POINT ( 'NONE', #5988 ) ;
#12126 = EDGE_CURVE ( 'NONE', #23664, #30343, #13118, .T. ) ;
#12127 = DIRECTION ( 'NONE',  ( -3.489354422748178582E-15, 1.218509414717996338E-16, -1.000000000000000000 ) ) ;
#12128 = ORIENTED_EDGE ( 'NONE', *, *, #24023, .T. ) ;
#12129 = ADVANCED_FACE ( 'NONE', ( #22447 ), #12000, .T. ) ;
#12130 = CARTESIAN_POINT ( 'NONE',  ( 51.80000000000002558, 8.701414213562481237, 2.049999999999819522 ) ) ;
#12131 = CARTESIAN_POINT ( 'NONE',  ( -55.23542740578361077, 0.7887156198831668519, -3.845940847736174728 ) ) ;
#12133 = FACE_OUTER_BOUND ( 'NONE', #29502, .T. ) ;
#12132 = DIRECTION ( 'NONE',  ( 0.000000000000000000, 0.000000000000000000, 1.000000000000000000 ) ) ;
#12134 = EDGE_CURVE ( 'NONE', #19797, #7685, #22779, .T. ) ;
#12135 = VERTEX_POINT ( 'NONE', #30972 ) ;
#12136 = ORIENTED_EDGE ( 'NONE', *, *, #30159, .T. ) ;
#12137 = CARTESIAN_POINT ( 'NONE',  ( -59.19999999999997442, 8.366749974758448157E-15, -2.103076948839454410E-13 ) ) ;
#12138 = ORIENTED_EDGE ( 'NONE', *, *, #3223, .F. ) ;
#12139 = CARTESIAN_POINT ( 'NONE',  ( 30.31473038485998828, 6.776227631128587170, -1.950000000000104983 ) ) ;
#12140 = ORIENTED_EDGE ( 'NONE', *, *, #14158, .F. ) ;
#12141 = CARTESIAN_POINT ( 'NONE',  ( -36.00201293083840426, 5.377732432866750401, 0.5657657256210959495 ) ) ;
#12142 = ORIENTED_EDGE ( 'NONE', *, *, #18936, .F. ) ;
#12143 = CARTESIAN_POINT ( 'NONE',  ( 53.35461118278485770, 7.923754912502171344, 1.887454836110121770 ) ) ;
#12144 = DIRECTION ( 'NONE',  ( 1.000000000000000000, 1.047444401652940007E-14, 0.000000000000000000 ) ) ;
#12145 = VECTOR ( 'NONE', #29724, 1000.000000000000000 ) ;
#12146 = EDGE_CURVE ( 'NONE', #3490, #3082, #30487, .T. ) ;
#12147 = CARTESIAN_POINT ( 'NONE',  ( -59.69999999999998153, 2.914965204491517081, 1.750136525132549137 ) ) ;
#12148 = CARTESIAN_POINT ( 'NONE',  ( -56.76905989232412963, -2.944486372867088697, 1.699999999999787015 ) ) ;
#12149 = CARTESIAN_POINT ( 'NONE',  ( 54.13139471328950236, 5.522381836601891969, -2.050000000000188116 ) ) ;
#12150 = AXIS2_PLACEMENT_3D ( 'NONE', #7800, #22243, #19555 ) ;
#12151 = DIRECTION ( 'NONE',  ( 3.083952846180964840E-15, 0.000000000000000000, 1.000000000000000000 ) ) ;
#12152 = CARTESIAN_POINT ( 'NONE',  ( 50.42118334212123898, 1.311095223031216284, -3.884869838566831657 ) ) ;
#12153 = ADVANCED_FACE ( 'NONE', ( #6599 ), #15220, .T. ) ;
#12154 = CARTESIAN_POINT ( 'NONE',  ( 15.32766723174653656, -4.698774973472838568, -2.676767126782125583 ) ) ;
#12156 = EDGE_CURVE ( 'NONE', #12911, #29967, #1020, .T. ) ;
#12155 = CARTESIAN_POINT ( 'NONE',  ( -60.49999999999995737, 1.963826825011730345E-15, 6.704595576490977020E-16 ) ) ;
#12157 = VERTEX_POINT ( 'NONE', #10066 ) ;
#12158 = CARTESIAN_POINT ( 'NONE',  ( 57.00000000000001421, -0.7000000000000006217, -2.452039967047844993 ) ) ;
#12160 = CARTESIAN_POINT ( 'NONE',  ( 58.66133336607639137, 1.302803168108718879, -1.348863877412651791 ) ) ;
#12159 = CARTESIAN_POINT ( 'NONE',  ( 61.23770293223015670, -0.8897917884444476178, 1.791164585743103999 ) ) ;
#12161 = CARTESIAN_POINT ( 'NONE',  ( 53.81450004168216594, 5.799141575175354113, 1.730551604087905204 ) ) ;
#12162 = VERTEX_POINT ( 'NONE', #14336 ) ;
#12163 = CARTESIAN_POINT ( 'NONE',  ( -36.00197790576392265, -5.377732432866662471, 0.5657657256215433694 ) ) ;
#12164 = VERTEX_POINT ( 'NONE', #4999 ) ;
#12165 = EDGE_CURVE ( 'NONE', #7871, #16027, #9112, .T. ) ;
#12166 = SURFACE_STYLE_USAGE ( .BOTH. , #10099 ) ;
#12167 = CARTESIAN_POINT ( 'NONE',  ( -36.68133364217572989, -4.872718122832729648, 2.345308583460507190 ) ) ;
#12168 = CARTESIAN_POINT ( 'NONE',  ( 51.70000000000000995, -4.020776289669855785, -2.234582293948758736 ) ) ;
#12169 = ADVANCED_FACE ( 'NONE', ( #24460 ), #7681, .F. ) ;
#12170 = EDGE_LOOP ( 'NONE', ( #9838, #28355, #17056, #25535, #6592, #24312, #21279 ) ) ;
#12171 = CARTESIAN_POINT ( 'NONE',  ( -44.59999999999997300, 8.366749974758367693E-15, -1.870876429524646202E-13 ) ) ;
#12172 = LINE ( 'NONE', #7422, #19107 ) ;
#12174 = CARTESIAN_POINT ( 'NONE',  ( -54.49999999999997868, -1.549999999999999600, -4.064480286580312907 ) ) ;
#12173 = CARTESIAN_POINT ( 'NONE',  ( -44.49999999999997868, -0.7497673985144445163, -0.01867747640535983439 ) ) ;
#12175 = ORIENTED_EDGE ( 'NONE', *, *, #11678, .T. ) ;
#12176 = CARTESIAN_POINT ( 'NONE',  ( -59.62499999999997158, 1.184343223768590025, 3.558065644182725862 ) ) ;
#12177 = CARTESIAN_POINT ( 'NONE',  ( 61.24637336955049705, 0.9388313581417159215, 1.688008567905789237 ) ) ;
#12178 = CARTESIAN_POINT ( 'NONE',  ( 51.77437620346577773, -3.759602463706845921, 1.865002073832249252 ) ) ;
#12179 = CARTESIAN_POINT ( 'NONE',  ( -55.37499999999996447, -2.944486372867075819, -1.700000000000208455 ) ) ;
#12180 = FACE_OUTER_BOUND ( 'NONE', #12415, .T. ) ;
#12181 = DIRECTION ( 'NONE',  ( -1.000000000000000000, -0.000000000000000000, -0.000000000000000000 ) ) ;
#12182 =( BOUNDED_SURFACE ( )  B_SPLINE_SURFACE ( 1, 2, ( 
 ( #3218, #14633, #12859, #846, #29818, #2609, #12254, #21939, #222, #9884, #25689, #5751, #20341, #23177, #8588, #1461, #1299, #27757, #11121, #13317, #29968, #15868, #11265, #8276, #20798, #27907, #30278, #30112, #18267, #8887, #15575, #1151, #6075, #13639, #6218, #30427, #16031, #8728, #18415, #10662, #5916, #15401, #1607, #10966, #22864, #27589, #25375, #3678, #25223, #25520, #27438, #3833, #28053, #3541, #13482, #6369, #3995, #23321, #20651, #20946, #17944, #25054, #13177, #30578, #20487, #3384, #13031, #10803, #22715, #23008, #1010, #8434, #18118, #15726, #21283, #11903, #1761, #14123, #30911, #18886, #4619, #2087, #23797, #30756, #40, #21122, #11751, #11602, #23944, #24100, #9065, #31230, #16505, #21425, #9228, #26162, #28703, #28530, #21587, #11432, #31056, #6840, #4469, #2411, #9379, #19048, #18738, #28378, #23643 ),
 ( #19214, #2238, #14279, #9556, #6683, #28855, #7014, #14427, #7168, #6533, #21751, #16678, #13784, #26321, #16830, #26468, #4768, #16345, #12074, #18578, #28225, #16194, #25841, #4148, #25992, #23468, #4298, #13946, #1940, #15211, #24857, #9702, #29160, #29002, #17428, #19968, #19365, #29604, #14743, #7312, #10010, #19673, #29313, #12356, #5398, #16980, #22042, #3175, #7931, #26630, #2573, #15057, #22203, #24712, #14886, #7624, #3024, #26926, #12218, #29450, #12815, #21901, #12668, #10152, #12520, #339, #492, #22499, #7476, #24403, #17283, #27245, #19818, #22349, #17600, #640, #10299, #24261, #19512, #4937, #14595, #24549, #5093, #9843, #5234, #2868, #17142, #7763, #185, #27078, #5562, #26789, #2712, #6184, #3643, #3499, #27868, #10464, #13139, #25645, #30389, #20146, #25009, #15829, #13279, #25482, #6037, #1116, #3791 ) ),
 .UNSPECIFIED., .F., .F., .T. ) 
 B_SPLINE_SURFACE_WITH_KNOTS ( ( 2, 2 ),
 ( 3, 2, 2, 2, 2, 2, 2, 2, 2, 2, 2, 2, 2, 2, 2, 2, 2, 2, 2, 2, 2, 2, 2, 2, 2, 2, 2, 2, 2, 2, 2, 2, 2, 2, 2, 2, 2, 2, 2, 2, 2, 2, 2, 2, 2, 2, 2, 2, 2, 2, 2, 2, 2, 2, 3 ),
 ( 0.000000000000000000, 1.000000000000000000 ),
 ( 0.000000000000000000, 0.01851851851851851749, 0.03703703703703703498, 0.05555555555555555247, 0.07407407407407406996, 0.09259259259259258745, 0.1111111111111111049, 0.1296296296296296224, 0.1481481481481481399, 0.1666666666666666574, 0.1851851851851851749, 0.2037037037037036924, 0.2222222222222222099, 0.2407407407407407274, 0.2592592592592592449, 0.2777777777777777901, 0.2962962962962962798, 0.3148148148148148251, 0.3333333333333333148, 0.3518518518518518601, 0.3703703703703703498, 0.3888888888888888951, 0.4074074074074073848, 0.4259259259259259300, 0.4444444444444444198, 0.4629629629629629650, 0.4814814814814814548, 0.5000000000000000000, 0.5185185185185184897, 0.5370370370370370905, 0.5555555555555555802, 0.5740740740740740700, 0.5925925925925925597, 0.6111111111111111605, 0.6296296296296296502, 0.6481481481481481399, 0.6666666666666666297, 0.6851851851851852304, 0.7037037037037037202, 0.7222222222222222099, 0.7407407407407406996, 0.7592592592592593004, 0.7777777777777777901, 0.7962962962962962798, 0.8148148148148147696, 0.8333333333333333703, 0.8518518518518518601, 0.8703703703703703498, 0.8888888888888888395, 0.9074074074074074403, 0.9259259259259259300, 0.9444444444444444198, 0.9629629629629629095, 0.9814814814814815103, 1.000000000000000000 ),
 .UNSPECIFIED. ) 
 GEOMETRIC_REPRESENTATION_ITEM ( )  RATIONAL_B_SPLINE_SURFACE ( (
 ( 1.000000000000000000, 0.8660254037844387076, 1.000000000000000000, 0.8660254037844387076, 1.000000000000000000, 0.8660254037844387076, 1.000000000000000000, 0.8660254037844387076, 1.000000000000000000, 0.8660254037844387076, 1.000000000000000000, 0.8660254037844387076, 1.000000000000000000, 0.8660254037844387076, 1.000000000000000000, 0.8660254037844387076, 1.000000000000000000, 0.8660254037844387076, 1.000000000000000000, 0.8660254037844387076, 1.000000000000000000, 0.8660254037844387076, 1.000000000000000000, 0.8660254037844387076, 1.000000000000000000, 0.8660254037844387076, 1.000000000000000000, 0.8660254037844387076, 1.000000000000000000, 0.8660254037844387076, 1.000000000000000000, 0.8660254037844387076, 1.000000000000000000, 0.8660254037844387076, 1.000000000000000000, 0.8660254037844387076, 1.000000000000000000, 0.8660254037844387076, 1.000000000000000000, 0.8660254037844387076, 1.000000000000000000, 0.8660254037844387076, 1.000000000000000000, 0.8660254037844387076, 1.000000000000000000, 0.8660254037844387076, 1.000000000000000000, 0.8660254037844387076, 1.000000000000000000, 0.8660254037844387076, 1.000000000000000000, 0.8660254037844387076, 1.000000000000000000, 0.8660254037844387076, 1.000000000000000000, 0.8660254037844387076, 1.000000000000000000, 0.8660254037844387076, 1.000000000000000000, 0.8660254037844387076, 1.000000000000000000, 0.8660254037844387076, 1.000000000000000000, 0.8660254037844387076, 1.000000000000000000, 0.8660254037844387076, 1.000000000000000000, 0.8660254037844387076, 1.000000000000000000, 0.8660254037844387076, 1.000000000000000000, 0.8660254037844387076, 1.000000000000000000, 0.8660254037844387076, 1.000000000000000000, 0.8660254037844387076, 1.000000000000000000, 0.8660254037844387076, 1.000000000000000000, 0.8660254037844387076, 1.000000000000000000, 0.8660254037844387076, 1.000000000000000000, 0.8660254037844387076, 1.000000000000000000, 0.8660254037844387076, 1.000000000000000000, 0.8660254037844387076, 1.000000000000000000, 0.8660254037844387076, 1.000000000000000000, 0.8660254037844387076, 1.000000000000000000, 0.8660254037844387076, 1.000000000000000000, 0.8660254037844387076, 1.000000000000000000, 0.8660254037844387076, 1.000000000000000000, 0.8660254037844387076, 1.000000000000000000, 0.8660254037844387076, 1.000000000000000000, 0.8660254037844387076, 1.000000000000000000, 0.8660254037844387076, 1.000000000000000000, 0.8660254037844387076, 1.000000000000000000),
 ( 1.000000000000000000, 0.8660254037844387076, 1.000000000000000000, 0.8660254037844387076, 1.000000000000000000, 0.8660254037844387076, 1.000000000000000000, 0.8660254037844387076, 1.000000000000000000, 0.8660254037844387076, 1.000000000000000000, 0.8660254037844387076, 1.000000000000000000, 0.8660254037844387076, 1.000000000000000000, 0.8660254037844387076, 1.000000000000000000, 0.8660254037844387076, 1.000000000000000000, 0.8660254037844387076, 1.000000000000000000, 0.8660254037844387076, 1.000000000000000000, 0.8660254037844387076, 1.000000000000000000, 0.8660254037844387076, 1.000000000000000000, 0.8660254037844387076, 1.000000000000000000, 0.8660254037844387076, 1.000000000000000000, 0.8660254037844387076, 1.000000000000000000, 0.8660254037844387076, 1.000000000000000000, 0.8660254037844387076, 1.000000000000000000, 0.8660254037844387076, 1.000000000000000000, 0.8660254037844387076, 1.000000000000000000, 0.8660254037844387076, 1.000000000000000000, 0.8660254037844387076, 1.000000000000000000, 0.8660254037844387076, 1.000000000000000000, 0.8660254037844387076, 1.000000000000000000, 0.8660254037844387076, 1.000000000000000000, 0.8660254037844387076, 1.000000000000000000, 0.8660254037844387076, 1.000000000000000000, 0.8660254037844387076, 1.000000000000000000, 0.8660254037844387076, 1.000000000000000000, 0.8660254037844387076, 1.000000000000000000, 0.8660254037844387076, 1.000000000000000000, 0.8660254037844387076, 1.000000000000000000, 0.8660254037844387076, 1.000000000000000000, 0.8660254037844387076, 1.000000000000000000, 0.8660254037844387076, 1.000000000000000000, 0.8660254037844387076, 1.000000000000000000, 0.8660254037844387076, 1.000000000000000000, 0.8660254037844387076, 1.000000000000000000, 0.8660254037844387076, 1.000000000000000000, 0.8660254037844387076, 1.000000000000000000, 0.8660254037844387076, 1.000000000000000000, 0.8660254037844387076, 1.000000000000000000, 0.8660254037844387076, 1.000000000000000000, 0.8660254037844387076, 1.000000000000000000, 0.8660254037844387076, 1.000000000000000000, 0.8660254037844387076, 1.000000000000000000, 0.8660254037844387076, 1.000000000000000000, 0.8660254037844387076, 1.000000000000000000, 0.8660254037844387076, 1.000000000000000000, 0.8660254037844387076, 1.000000000000000000, 0.8660254037844387076, 1.000000000000000000, 0.8660254037844387076, 1.000000000000000000, 0.8660254037844387076, 1.000000000000000000, 0.8660254037844387076, 1.000000000000000000) ) ) 
 REPRESENTATION_ITEM ( '' )  SURFACE ( )  );
#12183 = FACE_BOUND ( 'NONE', #6356, .T. ) ;
#12184 = ORIENTED_EDGE ( 'NONE', *, *, #16717, .F. ) ;
#12185 = CARTESIAN_POINT ( 'NONE',  ( 15.74652664997095286, -3.008101665203153807, 4.495550615867657918 ) ) ;
#12186 = AXIS2_PLACEMENT_3D ( 'NONE', #25177, #790, #25329 ) ;
#12187 = DIRECTION ( 'NONE',  ( 3.489354422748178582E-15, -1.218509414717996338E-16, 1.000000000000000000 ) ) ;
#12188 = EDGE_CURVE ( 'NONE', #25083, #20971, #20250, .T. ) ;
#12189 = CIRCLE ( 'NONE', #8137, 0.09999999999999986677 ) ;
#12190 = ADVANCED_FACE ( 'NONE', ( #29225 ), #12272, .F. ) ;
#12191 = CARTESIAN_POINT ( 'NONE',  ( -62.04999999999998295, -2.687391533643777919, 0.2606275981160458555 ) ) ;
#12194 = ADVANCED_FACE ( 'NONE', ( #17200 ), #26704, .F. ) ;
#12193 = DIRECTION ( 'NONE',  ( -1.451851013137922794E-14, 0.8914544820238117229, -0.4531102586343168093 ) ) ;
#12192 = CARTESIAN_POINT ( 'NONE',  ( -59.46761860684633660, 2.377675374897951333, -1.175485268738917677 ) ) ;
#12195 = DIRECTION ( 'NONE',  ( 0.000000000000000000, 0.3137254901960787046, 0.9495137264943726008 ) ) ;
#12197 = CARTESIAN_POINT ( 'NONE',  ( 50.36640492253748391, -1.250162886418155761, -3.874884102585953727 ) ) ;
#12196 = CARTESIAN_POINT ( 'NONE',  ( 58.75000000000001421, 0.6121634413823866527, 1.877732920581527409 ) ) ;
#12198 = ORIENTED_EDGE ( 'NONE', *, *, #8075, .F. ) ;
#12199 = CARTESIAN_POINT ( 'NONE',  ( 58.75000000000004263, -1.932246131436417436, 0.4087173687851148873 ) ) ;
#12200 = CARTESIAN_POINT ( 'NONE',  ( -59.19999999999996732, 4.156921938165317520, -0.9498634748674451567 ) ) ;
#12202 = FACE_OUTER_BOUND ( 'NONE', #6359, .T. ) ;
#12201 = CARTESIAN_POINT ( 'NONE',  ( -59.25776236348306014, 2.397420733123352576, 3.154278791497947765 ) ) ;
#12203 = FACE_OUTER_BOUND ( 'NONE', #368, .T. ) ;
#12204 = VERTEX_POINT ( 'NONE', #14950 ) ;
#12205 = EDGE_LOOP ( 'NONE', ( #19761, #10825, #29436, #1959, #15890 ) ) ;
#12206 = AXIS2_PLACEMENT_3D ( 'NONE', #21221, #6630, #21053 ) ;
#12207 = DIRECTION ( 'NONE',  ( 1.000000000000000000, 3.053848253006669023E-16, -2.042510438544995415E-16 ) ) ;
#12208 = ORIENTED_EDGE ( 'NONE', *, *, #24035, .T. ) ;
#12209 = FACE_OUTER_BOUND ( 'NONE', #17576, .T. ) ;
#12210 = FACE_OUTER_BOUND ( 'NONE', #19746, .T. ) ;
#12211 = ORIENTED_EDGE ( 'NONE', *, *, #159, .T. ) ;
#12212 = CARTESIAN_POINT ( 'NONE',  ( -35.85663232820580504, -5.340403872473343583, -0.9205822173396128738 ) ) ;
#12213 = EDGE_LOOP ( 'NONE', ( #24873, #22728, #21856, #8267 ) ) ;
#12214 = CARTESIAN_POINT ( 'NONE',  ( 50.93273830208138975, -4.031600731908413060, -1.173113608511851869 ) ) ;
#12215 = ORIENTED_EDGE ( 'NONE', *, *, #1559, .F. ) ;
#12216 =( BOUNDED_CURVE ( )  B_SPLINE_CURVE ( 2, ( #17878, #3305, #3620, #12952, #13111, #22647, #7893, #25308, #19940 ),
 .UNSPECIFIED., .F., .T. ) 
 B_SPLINE_CURVE_WITH_KNOTS ( ( 3, 2, 2, 2, 3 ),
 ( 0.5833333333333333703, 0.5925925925925925597, 0.6111111111111111605, 0.6296296296296296502, 0.6388888888888889506 ),
 .UNSPECIFIED. ) 
 CURVE ( )  GEOMETRIC_REPRESENTATION_ITEM ( )  RATIONAL_B_SPLINE_CURVE ( ( 0.9330127018922194093, 0.9330127018922197424, 1.000000000000000000, 0.8660254037844387076, 1.000000000000000000, 0.8660254037844387076, 1.000000000000000000, 0.9330127018922189652, 0.9330127018922194093 ) ) 
 REPRESENTATION_ITEM ( '' )  );
#12217 = EDGE_LOOP ( 'NONE', ( #13060, #22379, #19354, #17414 ) ) ;
#12218 = CARTESIAN_POINT ( 'NONE',  ( -58.00952994616203284, 3.117691453623994580, -1.800000000000192557 ) ) ;
#12219 = CARTESIAN_POINT ( 'NONE',  ( 52.80968221184927103, 4.034333029853865327, -2.050000000000183675 ) ) ;
#12220 = DIRECTION ( 'NONE',  ( 3.051840300662039536E-15, -0.4857787595540328796, 0.8740818021021518058 ) ) ;
#12221 = LINE ( 'NONE', #10013, #15965 ) ;
#12222 = DIRECTION ( 'NONE',  ( -2.581436205204234499E-16, 0.9796124928211140670, 0.2008964009354147762 ) ) ;
#12223 = EDGE_CURVE ( 'NONE', #28004, #24689, #16887, .T. ) ;
#12224 = AXIS2_PLACEMENT_3D ( 'NONE', #13718, #30669, #18028 ) ;
#12227 = ADVANCED_FACE ( 'NONE', ( #12133 ), #19587, .T. ) ;
#12226 = CARTESIAN_POINT ( 'NONE',  ( -61.39919102937894735, -2.565992354215222981, -0.8400338161548545068 ) ) ;
#12225 = CARTESIAN_POINT ( 'NONE',  ( 51.80000000000002558, -4.387164041431067751, 1.383037119376577140 ) ) ;
#12228 = DIRECTION ( 'NONE',  ( 1.000000000000000000, 0.000000000000000000, -3.491481338843133355E-15 ) ) ;
#12229 = CARTESIAN_POINT ( 'NONE',  ( 51.64837794009019944, 0.8283786772117788244, -1.688958810662479104 ) ) ;
#12231 = CARTESIAN_POINT ( 'NONE',  ( 51.87765138016307986, 8.698644590117595499, -2.050000000000180123 ) ) ;
#12230 = CARTESIAN_POINT ( 'NONE',  ( 15.95705409078463788, 4.926689578693635774, -2.233438676318118432 ) ) ;
#12232 = VERTEX_POINT ( 'NONE', #12581 ) ;
#12233 = CARTESIAN_POINT ( 'NONE',  ( 47.10000000000002274, 6.982261990806648555E-14, -1.632474749424821370E-13 ) ) ;
#12234 = CARTESIAN_POINT ( 'NONE',  ( -59.09999999999997300, 8.366749974758448157E-15, -2.099585467500611340E-13 ) ) ;
#12236 = CARTESIAN_POINT ( 'NONE',  ( 52.89442146867855854, 4.088415591072481980, 0.3516000293862507342 ) ) ;
#12235 = CARTESIAN_POINT ( 'NONE',  ( 48.50000000000263611, -1.409901620923685206, 3.849999999997240518 ) ) ;
#12237 = CARTESIAN_POINT ( 'NONE',  ( -35.85663232820584057, -5.086913985776155833, -1.171642053949114803 ) ) ;
#12238 = ORIENTED_EDGE ( 'NONE', *, *, #2544, .T. ) ;
#12239 = DIRECTION ( 'NONE',  ( -9.754918421198724481E-16, 0.9601771338024399638, -0.2793919678926571892 ) ) ;
#12240 = ADVANCED_FACE ( 'NONE', ( #26380 ), #24620, .T. ) ;
#12241 = ORIENTED_EDGE ( 'NONE', *, *, #29768, .F. ) ;
#12242 = DIRECTION ( 'NONE',  ( -1.000000000000000000, 0.000000000000000000, 3.469446951951483476E-15 ) ) ;
#12243 = VERTEX_POINT ( 'NONE', #22115 ) ;
#12244 = ORIENTED_EDGE ( 'NONE', *, *, #10383, .T. ) ;
#12245 = CARTESIAN_POINT ( 'NONE',  ( 61.09423418604048095, 0.6373668173476213505, -1.895722432252298084 ) ) ;
#12246 = ORIENTED_EDGE ( 'NONE', *, *, #27243, .F. ) ;
#12247 = CARTESIAN_POINT ( 'NONE',  ( 48.46953526341860652, -1.366509374015013600, 3.854674997130604908 ) ) ;
#12248 = CARTESIAN_POINT ( 'NONE',  ( -55.13452994616203995, 2.093608279459367933E-14, -3.600000000000195932 ) ) ;
#12249 = EDGE_LOOP ( 'NONE', ( #5509, #9842, #10337, #26716 ) ) ;
#12250 = CARTESIAN_POINT ( 'NONE',  ( 54.45370770736469268, -0.0004837498569785767585, 4.360091688067994298 ) ) ;
#12251 = DIRECTION ( 'NONE',  ( -1.000000000000000000, -3.053848253006669023E-16, 2.042510438544995415E-16 ) ) ;
#12252 = CARTESIAN_POINT ( 'NONE',  ( 29.93605863096246367, 6.616288078318590671, 2.049999999999895461 ) ) ;
#12253 = ORIENTED_EDGE ( 'NONE', *, *, #3910, .F. ) ;
#12254 = CARTESIAN_POINT ( 'NONE',  ( -54.87499999999998579, -3.920666489018356189E-15, 3.399999999999804068 ) ) ;
#12255 = CARTESIAN_POINT ( 'NONE',  ( -54.44999999999997442, -1.499999999999998668, 4.029888335921975262 ) ) ;
#12256 = CARTESIAN_POINT ( 'NONE',  ( 58.75000000000002842, -1.066009655020577096, -1.652371589363125004 ) ) ;
#12257 = DIRECTION ( 'NONE',  ( -1.000000000000000000, -0.000000000000000000, 3.491481338843133355E-15 ) ) ;
#12258 = CARTESIAN_POINT ( 'NONE',  ( 57.01898512823798626, 0.7746824256175574019, 1.734896867090173211 ) ) ;
#12259 = EDGE_CURVE ( 'NONE', #203, #9827, #19569, .T. ) ;
#12261 = CYLINDRICAL_SURFACE ( 'NONE', #27038, 0.1500000000000002720 ) ;
#12260 = CARTESIAN_POINT ( 'NONE',  ( -54.49999999999997868, 3.796242339859525868E-15, -5.550248518040434488E-16 ) ) ;
#12262 = FACE_OUTER_BOUND ( 'NONE', #28444, .T. ) ;
#12263 = CARTESIAN_POINT ( 'NONE',  ( -63.84999999999997300, 6.335931579819947332E-16, 2.555166080847169934E-15 ) ) ;
#12264 = CARTESIAN_POINT ( 'NONE',  ( -62.14999999999998437, 2.799131621120617641, 0.06972924524667370449 ) ) ;
#12265 = ORIENTED_EDGE ( 'NONE', *, *, #9337, .T. ) ;
#12266 = ADVANCED_FACE ( 'NONE', ( #554 ), #100, .F. ) ;
#12267 = ORIENTED_EDGE ( 'NONE', *, *, #22720, .F. ) ;
#12268 = FACE_OUTER_BOUND ( 'NONE', #28081, .T. ) ;
#12269 = CIRCLE ( 'NONE', #152, 0.1000000000000001443 ) ;
#12270 = CARTESIAN_POINT ( 'NONE',  ( -60.72085481156722864, 1.184343223768590470, 3.558065644182728082 ) ) ;
#12272 = PLANE ( 'NONE',  #10621 ) ;
#12271 = CARTESIAN_POINT ( 'NONE',  ( 16.00221665700882312, 5.295593823078800000, 1.114646847977682098 ) ) ;
#12273 = VERTEX_POINT ( 'NONE', #31289 ) ;
#12274 = ORIENTED_EDGE ( 'NONE', *, *, #5828, .T. ) ;
#12275 = CARTESIAN_POINT ( 'NONE',  ( 58.45000000000001705, -0.8000000000000000444, 3.499999999999999556 ) ) ;
#12276 = ORIENTED_EDGE ( 'NONE', *, *, #22145, .T. ) ;
#12277 = CARTESIAN_POINT ( 'NONE',  ( -73.90999999999998238, -2.438578184542714499E-15, 4.609931582023435380E-15 ) ) ;
#12278 = ORIENTED_EDGE ( 'NONE', *, *, #27542, .T. ) ;
#12279 = CARTESIAN_POINT ( 'NONE',  ( 34.56702326949724124, 8.213851659285211326, -2.050000000000119726 ) ) ;
#12280 = CARTESIAN_POINT ( 'NONE',  ( 51.18880157753722671, -1.010242313720678631, 1.292695951881193794 ) ) ;
#12281 = CARTESIAN_POINT ( 'NONE',  ( 51.99340984296998158, 4.356875777028168528, 1.476187001954879952 ) ) ;
#12282 = CARTESIAN_POINT ( 'NONE',  ( 58.75000000000004263, -2.079005547593188119, 1.932245437381540134E-15 ) ) ;
#12283 = CARTESIAN_POINT ( 'NONE',  ( -55.64405989232412253, 2.944486372867106461, -1.700000000000184919 ) ) ;
#12284 = CARTESIAN_POINT ( 'NONE',  ( 53.87827693845218846, 5.944250707180090743, -1.708828125785526675 ) ) ;
#12285 = EDGE_CURVE ( 'NONE', #24464, #31094, #13350, .T. ) ;
#12286 = CARTESIAN_POINT ( 'NONE',  ( -56.53335481156723574, 0.7533615035078095046, -3.673546848079178861 ) ) ;
#12287 = CARTESIAN_POINT ( 'NONE',  ( 50.36581974271289397, 1.399739523915438211, -3.853780793998481169 ) ) ;
#12288 = AXIS2_PLACEMENT_3D ( 'NONE', #29582, #5686, #22808 ) ;
#12289 = EDGE_CURVE ( 'NONE', #7611, #24092, #14277, .T. ) ;
#12290 = DIRECTION ( 'NONE',  ( 0.000000000000000000, -1.000000000000000000, -0.000000000000000000 ) ) ;
#12291 = LINE ( 'NONE', #19612, #5851 ) ;
#12292 = EDGE_LOOP ( 'NONE', ( #9727, #26571, #16668, #25816 ) ) ;
#12293 = DIRECTION ( 'NONE',  ( 1.000000000000000000, 1.047444401652940007E-14, 0.000000000000000000 ) ) ;
#12294 = CARTESIAN_POINT ( 'NONE',  ( -36.42771574642738130, -3.560621078037132570, -4.077054076718796161 ) ) ;
#12295 = CARTESIAN_POINT ( 'NONE',  ( 54.00139016905851008, 6.058270281819565284, 1.948881089517881637 ) ) ;
#12296 = ORIENTED_EDGE ( 'NONE', *, *, #12393, .T. ) ;
#12297 = EDGE_CURVE ( 'NONE', #11854, #22512, #6925, .T. ) ;
#12298 = LINE ( 'NONE', #16438, #30500 ) ;
#12299 = VERTEX_POINT ( 'NONE', #3414 ) ;
#12300 = FILL_AREA_STYLE_COLOUR ( '', #6642 ) ;
#12301 = CARTESIAN_POINT ( 'NONE',  ( -36.92443669619682112, -5.191204783933228484, 1.522159526382896866 ) ) ;
#12303 = DIRECTION ( 'NONE',  ( 3.023770467182126270E-15, 0.4999707644721522182, 0.8660422822663637055 ) ) ;
#12302 = LINE ( 'NONE', #9947, #12986 ) ;
#12304 = ORIENTED_EDGE ( 'NONE', *, *, #25578, .F. ) ;
#12305 = DIRECTION ( 'NONE',  ( 1.000000000000000000, 0.000000000000000000, 0.000000000000000000 ) ) ;
#12307 = LINE ( 'NONE', #19776, #27685 ) ;
#12306 = CARTESIAN_POINT ( 'NONE',  ( 51.45655683570191741, -0.9591657938390835136, -1.196087371390569087 ) ) ;
#12308 = VERTEX_POINT ( 'NONE', #27155 ) ;
#12309 = CARTESIAN_POINT ( 'NONE',  ( -57.74999999999997158, -1.184343223768585807, -3.558065644182723641 ) ) ;
#12310 = CIRCLE ( 'NONE', #15362, 4.786668705877438867 ) ;
#12311 = CARTESIAN_POINT ( 'NONE',  ( 58.75000000000002132, 6.153735859711025284E-13, 3.111507638930570854E-58 ) ) ;
#12312 = CARTESIAN_POINT ( 'NONE',  ( -55.99999999999995737, 2.190330617366546392E-14, -3.400000000000199307 ) ) ;
#12313 = EDGE_CURVE ( 'NONE', #4345, #473, #877, .T. ) ;
#12314 = CARTESIAN_POINT ( 'NONE',  ( -55.40400635094609072, -3.399999999999988365, -0.9110272542660277084 ) ) ;
#12315 = CARTESIAN_POINT ( 'NONE',  ( 68.00000000000004263, 2.908536147974970122E-16, 2.374999999999286793 ) ) ;
#12316 = CARTESIAN_POINT ( 'NONE',  ( 51.80000000000001847, -0.1421112804877788793, -7.888760782825513275E-16 ) ) ;
#12317 = CARTESIAN_POINT ( 'NONE',  ( 50.25000000000003553, -1.499837071477821082, -1.323060376181415254 ) ) ;
#12318 = ORIENTED_EDGE ( 'NONE', *, *, #3336, .T. ) ;
#12319 = ADVANCED_FACE ( 'NONE', ( #25397 ), #5469, .T. ) ;
#12320 = CYLINDRICAL_SURFACE ( 'NONE', #6466, 4.600000000000036948 ) ;
#12321 = EDGE_CURVE ( 'NONE', #3273, #17666, #5394, .T. ) ;
#12322 = ADVANCED_BREP_SHAPE_REPRESENTATION ( '', ( #4756, #9018 ), #5016 ) ;
#12323 = CARTESIAN_POINT ( 'NONE',  ( 26.50971933136674608, 5.213424020870816022, -1.950000000000092770 ) ) ;
#12324 = ADVANCED_FACE ( 'NONE', ( #15599 ), #2652, .T. ) ;
#12325 = DIRECTION ( 'NONE',  ( 0.000000000000000000, 0.1576190026614809614, -0.9875000000000001554 ) ) ;
#12326 = CARTESIAN_POINT ( 'NONE',  ( 58.65000000000001279, 0.8948927608033908632, 1.760622601997029690 ) ) ;
#12327 = CIRCLE ( 'NONE', #10820, 2.600000000000000089 ) ;
#12328 = CARTESIAN_POINT ( 'NONE',  ( 61.25000000000000000, 1.791164585743364901, -0.8897917884432851032 ) ) ;
#12330 = CARTESIAN_POINT ( 'NONE',  ( 29.64923672893716855, 6.300449151053627794, 1.424999999999897238 ) ) ;
#12329 = LINE ( 'NONE', #19483, #28154 ) ;
#12331 = ORIENTED_EDGE ( 'NONE', *, *, #28902, .F. ) ;
#12332 = CARTESIAN_POINT ( 'NONE',  ( 58.75000018595673623, -1.857295262527126845, 0.5493460779660276350 ) ) ;
#12333 = ORIENTED_EDGE ( 'NONE', *, *, #5560, .T. ) ;
#12334 = PRODUCT_DEFINITION_CONTEXT ( 'detailed design', #9192, 'design' ) ;
#12335 = DIRECTION ( 'NONE',  ( 0.000000000000000000, -0.2008964009354147762, 0.9796124928211140670 ) ) ;
#12337 = FACE_OUTER_BOUND ( 'NONE', #19887, .T. ) ;
#12336 = CARTESIAN_POINT ( 'NONE',  ( 15.44631504820157808, -3.231775792180293649, -4.079530926931276724 ) ) ;
#12338 = DIRECTION ( 'NONE',  ( 1.000000000000000000, 1.047444401652940007E-14, 0.000000000000000000 ) ) ;
#12339 = VERTEX_POINT ( 'NONE', #23033 ) ;
#12340 = AXIS2_PLACEMENT_3D ( 'NONE', #126, #19151, #4866 ) ;
#12341 = ORIENTED_EDGE ( 'NONE', *, *, #22851, .T. ) ;
#12342 = CARTESIAN_POINT ( 'NONE',  ( -53.99999999999997868, 5.755839955992559655E-16, -4.700000000000000178 ) ) ;
#12343 = ORIENTED_EDGE ( 'NONE', *, *, #28240, .T. ) ;
#12344 = DIRECTION ( 'NONE',  ( -1.000000000000000000, -1.047444401652940007E-14, -0.000000000000000000 ) ) ;
#12345 =( BOUNDED_CURVE ( )  B_SPLINE_CURVE ( 3, ( #29893, #15487, #3465, #24826 ),
 .UNSPECIFIED., .F., .T. ) 
 B_SPLINE_CURVE_WITH_KNOTS ( ( 4, 4 ),
 ( 4.829242994979814796, 4.929162845165778961 ),
 .UNSPECIFIED. ) 
 CURVE ( )  GEOMETRIC_REPRESENTATION_ITEM ( )  RATIONAL_B_SPLINE_CURVE ( ( 1.000000000000000000, 0.9991681750023542197, 0.9991681750023542197, 1.000000000000000000 ) ) 
 REPRESENTATION_ITEM ( '' )  );
#12346 = LINE ( 'NONE', #27066, #23005 ) ;
#12347 = EDGE_CURVE ( 'NONE', #2409, #24563, #19859, .T. ) ;
#12348 = CARTESIAN_POINT ( 'NONE',  ( -36.42771574642760157, -5.277035221755912886, -1.205525476379292416 ) ) ;
#12349 = ORIENTED_EDGE ( 'NONE', *, *, #9738, .T. ) ;
#12350 = CARTESIAN_POINT ( 'NONE',  ( -71.44999999999998863, -0.2962051453644871657, 1.444357686279452047 ) ) ;
#12351 =( NAMED_UNIT ( * ) PLANE_ANGLE_UNIT ( ) SI_UNIT ( $, .RADIAN. ) );
#12352 = APPLICATION_CONTEXT ( 'automotive_design' ) ;
#12353 = EDGE_CURVE ( 'NONE', #10074, #7683, #7504, .T. ) ;
#12354 = AXIS2_PLACEMENT_3D ( 'NONE', #19773, #29406, #17377 ) ;
#12355 = ORIENTED_EDGE ( 'NONE', *, *, #19010, .T. ) ;
#12356 = CARTESIAN_POINT ( 'NONE',  ( -57.07202994616206126, 2.078460969082646770, 3.599999999999804690 ) ) ;
#12357 = CARTESIAN_POINT ( 'NONE',  ( 52.98753545145216037, 8.419778228641124684, -2.050000000000184563 ) ) ;
#12358 = CARTESIAN_POINT ( 'NONE',  ( 22.07280086217094706, 8.086143481909154218, 1.949999999999922906 ) ) ;
#12359 = FACE_OUTER_BOUND ( 'NONE', #14871, .T. ) ;
#12360 = PLANE ( 'NONE',  #24163 ) ;
#12361 = CARTESIAN_POINT ( 'NONE',  ( -57.04806624327023457, 3.400000000000003908, 0.9110272542656316919 ) ) ;
#12363 = CARTESIAN_POINT ( 'NONE',  ( -61.35802040574235861, -2.553010640673968989, -0.8058083345264630548 ) ) ;
#12362 = DIRECTION ( 'NONE',  ( 0.000000000000000000, 0.000000000000000000, 1.000000000000000000 ) ) ;
#12364 = VECTOR ( 'NONE', #24617, 1000.000000000000000 ) ;
#12365 = CIRCLE ( 'NONE', #17441, 0.2500000000000000000 ) ;
#12366 = CARTESIAN_POINT ( 'NONE',  ( 47.10000000000000853, -3.933368109459638884, -2.186004417993339111 ) ) ;
#12367 = DIRECTION ( 'NONE',  ( -1.000000000000000000, -0.000000000000000000, -0.000000000000000000 ) ) ;
#12369 = CARTESIAN_POINT ( 'NONE',  ( -62.09999999999997300, -2.625757682666624238, -0.2804666419185134485 ) ) ;
#12368 = CARTESIAN_POINT ( 'NONE',  ( 15.03925126672132606, 4.861582140531648832, -2.394243978978272569 ) ) ;
#12370 = EDGE_LOOP ( 'NONE', ( #15040, #27187, #22997, #17999 ) ) ;
#12371 = DIRECTION ( 'NONE',  ( -2.614375865348240525E-16, 0.2008964009354147762, -0.9796124928211140670 ) ) ;
#12372 = B_SPLINE_CURVE_WITH_KNOTS ( 'NONE', 3,
 ( #25167, #2843, #29756, #12799, #22480, #22022, #315, #8073, #7608, #17263, #26908, #14866, #10135, #23115, #8826, #27856 ),
 .UNSPECIFIED., .F., .F.,
 ( 4, 3, 3, 3, 3, 4 ),
 ( 0.000000000000000000, 1.625241835515689952E-05, 3.292491922809579385E-05, 5.060195339673861708E-05, 6.961003767230190245E-05, 8.476187580399473969E-05 ),
 .UNSPECIFIED. ) ;
#12373 = AXIS2_PLACEMENT_3D ( 'NONE', #15855, #3530, #20640 ) ;
#12374 = CARTESIAN_POINT ( 'NONE',  ( 47.02521898271880474, -4.051679580537261849, -1.951144708070795541 ) ) ;
#12376 = FACE_OUTER_BOUND ( 'NONE', #17333, .T. ) ;
#12375 = CARTESIAN_POINT ( 'NONE',  ( -59.92928932188130631, -0.9743475445367597576, 4.751120590182403625 ) ) ;
#12377 = CARTESIAN_POINT ( 'NONE',  ( 46.99709697984359025, -4.086844330037576078, 2.115703333131348174 ) ) ;
#12378 = ORIENTED_EDGE ( 'NONE', *, *, #29511, .T. ) ;
#12379 = CARTESIAN_POINT ( 'NONE',  ( 50.30000000000001847, 1.426739617975221641, 3.843750000000023093 ) ) ;
#12380 = ORIENTED_EDGE ( 'NONE', *, *, #2752, .F. ) ;
#12381 = AXIS2_PLACEMENT_3D ( 'NONE', #28843, #6827, #16666 ) ;
#12382 = CARTESIAN_POINT ( 'NONE',  ( 15.90468948301722918, -5.313409993919707475, 1.009519134730179291 ) ) ;
#12383 = ORIENTED_EDGE ( 'NONE', *, *, #25413, .T. ) ;
#12384 = EDGE_LOOP ( 'NONE', ( #9795, #15078, #24165, #25859, #7285, #9835 ) ) ;
#12385 = EDGE_CURVE ( 'NONE', #2387, #12697, #359, .T. ) ;
#12386 = CARTESIAN_POINT ( 'NONE',  ( 15.18463186935387554, 5.377732432866777934, -0.5657657256209858154 ) ) ;
#12387 = EDGE_LOOP ( 'NONE', ( #18884, #27656, #25875, #20850 ) ) ;
#12388 = ADVANCED_FACE ( 'NONE', ( #12209 ), #13996, .T. ) ;
#12389 = CARTESIAN_POINT ( 'NONE',  ( 51.89794158693270987, 4.415147102489865638, 1.292252039327525859 ) ) ;
#12390 = CARTESIAN_POINT ( 'NONE',  ( -55.75952994616203995, 3.117691453623994580, -1.800000000000184563 ) ) ;
#12391 = ORIENTED_EDGE ( 'NONE', *, *, #23328, .T. ) ;
#12392 = LINE ( 'NONE', #377, #17642 ) ;
#12393 = EDGE_CURVE ( 'NONE', #3627, #28219, #2374, .T. ) ;
#12394 = LINE ( 'NONE', #19712, #7136 ) ;
#12395 = AXIS2_PLACEMENT_3D ( 'NONE', #31237, #4002, #13648 ) ;
#12396 = CARTESIAN_POINT ( 'NONE',  ( 33.40812713800838196, 8.122903761242909582, 1.949999999999884936 ) ) ;
#12397 = ORIENTED_EDGE ( 'NONE', *, *, #17439, .T. ) ;
#12398 = VECTOR ( 'NONE', #10938, 1000.000000000000000 ) ;
#12399 = DIRECTION ( 'NONE',  ( 1.000000000000000000, 0.000000000000000000, 0.000000000000000000 ) ) ;
#12400 = CARTESIAN_POINT ( 'NONE',  ( -57.22499999999997300, 2.964020293532818446E-15, 1.549317489258312010E-18 ) ) ;
#12401 = CARTESIAN_POINT ( 'NONE',  ( 58.74999981404334903, -1.050697058759886948, -1.649595783782785263 ) ) ;
#12402 = DIRECTION ( 'NONE',  ( 1.000000000000000000, 3.053848253006669023E-16, -2.042510438544995415E-16 ) ) ;
#12403 = AXIS2_PLACEMENT_3D ( 'NONE', #9110, #26361, #26036 ) ;
#12404 = EDGE_CURVE ( 'NONE', #27956, #16762, #21475, .T. ) ;
#12405 = CIRCLE ( 'NONE', #30098, 0.1000000000000000472 ) ;
#12407 = FACE_BOUND ( 'NONE', #4091, .T. ) ;
#12406 = CARTESIAN_POINT ( 'NONE',  ( -36.38139716712170468, -3.953723660658932992, 3.694477770903708436 ) ) ;
#12408 = CARTESIAN_POINT ( 'NONE',  ( 51.73137679800704802, -4.259946794064842557, 1.000000024775425711 ) ) ;
#12409 = CARTESIAN_POINT ( 'NONE',  ( 58.64999999999999858, 1.874150328521186681, -0.06593717335319848605 ) ) ;
#12410 = DIRECTION ( 'NONE',  ( -1.000000000000000000, -3.053848253006669023E-16, 2.042510438544995415E-16 ) ) ;
#12411 = ORIENTED_EDGE ( 'NONE', *, *, #5588, .F. ) ;
#12412 = AXIS2_PLACEMENT_3D ( 'NONE', #18546, #16162, #4119 ) ;
#12413 = AXIS2_PLACEMENT_3D ( 'NONE', #30076, #7936, #3646 ) ;
#12414 = ORIENTED_EDGE ( 'NONE', *, *, #2761, .T. ) ;
#12415 = EDGE_LOOP ( 'NONE', ( #21350, #14955, #21685, #17818 ) ) ;
#12416 = CARTESIAN_POINT ( 'NONE',  ( 53.71501932699290904, 7.815554144461332342, 2.049999999999812417 ) ) ;
#12417 = CARTESIAN_POINT ( 'NONE',  ( -57.54792740578359656, -1.073804522883517132, -3.225979517392335350 ) ) ;
#12419 = DIRECTION ( 'NONE',  ( 1.168655815394902336E-14, 0.000000000000000000, 1.000000000000000000 ) ) ;
#12418 = CYLINDRICAL_SURFACE ( 'NONE', #23160, 0.5000000000000000000 ) ;
#12420 = ORIENTED_EDGE ( 'NONE', *, *, #28589, .F. ) ;
#12421 = AXIS2_PLACEMENT_3D ( 'NONE', #22010, #12484, #17114 ) ;
#12422 = ORIENTED_EDGE ( 'NONE', *, *, #21476, .T. ) ;
#12423 = DIRECTION ( 'NONE',  ( 1.000000000000000000, 3.054025858079668409E-16, -2.042474015755241579E-16 ) ) ;
#12424 = VERTEX_POINT ( 'NONE', #23199 ) ;
#12425 = CIRCLE ( 'NONE', #30118, 2.650000000000000799 ) ;
#12426 = ADVANCED_FACE ( 'NONE', ( #4609 ), #26458, .F. ) ;
#12427 = CARTESIAN_POINT ( 'NONE',  ( -58.81249999999996447, 3.400000000000008349, -1.915049148454697437E-13 ) ) ;
#12428 = EDGE_LOOP ( 'NONE', ( #11745, #2710, #16627, #28611 ) ) ;
#12429 = CARTESIAN_POINT ( 'NONE',  ( 31.46392738815579548, 7.544460793879616212, -2.050000000000109512 ) ) ;
#12430 = MECHANICAL_DESIGN_GEOMETRIC_PRESENTATION_REPRESENTATION (  '', ( #4846 ), #19033 ) ;
#12431 = ORIENTED_EDGE ( 'NONE', *, *, #25276, .F. ) ;
#12432 = CARTESIAN_POINT ( 'NONE',  ( -58.12499999999997158, 1.184343223768580255, 3.558065644182728526 ) ) ;
#12433 = CARTESIAN_POINT ( 'NONE',  ( 46.90000000000001279, 1.734723475976807094E-15, 4.275000000000000355 ) ) ;
#12434 = AXIS2_PLACEMENT_3D ( 'NONE', #13019, #23790, #28693 ) ;
#12435 = FACE_OUTER_BOUND ( 'NONE', #23510, .T. ) ;
#12436 = CARTESIAN_POINT ( 'NONE',  ( -55.51905989232413674, 2.944486372867092250, 1.699999999999814104 ) ) ;
#12437 = CARTESIAN_POINT ( 'NONE',  ( 53.94440344817328281, 6.524635634306427789, -2.050000000000187228 ) ) ;
#12438 = AXIS2_PLACEMENT_3D ( 'NONE', #29941, #3513, #13152 ) ;
#12439 = EDGE_CURVE ( 'NONE', #4710, #30753, #8937, .T. ) ;
#12440 = CIRCLE ( 'NONE', #19553, 0.05000000000000014849 ) ;
#12441 = CARTESIAN_POINT ( 'NONE',  ( -58.49999999999997868, -2.944486372867095358, 1.699999999999771028 ) ) ;
#12442 = AXIS2_PLACEMENT_3D ( 'NONE', #28106, #25420, #13366 ) ;
#12443 = CIRCLE ( 'NONE', #322, 0.1500000000000001887 ) ;
#12444 = CARTESIAN_POINT ( 'NONE',  ( 15.71019289815288644, -4.797343084509205546, -2.497389432263995346 ) ) ;
#12445 = TOROIDAL_SURFACE ( 'NONE', #7887, 2.299325721147392088, 0.05000000000000000278 ) ;
#12446 = VECTOR ( 'NONE', #9722, 1000.000000000000000 ) ;
#12447 = DIRECTION ( 'NONE',  ( -1.000000000000000000, 0.000000000000000000, 1.047444401652940007E-14 ) ) ;
#12448 = ORIENTED_EDGE ( 'NONE', *, *, #18730, .F. ) ;
#12449 = CARTESIAN_POINT ( 'NONE',  ( 58.75000000000003553, -1.800471618824212694, -1.039502773796582069 ) ) ;
#12450 = EDGE_CURVE ( 'NONE', #28184, #6720, #6945, .T. ) ;
#12451 = CARTESIAN_POINT ( 'NONE',  ( -36.04581030752635229, -2.525801262579533191, -4.794550356814626824 ) ) ;
#12452 = CARTESIAN_POINT ( 'NONE',  ( 54.15033841019267413, 6.694122904935910334, 2.049999999999792877 ) ) ;
#12453 = ORIENTED_EDGE ( 'NONE', *, *, #18350, .F. ) ;
#12454 = CARTESIAN_POINT ( 'NONE',  ( 58.45000000000001705, -0.8000000000000000444, 1.778341924377873751 ) ) ;
#12455 = EDGE_LOOP ( 'NONE', ( #7541, #1330, #27275, #6353 ) ) ;
#12456 = PRESENTATION_STYLE_ASSIGNMENT (( #12166 ) ) ;
#12458 = DIRECTION ( 'NONE',  ( 0.000000000000000000, 0.000000000000000000, -1.000000000000000000 ) ) ;
#12457 = CARTESIAN_POINT ( 'NONE',  ( 51.88812122917396152, 8.998461838224883991, 1.949999999999818989 ) ) ;
#12459 = ORIENTED_EDGE ( 'NONE', *, *, #2601, .F. ) ;
#12460 = VECTOR ( 'NONE', #14093, 1000.000000000000000 ) ;
#12461 = CARTESIAN_POINT ( 'NONE',  ( -57.64405989232413674, -1.933093229062082635E-14, 3.399999999999794298 ) ) ;
#12462 = AXIS2_PLACEMENT_3D ( 'NONE', #20592, #10748, #18358 ) ;
#12463 = ADVANCED_FACE ( 'NONE', ( #19203 ), #16665, .F. ) ;
#12464 = DIRECTION ( 'NONE',  ( 1.000000000000000000, 0.000000000000000000, 0.000000000000000000 ) ) ;
#12466 = DIRECTION ( 'NONE',  ( -1.000000000000000000, -0.000000000000000000, 3.491481338843133355E-15 ) ) ;
#12465 = CARTESIAN_POINT ( 'NONE',  ( 47.10000000000000853, -3.550773357292059451, -2.049880134335985815 ) ) ;
#12467 = ORIENTED_EDGE ( 'NONE', *, *, #22900, .T. ) ;
#12468 = CARTESIAN_POINT ( 'NONE',  ( -60.31249999999996447, -0.8699069336946629871, 4.241846523238429256 ) ) ;
#12469 = CARTESIAN_POINT ( 'NONE',  ( -64.31974649313019654, 4.901397072418226544E-16, 2.651112292416007398E-15 ) ) ;
#12470 = AXIS2_PLACEMENT_3D ( 'NONE', #6623, #23409, #3510 ) ;
#12471 = CARTESIAN_POINT ( 'NONE',  ( -55.12499999999997868, 1.184343223768590692, 3.558065644182724530 ) ) ;
#12472 = CIRCLE ( 'NONE', #16541, 0.1000000000000002970 ) ;
#12473 = DIRECTION ( 'NONE',  ( 0.000000000000000000, -0.9985773570673280863, 0.05332224631830469186 ) ) ;
#12474 = FACE_OUTER_BOUND ( 'NONE', #6204, .T. ) ;
#12475 = CIRCLE ( 'NONE', #31205, 4.500000000000037303 ) ;
#12476 = CIRCLE ( 'NONE', #27150, 3.399999999999999911 ) ;
#12477 = CARTESIAN_POINT ( 'NONE',  ( 51.80000000000001137, 6.475000000000062705, -1.950000000000180256 ) ) ;
#12478 = ORIENTED_EDGE ( 'NONE', *, *, #686, .T. ) ;
#12479 = EDGE_CURVE ( 'NONE', #26012, #21420, #10978, .T. ) ;
#12480 = DIRECTION ( 'NONE',  ( -1.000000000000000000, -1.047444401652940007E-14, -0.000000000000000000 ) ) ;
#12481 = AXIS2_PLACEMENT_3D ( 'NONE', #14584, #2560, #27928 ) ;
#12482 = CARTESIAN_POINT ( 'NONE',  ( 31.68228470681282971, 7.543995930034753883, -1.950000000000109868 ) ) ;
#12483 = CIRCLE ( 'NONE', #1871, 2.114644660940672605 ) ;
#12484 = DIRECTION ( 'NONE',  ( 1.000000000000000000, -1.219044193948983948E-29, 3.491481338843133355E-15 ) ) ;
#12485 = CIRCLE ( 'NONE', #365, 1.679509022399086948 ) ;
#12486 = PLANE ( 'NONE',  #5341 ) ;
#12487 = EDGE_CURVE ( 'NONE', #29731, #1382, #24088, .T. ) ;
#12488 = DIRECTION ( 'NONE',  ( 0.000000000000000000, -0.9996898646859343485, -0.02490330187381124133 ) ) ;
#12490 = CARTESIAN_POINT ( 'NONE',  ( 28.44937284992260729, 5.648694717987689629, 1.424999999999900790 ) ) ;
#12489 = CARTESIAN_POINT ( 'NONE',  ( 51.15311061045468222, 0.9578955620007181260, 1.386733222354203487 ) ) ;
#12491 = ORIENTED_EDGE ( 'NONE', *, *, #11583, .F. ) ;
#12492 = CIRCLE ( 'NONE', #25141, 0.1500000000000001887 ) ;
#12493 = CARTESIAN_POINT ( 'NONE',  ( -71.44999999999998863, -0.4118376219176019259, 2.008205610283286813 ) ) ;
#12494 = ORIENTED_EDGE ( 'NONE', *, *, #10358, .T. ) ;
#12495 = TOROIDAL_SURFACE ( 'NONE', #2908, 2.649999999999999911, 0.05000000000000000278 ) ;
#12496 = CARTESIAN_POINT ( 'NONE',  ( -59.69999999999997442, 8.366749974758454467E-15, -2.120534355533670266E-13 ) ) ;
#12498 = CARTESIAN_POINT ( 'NONE',  ( -44.59999999999996589, -1.399999999999979261, -3.959797974644847507 ) ) ;
#12497 = CARTESIAN_POINT ( 'NONE',  ( -54.46614378277664059, -2.255560380866761250, -2.805788190199900889 ) ) ;
#12499 = CARTESIAN_POINT ( 'NONE',  ( 50.22478246037405825, 8.164214000976988572, -1.950000000000174483 ) ) ;
#12500 = ORIENTED_EDGE ( 'NONE', *, *, #14263, .F. ) ;
#12501 = ORIENTED_EDGE ( 'NONE', *, *, #28716, .T. ) ;
#12502 = DIRECTION ( 'NONE',  ( 1.000000000000000000, 1.047444401652940007E-14, 0.000000000000000000 ) ) ;
#12503 = ADVANCED_FACE ( 'NONE', ( #9544 ), #23100, .T. ) ;
#12504 = CARTESIAN_POINT ( 'NONE',  ( 47.86726169791864294, -4.031600731908413948, 1.173113608511507255 ) ) ;
#12505 = ORIENTED_EDGE ( 'NONE', *, *, #30506, .T. ) ;
#12506 = CARTESIAN_POINT ( 'NONE',  ( 69.20000000000001705, -0.7500000000000000000, -1.988246715074082793 ) ) ;
#12507 = EDGE_CURVE ( 'NONE', #7079, #25398, #22124, .T. ) ;
#12508 = CARTESIAN_POINT ( 'NONE',  ( -55.61042740578361077, -0.7887156198831598575, 3.845940847736173840 ) ) ;
#12509 = CIRCLE ( 'NONE', #23654, 2.600000000000000089 ) ;
#12510 = EDGE_CURVE ( 'NONE', #21772, #19129, #23630, .T. ) ;
#12511 = CARTESIAN_POINT ( 'NONE',  ( -36.27260443516959043, -5.005099703116284715, -1.423440526321894328 ) ) ;
#12512 = ORIENTED_EDGE ( 'NONE', *, *, #16390, .F. ) ;
#12513 = DIRECTION ( 'NONE',  ( 1.000000000000000000, 0.000000000000000000, 0.000000000000000000 ) ) ;
#12514 = CIRCLE ( 'NONE', #17080, 0.1500000000000001887 ) ;
#12515 = CYLINDRICAL_SURFACE ( 'NONE', #24037, 0.1000000000000002554 ) ;
#12516 = CIRCLE ( 'NONE', #23661, 1.875000000000001776 ) ;
#12517 =( LENGTH_UNIT ( ) NAMED_UNIT ( * ) SI_UNIT ( .MILLI., .METRE. ) );
#12518 = EDGE_LOOP ( 'NONE', ( #29788, #29404, #4804, #15564, #4607, #2621, #13372, #27094 ) ) ;
#12519 = VECTOR ( 'NONE', #19593, 1000.000000000000000 ) ;
#12520 = CARTESIAN_POINT ( 'NONE',  ( -58.38452994616204705, -3.117691453623976816, 1.799999999999780442 ) ) ;
#12521 = DIRECTION ( 'NONE',  ( 0.000000000000000000, -0.9996898646859344595, -0.02490330187381124133 ) ) ;
#12522 = CARTESIAN_POINT ( 'NONE',  ( 48.38577482684819131, -1.132063507975290095, -3.941224428058327511 ) ) ;
#12523 = DIRECTION ( 'NONE',  ( 0.000000000000000000, 0.000000000000000000, 1.000000000000000000 ) ) ;
#12524 = CARTESIAN_POINT ( 'NONE',  ( 51.78960940689399450, -4.157292525004591788, -1.048498855808313035 ) ) ;
#12526 = CARTESIAN_POINT ( 'NONE',  ( -36.56242893520685300, -0.2143423494565226961, -5.404929114625703690 ) ) ;
#12525 = DIRECTION ( 'NONE',  ( 1.000000000000000000, 0.000000000000000000, -3.491481338843133355E-15 ) ) ;
#12527 = EDGE_CURVE ( 'NONE', #24542, #25083, #23131, .T. ) ;
#12528 = AXIS2_PLACEMENT_3D ( 'NONE', #15895, #25253, #5782 ) ;
#12529 = LINE ( 'NONE', #30684, #30672 ) ;
#12530 = CARTESIAN_POINT ( 'NONE',  ( 69.25000000000000000, 0.7500000000000000000, -1.988246715074081905 ) ) ;
#12532 = CARTESIAN_POINT ( 'NONE',  ( 57.05000000000002558, -0.7500000000000000000, 2.490438859776669123 ) ) ;
#12531 = CARTESIAN_POINT ( 'NONE',  ( 54.50000000000002132, -0.003160834336494982005, -4.277587663180611344 ) ) ;
#12533 = ORIENTED_EDGE ( 'NONE', *, *, #26718, .F. ) ;
#12534 = DIRECTION ( 'NONE',  ( -3.002035892788117459E-16, 0.9996898646859344595, 0.02490330187381124133 ) ) ;
#12535 = EDGE_CURVE ( 'NONE', #18823, #26062, #630, .T. ) ;
#12536 = CARTESIAN_POINT ( 'NONE',  ( 69.20000000000004547, -0.6441176470588234615, 1.707553061179923892 ) ) ;
#12538 = DIRECTION ( 'NONE',  ( -1.047444401652940007E-14, 0.000000000000000000, -1.000000000000000000 ) ) ;
#12537 = CARTESIAN_POINT ( 'NONE',  ( 15.17214319754864427, 3.426725954212534120, -3.937891351789542416 ) ) ;
#12539 = DIRECTION ( 'NONE',  ( -1.000000000000000000, -0.000000000000000000, -0.000000000000000000 ) ) ;
#12540 = ORIENTED_EDGE ( 'NONE', *, *, #1078, .T. ) ;
#12541 = CARTESIAN_POINT ( 'NONE',  ( -61.37927097740655569, -2.651043540278919419, 0.4875364716318860703 ) ) ;
#12542 = EDGE_LOOP ( 'NONE', ( #27314, #16360, #2860, #12184 ) ) ;
#12543 = CARTESIAN_POINT ( 'NONE',  ( 51.70000000000001705, -3.826179070414207573, 1.000000000000000222 ) ) ;
#12544 = VERTEX_POINT ( 'NONE', #3325 ) ;
#12545 = EDGE_LOOP ( 'NONE', ( #24322, #26187, #16409, #29338 ) ) ;
#12546 = EDGE_CURVE ( 'NONE', #4809, #10712, #27661, .T. ) ;
#12547 = DIRECTION ( 'NONE',  ( 0.000000000000000000, -0.2008964009354162750, 0.9796124928211136229 ) ) ;
#12548 = ORIENTED_EDGE ( 'NONE', *, *, #12439, .F. ) ;
#12549 = DIRECTION ( 'NONE',  ( -1.000000000000000000, -0.000000000000000000, -0.000000000000000000 ) ) ;
#12550 = CARTESIAN_POINT ( 'NONE',  ( -59.88452994616203995, -3.117691453623976816, 1.799999999999775335 ) ) ;
#12551 = EDGE_LOOP ( 'NONE', ( #2682, #24927, #16484 ) ) ;
#12552 = DIRECTION ( 'NONE',  ( 0.000000000000000000, -1.000000000000000000, 0.000000000000000000 ) ) ;
#12553 = LINE ( 'NONE', #21789, #21302 ) ;
#12554 = AXIS2_PLACEMENT_3D ( 'NONE', #19344, #17262, #9987 ) ;
#12555 = LINE ( 'NONE', #24590, #15396 ) ;
#12556 = ORIENTED_EDGE ( 'NONE', *, *, #17031, .T. ) ;
#12557 =( GEOMETRIC_REPRESENTATION_CONTEXT ( 3 ) GLOBAL_UNCERTAINTY_ASSIGNED_CONTEXT ( ( #28834 ) ) GLOBAL_UNIT_ASSIGNED_CONTEXT ( ( #1294, #1757, #14117 ) ) REPRESENTATION_CONTEXT ( 'NONE', 'WORKASPACE' ) );
#12558 = CARTESIAN_POINT ( 'NONE',  ( 51.72219788184018086, -4.178381389434671078, -1.001886780333043125 ) ) ;
#12559 = CARTESIAN_POINT ( 'NONE',  ( -35.85663232820583346, -4.383220986679603470, -0.4611378927910509407 ) ) ;
#12560 = DIRECTION ( 'NONE',  ( 0.000000000000000000, 0.8381322357049212357, 0.5454670984324081484 ) ) ;
#12561 = CARTESIAN_POINT ( 'NONE',  ( 56.95000000000001705, -0.7137254901960785602, -2.500119182087999548 ) ) ;
#12562 = CARTESIAN_POINT ( 'NONE',  ( 57.01550456668461209, -0.7366124869942373143, 2.429953032873097829 ) ) ;
#12564 = DIRECTION ( 'NONE',  ( 0.000000000000000000, 0.000000000000000000, 1.000000000000000000 ) ) ;
#12563 = CARTESIAN_POINT ( 'NONE',  ( -36.23324115033521053, -3.272294129011612540, 4.050092634494196098 ) ) ;
#12565 = EDGE_CURVE ( 'NONE', #28405, #29835, #1372, .T. ) ;
#12566 = CARTESIAN_POINT ( 'NONE',  ( 58.66054497608116947, -0.4999999999856035160, 1.807104036853935503 ) ) ;
#12567 = EDGE_CURVE ( 'NONE', #20708, #25749, #1817, .T. ) ;
#12568 = CARTESIAN_POINT ( 'NONE',  ( 69.20000000000004547, -0.7500000000000000000, 1.988246715072631732 ) ) ;
#12569 = CARTESIAN_POINT ( 'NONE',  ( -54.49865678108456279, 1.537045020190657585, -3.323865043138458208 ) ) ;
#12570 = CARTESIAN_POINT ( 'NONE',  ( 51.39453088482485299, 4.389042235173730155, 2.049999999999819966 ) ) ;
#12571 = EDGE_CURVE ( 'NONE', #13230, #6307, #29442, .T. ) ;
#12572 = ORIENTED_EDGE ( 'NONE', *, *, #14624, .F. ) ;
#12573 = COLOUR_RGB ( '', 0.09019608, 0.27058824, 0.51372549) ;
#12574 = EDGE_LOOP ( 'NONE', ( #16883, #6193, #23633, #9022 ) ) ;
#12575 = CIRCLE ( 'NONE', #19193, 1.000000000000000000 ) ;
#12576 = ORIENTED_EDGE ( 'NONE', *, *, #29439, .F. ) ;
#12577 = CARTESIAN_POINT ( 'NONE',  ( -59.16647130186552772, 2.362152846858203592, 1.255950301266114622 ) ) ;
#12578 = PRODUCT_DEFINITION_SHAPE ( 'NONE', 'NONE',  #17468 ) ;
#12579 = CARTESIAN_POINT ( 'NONE',  ( -60.61042740578359656, -2.936324665650201560, -2.606018187048497303 ) ) ;
#12581 = CARTESIAN_POINT ( 'NONE',  ( 58.75000000000000711, 1.323060376182032760, -1.499837071477343242 ) ) ;
#12580 = FACE_OUTER_BOUND ( 'NONE', #14501, .T. ) ;
#12582 = VERTEX_POINT ( 'NONE', #22489 ) ;
#12583 = ORIENTED_EDGE ( 'NONE', *, *, #6084, .F. ) ;
#12584 = CARTESIAN_POINT ( 'NONE',  ( 54.15033848193498756, 6.694122911624470262, -2.050000000000185008 ) ) ;
#12585 = ORIENTED_EDGE ( 'NONE', *, *, #26718, .T. ) ;
#12586 = EDGE_CURVE ( 'NONE', #10094, #11116, #24394, .T. ) ;
#12587 = DIRECTION ( 'NONE',  ( 0.000000000000000000, 0.000000000000000000, -1.000000000000000000 ) ) ;
#12588 = ORIENTED_EDGE ( 'NONE', *, *, #12188, .T. ) ;
#12589 = CARTESIAN_POINT ( 'NONE',  ( 32.57869118458719981, 7.908463456459825736, -1.950000000000176925 ) ) ;
#12590 = ORIENTED_EDGE ( 'NONE', *, *, #4470, .T. ) ;
#12591 = CARTESIAN_POINT ( 'NONE',  ( -57.11505354137801049, 3.400000000000011902, -0.9110272542660005080 ) ) ;
#12592 = AXIS2_PLACEMENT_3D ( 'NONE', #5486, #16464, #9671 ) ;
#12593 = CARTESIAN_POINT ( 'NONE',  ( 47.10000000000002984, -3.550773357292059007, 2.049880134335656745 ) ) ;
#12594 = ORIENTED_EDGE ( 'NONE', *, *, #331, .F. ) ;
#12595 = CARTESIAN_POINT ( 'NONE',  ( 15.41586008885046866, -5.027926281937888042, -1.353187539902112491 ) ) ;
#12596 = CARTESIAN_POINT ( 'NONE',  ( -60.00952994616204705, -4.643455692769866465E-15, 3.599999999999786038 ) ) ;
#12597 = CARTESIAN_POINT ( 'NONE',  ( 53.04927178323139714, 4.171861402708406885, -2.050000000000185008 ) ) ;
#12598 = CARTESIAN_POINT ( 'NONE',  ( 58.66133336607619952, 1.819551968141050136, 0.4538287010067406646 ) ) ;
#12599 = AXIS2_PLACEMENT_3D ( 'NONE', #27417, #10942, #17923 ) ;
#12600 = CARTESIAN_POINT ( 'NONE',  ( 48.30000000000001847, 0.6462379109120995890, -4.048750000000023164 ) ) ;
#12601 = CYLINDRICAL_SURFACE ( 'NONE', #11468, 1.000000000000000000 ) ;
#12602 = CARTESIAN_POINT ( 'NONE',  ( 50.40896409817930390, 1.199904535326282495, -3.921111011342365504 ) ) ;
#12603 = DIRECTION ( 'NONE',  ( 0.000000000000000000, 0.000000000000000000, 1.000000000000000000 ) ) ;
#12604 = ADVANCED_FACE ( 'NONE', ( #5550 ), #27065, .T. ) ;
#12605 = DIRECTION ( 'NONE',  ( 0.000000000000000000, 0.000000000000000000, -1.000000000000000000 ) ) ;
#12606 = EDGE_CURVE ( 'NONE', #12299, #26302, #18432, .T. ) ;
#12607 = ORIENTED_EDGE ( 'NONE', *, *, #17537, .T. ) ;
#12608 = FACE_OUTER_BOUND ( 'NONE', #20543, .T. ) ;
#12609 = CARTESIAN_POINT ( 'NONE',  ( 51.49777277048506363, -1.059151787767940389, -1.232523824083111563 ) ) ;
#12610 = CARTESIAN_POINT ( 'NONE',  ( 54.41366571437522737, 6.718673005292168376, 1.963089969304595783 ) ) ;
#12611 = ORIENTED_EDGE ( 'NONE', *, *, #147, .F. ) ;
#12612 = CARTESIAN_POINT ( 'NONE',  ( 58.75000000000003553, -1.666164585742988091, 1.106298139390331947 ) ) ;
#12613 = EDGE_LOOP ( 'NONE', ( #29641, #29301, #29190, #23958 ) ) ;
#12614 = CARTESIAN_POINT ( 'NONE',  ( -62.34999999999997300, 1.091670395932995432E-15, 2.248789515065420326E-15 ) ) ;
#12615 = CARTESIAN_POINT ( 'NONE',  ( -35.85663232820584057, -0.4576450603547173035, -5.200000000000000178 ) ) ;
#12617 = DIRECTION ( 'NONE',  ( 1.000000000000000000, 1.047444401652940007E-14, 0.000000000000000000 ) ) ;
#12616 = CARTESIAN_POINT ( 'NONE',  ( 61.25000000000002132, 6.415596960124259844E-13, 3.111507638930570854E-58 ) ) ;
#12618 = ORIENTED_EDGE ( 'NONE', *, *, #8979, .F. ) ;
#12619 = VECTOR ( 'NONE', #16443, 1000.000000000000000 ) ;
#12620 = EDGE_CURVE ( 'NONE', #4687, #9856, #29148, .T. ) ;
#12621 = DIRECTION ( 'NONE',  ( 0.000000000000000000, -0.9996898646859343485, -0.02490330187381123786 ) ) ;
#12622 = CIRCLE ( 'NONE', #30323, 0.1499999999999999667 ) ;
#12623 = VERTEX_POINT ( 'NONE', #22033 ) ;
#12625 = DIRECTION ( 'NONE',  ( 1.000000000000000000, 1.047444401652940007E-14, -0.000000000000000000 ) ) ;
#12624 = CARTESIAN_POINT ( 'NONE',  ( 52.79223755100147741, 4.124864650457799264, 2.046664448805795011 ) ) ;
#12626 = CARTESIAN_POINT ( 'NONE',  ( 34.56702326949724835, 8.213851659285209550, -2.050000000000119726 ) ) ;
#12627 = CARTESIAN_POINT ( 'NONE',  ( -60.18749999999997158, -4.108500314926507357, 1.367561758111407011 ) ) ;
#12628 = CARTESIAN_POINT ( 'NONE',  ( -71.49999999999998579, 0.4218824419643696921, -2.057186234924337054 ) ) ;
#12629 = LINE ( 'NONE', #22314, #3253 ) ;
#12630 = CIRCLE ( 'NONE', #24771, 4.500000000000037303 ) ;
#12631 = CARTESIAN_POINT ( 'NONE',  ( 69.20000000000004547, 0.6617647058823536987, 1.754335336828709346 ) ) ;
#12632 = CYLINDRICAL_SURFACE ( 'NONE', #9708, 2.624999999999998668 ) ;
#12633 = CARTESIAN_POINT ( 'NONE',  ( -63.86464466094066239, -2.684522515537854925, -0.06687421464704190743 ) ) ;
#12634 = CARTESIAN_POINT ( 'NONE',  ( 15.59140265158956318, -0.9780988077348131693, 5.318542208600381294 ) ) ;
#12635 = ORIENTED_EDGE ( 'NONE', *, *, #13473, .F. ) ;
#12636 = CIRCLE ( 'NONE', #1519, 0.1000000000000000472 ) ;
#12637 = CARTESIAN_POINT ( 'NONE',  ( 15.61552784268253724, -2.776541361170953515, 4.646985486732154946 ) ) ;
#12638 = CARTESIAN_POINT ( 'NONE',  ( -62.06644497648784409, -2.658467779542562859, 0.2005540737866994272 ) ) ;
#12639 = EDGE_CURVE ( 'NONE', #11417, #8120, #1868, .T. ) ;
#12640 = DIRECTION ( 'NONE',  ( -1.000000000000000000, -0.000000000000000000, -0.000000000000000000 ) ) ;
#12641 = CARTESIAN_POINT ( 'NONE',  ( -58.00952994616203284, 3.117691453623999021, -1.800000000000183897 ) ) ;
#12642 = DIRECTION ( 'NONE',  ( 0.000000000000000000, -0.9996898646859344595, -0.02490330187381124827 ) ) ;
#12643 = CARTESIAN_POINT ( 'NONE',  ( 23.92596721145586258, 5.813591174092887393, 2.049999999999916334 ) ) ;
#12644 = ORIENTED_EDGE ( 'NONE', *, *, #2782, .F. ) ;
#12645 = CARTESIAN_POINT ( 'NONE',  ( 68.00000000000004263, -0.6617647058823529216, 1.754335336828721337 ) ) ;
#12646 = ORIENTED_EDGE ( 'NONE', *, *, #711, .T. ) ;
#12647 = UNCERTAINTY_MEASURE_WITH_UNIT (LENGTH_MEASURE( 1.000000000000000082E-05 ), #8744, 'distance_accuracy_value', 'NONE');
#12648 = DIRECTION ( 'NONE',  ( 1.000000000000000000, 1.047444401652940007E-14, 0.000000000000000000 ) ) ;
#12650 = DIRECTION ( 'NONE',  ( -1.015447888376667464E-14, 0.000000000000000000, -1.000000000000000000 ) ) ;
#12649 = CARTESIAN_POINT ( 'NONE',  ( 16.07512358269907082, -3.430438802933840403, -4.182416543699102540 ) ) ;
#12651 = ORIENTED_EDGE ( 'NONE', *, *, #1811, .T. ) ;
#12652 = ORIENTED_EDGE ( 'NONE', *, *, #2821, .F. ) ;
#12653 = CARTESIAN_POINT ( 'NONE',  ( 69.20000000000003126, 4.557543281186736018E-17, -7.248315259438346108E-13 ) ) ;
#12654 = EDGE_CURVE ( 'NONE', #23979, #5992, #29536, .T. ) ;
#12655 = CARTESIAN_POINT ( 'NONE',  ( 48.00000000000002132, -4.031600731908413948, 1.173113608511506367 ) ) ;
#12656 =( BOUNDED_SURFACE ( )  B_SPLINE_SURFACE ( 3, 2, ( 
 ( #12196, #21875, #9978 ),
 ( #162, #7601, #26899 ),
 ( #5211, #24522, #14859 ),
 ( #19944, #27517, #13256 ) ),
 .UNSPECIFIED., .F., .F., .F. ) 
 B_SPLINE_SURFACE_WITH_KNOTS ( ( 4, 4 ),
 ( 3, 3 ),
 ( 0.0001706658715695485952, 0.0002755376070443638472 ),
 ( 0.000000000000000000, 1.000000000000000000 ),
 .UNSPECIFIED. ) 
 GEOMETRIC_REPRESENTATION_ITEM ( )  RATIONAL_B_SPLINE_SURFACE ( (
 ( 1.000000000000000000, 0.7071067811865487940, 1.000000000000000000),
 ( 1.000000000000000000, 0.7664791242981755515, 1.000000000000000000),
 ( 1.000000000000000000, 0.8546216002033862891, 1.000000000000000000),
 ( 1.000000000000000000, 0.8543839179668213379, 1.000000000000000000) ) ) 
 REPRESENTATION_ITEM ( '' )  SURFACE ( )  );
#12657 = ORIENTED_EDGE ( 'NONE', *, *, #29717, .T. ) ;
#12659 = DIRECTION ( 'NONE',  ( 0.000000000000000000, 0.000000000000000000, 1.000000000000000000 ) ) ;
#12658 = CARTESIAN_POINT ( 'NONE',  ( -58.32202994616204705, -4.156921938165296204, -2.220106322563329850E-13 ) ) ;
#12660 = DIRECTION ( 'NONE',  ( -1.000000000000000000, -0.000000000000000000, -0.000000000000000000 ) ) ;
#12661 = CARTESIAN_POINT ( 'NONE',  ( -36.89250464418362441, -5.037778396015640148, -1.970103387723705080 ) ) ;
#12662 =( NAMED_UNIT ( * ) SI_UNIT ( $, .STERADIAN. ) SOLID_ANGLE_UNIT ( ) );
#12663 = CARTESIAN_POINT ( 'NONE',  ( 58.65000045311413857, -1.265716300431979358, -1.383426348886848123 ) ) ;
#12664 = FILL_AREA_STYLE_COLOUR ( '', #26751 ) ;
#12665 = EDGE_CURVE ( 'NONE', #13977, #13894, #25612, .T. ) ;
#12666 = ORIENTED_EDGE ( 'NONE', *, *, #18779, .F. ) ;
#12667 = AXIS2_PLACEMENT_3D ( 'NONE', #29483, #22385, #17638 ) ;
#12668 = CARTESIAN_POINT ( 'NONE',  ( -58.25952994616203284, -3.117691453623963938, -1.800000000000218092 ) ) ;
#12669 = CARTESIAN_POINT ( 'NONE',  ( -59.69999999999997442, 3.400000000000007905, -2.001823990013003858E-13 ) ) ;
#12670 = CARTESIAN_POINT ( 'NONE',  ( 48.42250533816334013, -1.328329461116573684, -3.879000873601222477 ) ) ;
#12671 = CARTESIAN_POINT ( 'NONE',  ( 15.56274145962601807, -1.026563698233271538, 5.312790900508115755 ) ) ;
#12672 = DIRECTION ( 'NONE',  ( 0.000000000000000000, -0.9996898646859343485, -0.02490330187381124133 ) ) ;
#12673 = CARTESIAN_POINT ( 'NONE',  ( -57.08155989232412963, 3.400000000000007905, -1.873796572744660248E-13 ) ) ;
#12674 = ADVANCED_FACE ( 'NONE', ( #6176 ), #855, .F. ) ;
#12676 = CARTESIAN_POINT ( 'NONE',  ( -36.04518387042617888, -0.7747498539018073949, -5.363501450340010024 ) ) ;
#12675 = FACE_OUTER_BOUND ( 'NONE', #8405, .T. ) ;
#12677 = EDGE_CURVE ( 'NONE', #14419, #20749, #30381, .T. ) ;
#12678 = EDGE_CURVE ( 'NONE', #10332, #19277, #25125, .T. ) ;
#12679 = DIRECTION ( 'NONE',  ( 1.000000000000000000, 1.047444401652940007E-14, -0.000000000000000000 ) ) ;
#12680 = CARTESIAN_POINT ( 'NONE',  ( 52.06628335902944826, 0.5434431642986571331, -1.794517909405660694 ) ) ;
#12682 = CARTESIAN_POINT ( 'NONE',  ( 56.99368740573074632, -0.8156852809530760195, 2.468736017162952656 ) ) ;
#12681 = CARTESIAN_POINT ( 'NONE',  ( 54.46244440770933437, -0.0007103938888845436886, -4.353106894003209604 ) ) ;
#12683 = ORIENTED_EDGE ( 'NONE', *, *, #28491, .F. ) ;
#12684 = B_SPLINE_CURVE_WITH_KNOTS ( 'NONE', 3,
 ( #26272, #26424, #21534, #2528, #19170, #14702, #11857, #12177, #21997, #23900, #26884, #28810, #2359 ),
 .UNSPECIFIED., .F., .F.,
 ( 4, 3, 3, 3, 4 ),
 ( 0.000000000000000000, 4.994367907427477767E-05, 9.982969917209731626E-05, 0.0001505119896697553904, 0.0001857353029114525904 ),
 .UNSPECIFIED. ) ;
#12685 = CARTESIAN_POINT ( 'NONE',  ( 50.29999999999649418, -1.426739617988837194, -3.843749999997122746 ) ) ;
#12686 = CARTESIAN_POINT ( 'NONE',  ( -36.40878371307407946, -5.360483378448159364, -0.7132926830812800212 ) ) ;
#12688 = CARTESIAN_POINT ( 'NONE',  ( 52.71963143566818388, 4.013862682579961927, 0.8481297820164899193 ) ) ;
#12687 = CARTESIAN_POINT ( 'NONE',  ( 15.30042582489635095, 2.199885882961221562, -4.939696253591084663 ) ) ;
#12689 = CARTESIAN_POINT ( 'NONE',  ( 56.95000081403880188, 0.7675332364161941978, 2.484758330364432943 ) ) ;
#12690 = ORIENTED_EDGE ( 'NONE', *, *, #4217, .F. ) ;
#12691 = DIRECTION ( 'NONE',  ( 0.000000000000000000, 0.2008964009354141933, -0.9796124928211140670 ) ) ;
#12692 = CARTESIAN_POINT ( 'NONE',  ( 47.06748821295592933, -4.176834854957374610, 1.005432649909180132 ) ) ;
#12693 = EDGE_CURVE ( 'NONE', #5591, #26849, #19096, .T. ) ;
#12694 = ORIENTED_EDGE ( 'NONE', *, *, #5356, .T. ) ;
#12695 = DIRECTION ( 'NONE',  ( 3.002035892788117459E-16, -0.9996898646859343485, -0.02490330187381124480 ) ) ;
#12696 = ORIENTED_EDGE ( 'NONE', *, *, #14849, .T. ) ;
#12697 = VERTEX_POINT ( 'NONE', #15969 ) ;
#12698 = CARTESIAN_POINT ( 'NONE',  ( 15.32752150720752837, 4.698781674909530359, -2.676750094560090165 ) ) ;
#12699 = ORIENTED_EDGE ( 'NONE', *, *, #502, .T. ) ;
#12700 = CARTESIAN_POINT ( 'NONE',  ( 30.14940651961542528, 6.652605095929053469, 1.949999999999894706 ) ) ;
#12701 = CARTESIAN_POINT ( 'NONE',  ( -60.94702994616203995, 4.156921938165313080, -2.011299877933566609E-13 ) ) ;
#12702 = ORIENTED_EDGE ( 'NONE', *, *, #28233, .T. ) ;
#12703 = CARTESIAN_POINT ( 'NONE',  ( 61.23770293222996486, -0.8897917884435792013, -1.791164585742600179 ) ) ;
#12704 = ORIENTED_EDGE ( 'NONE', *, *, #9624, .F. ) ;
#12705 = DIRECTION ( 'NONE',  ( -1.000000000000000000, -2.586136946169074517E-16, 0.000000000000000000 ) ) ;
#12706 = EDGE_CURVE ( 'NONE', #28363, #4064, #30232, .T. ) ;
#12707 = CARTESIAN_POINT ( 'NONE',  ( 24.79111845547922499, 5.500805180497224889, 2.049999999999913225 ) ) ;
#12708 = ORIENTED_EDGE ( 'NONE', *, *, #27206, .F. ) ;
#12709 = AXIS2_PLACEMENT_3D ( 'NONE', #1853, #15654, #25299 ) ;
#12710 = CARTESIAN_POINT ( 'NONE',  ( 60.75000000000001421, 0.6500000000006362910, 1.489337100860648189 ) ) ;
#12711 = ADVANCED_FACE ( 'NONE', ( #10612 ), #20290, .T. ) ;
#12712 = CARTESIAN_POINT ( 'NONE',  ( 54.18071634157380601, 6.868323337799980166, -2.050000000000189448 ) ) ;
#12713 = DIRECTION ( 'NONE',  ( 1.000000000000000000, 1.047444401652940007E-14, 0.000000000000000000 ) ) ;
#12714 = DIRECTION ( 'NONE',  ( 0.000000000000000000, -0.9996898646859344595, -0.02490330187381124480 ) ) ;
#12715 = CARTESIAN_POINT ( 'NONE',  ( 51.31572262954149721, 1.002608958138273554, 1.395204572094392192 ) ) ;
#12717 = DIRECTION ( 'NONE',  ( 0.000000000000000000, 0.000000000000000000, -1.000000000000000000 ) ) ;
#12716 = DIRECTION ( 'NONE',  ( -3.696862594069216125E-15, 0.9356455129756975353, -0.3529411764705897570 ) ) ;
#12718 = EDGE_CURVE ( 'NONE', #1734, #1808, #19598, .T. ) ;
#12719 = ADVANCED_BREP_SHAPE_REPRESENTATION ( '', ( #5173, #9018 ), #23745 ) ;
#12720 = ADVANCED_FACE ( 'NONE', ( #29919 ), #22959, .T. ) ;
#12721 = CARTESIAN_POINT ( 'NONE',  ( 50.40811050917465508, -1.340787288841403635, -3.874691554877328858 ) ) ;
#12722 = CARTESIAN_POINT ( 'NONE',  ( -60.49999999999997868, -2.624185894800576513, -0.06537116741875401149 ) ) ;
#12723 = CARTESIAN_POINT ( 'NONE',  ( 58.65838214097848891, 1.301971553120403025, -1.349359547238234036 ) ) ;
#12724 = VECTOR ( 'NONE', #5753, 1000.000000000000000 ) ;
#12725 = CARTESIAN_POINT ( 'NONE',  ( 51.80000000000001847, -1.084202172485504434E-16, 4.374999999999999112 ) ) ;
#12726 = EDGE_LOOP ( 'NONE', ( #706, #16064, #6237, #11290 ) ) ;
#12727 = CARTESIAN_POINT ( 'NONE',  ( -59.69999999999997442, -3.399999999999991473, -2.235080921937235780E-13 ) ) ;
#12728 = ORIENTED_EDGE ( 'NONE', *, *, #18537, .F. ) ;
#12729 = CIRCLE ( 'NONE', #2119, 0.1000000000000000472 ) ;
#12730 = VERTEX_POINT ( 'NONE', #10757 ) ;
#12731 = CARTESIAN_POINT ( 'NONE',  ( -62.07633557594488849, -2.504645164848317673, -0.3199649952759585636 ) ) ;
#12732 = CARTESIAN_POINT ( 'NONE',  ( -58.61042740578358945, -0.7887156198831605236, 3.845940847736174284 ) ) ;
#12734 = DIRECTION ( 'NONE',  ( 0.000000000000000000, 0.000000000000000000, -1.000000000000000000 ) ) ;
#12733 = DIRECTION ( 'NONE',  ( 1.000000000000000000, 0.000000000000000000, 0.000000000000000000 ) ) ;
#12735 = ORIENTED_EDGE ( 'NONE', *, *, #15624, .T. ) ;
#12736 = EDGE_LOOP ( 'NONE', ( #14224, #14835, #21442, #26235, #28832 ) ) ;
#12737 = CARTESIAN_POINT ( 'NONE',  ( 53.99324464492229225, 6.679476996055688787, -1.975347834873397490 ) ) ;
#12738 = ORIENTED_EDGE ( 'NONE', *, *, #2186, .F. ) ;
#12739 = FACE_OUTER_BOUND ( 'NONE', #3772, .T. ) ;
#12740 = ORIENTED_EDGE ( 'NONE', *, *, #20652, .F. ) ;
#12741 = CARTESIAN_POINT ( 'NONE',  ( 26.61241883252577978, 5.319505464261553129, -2.050000000000092193 ) ) ;
#12742 = ADVANCED_FACE ( 'NONE', ( #8229 ), #8540, .F. ) ;
#12743 = CARTESIAN_POINT ( 'NONE',  ( -58.81249999999996447, 3.400000000000008349, -1.915049148454697437E-13 ) ) ;
#12744 = ORIENTED_EDGE ( 'NONE', *, *, #21512, .T. ) ;
#12745 = EDGE_CURVE ( 'NONE', #19589, #25687, #18225, .T. ) ;
#12746 = B_SPLINE_CURVE_WITH_KNOTS ( 'NONE', 3,
 ( #285, #29885, #748, #24818, #19629, #7872, #9954, #7719, #17240, #17712, #22157, #15316, #14838, #12624, #594, #17549, #27354, #24961, #24499, #26880, #2810, #3287 ),
 .UNSPECIFIED., .F., .F.,
 ( 4, 2, 2, 1, 1, 2, 2, 2, 2, 2, 2, 4 ),
 ( 2.427614462101942325E-07, 0.1250002124163139827, 0.1875001972437477793, 0.2187501896574692850, 0.2343751858643298436, 0.2421876839677601367, 0.2500001820711904021, 0.3750001517259984873, 0.4375001365533990882, 0.4687501289670995552, 0.5000001213808000777, 1.000000000000000000 ),
 .UNSPECIFIED. ) ;
#12747 = CARTESIAN_POINT ( 'NONE',  ( 15.98305126557417921, -4.951626736499063597, -2.174059107776757038 ) ) ;
#12748 = ADVANCED_FACE ( 'NONE', ( #27862 ), #1436, .F. ) ;
#12749 = CARTESIAN_POINT ( 'NONE',  ( -58.33155989232413674, -1.962990915244731571, 3.399999999999784528 ) ) ;
#12750 = CARTESIAN_POINT ( 'NONE',  ( 52.82099478266074755, 4.588601447596422744, -2.050000000000184119 ) ) ;
#12751 = FACE_OUTER_BOUND ( 'NONE', #30146, .T. ) ;
#12752 = CARTESIAN_POINT ( 'NONE',  ( 50.55258015808398397, 5.295040916136730406E-13, 1.177580158083963546 ) ) ;
#12753 = DIRECTION ( 'NONE',  ( 0.000000000000000000, 1.000000000000000000, -1.224646799147353207E-16 ) ) ;
#12754 = CARTESIAN_POINT ( 'NONE',  ( -36.22818246778668083, -3.722599991951390130, -3.938370952810070769 ) ) ;
#12755 = CARTESIAN_POINT ( 'NONE',  ( 58.75000000000003553, -1.877732920580702958, 0.6121634413824121879 ) ) ;
#12756 = DIRECTION ( 'NONE',  ( -1.520093157366893960E-16, 0.5877852522924802425, -0.8090169943749422332 ) ) ;
#12757 = VECTOR ( 'NONE', #19317, 1000.000000000000000 ) ;
#12758 = ORIENTED_EDGE ( 'NONE', *, *, #24333, .T. ) ;
#12759 = CARTESIAN_POINT ( 'NONE',  ( -59.29999999999996163, -1.164288416760277833, 3.283393033056293486 ) ) ;
#12760 = CARTESIAN_POINT ( 'NONE',  ( 61.21684424624547205, -0.7974861228894950527, 1.837019011345026653 ) ) ;
#12761 = CARTESIAN_POINT ( 'NONE',  ( 54.24490706950494712, 6.702939575443663145, 2.049999999999809308 ) ) ;
#12762 = VERTEX_POINT ( 'NONE', #21774 ) ;
#12763 = B_SPLINE_CURVE_WITH_KNOTS ( 'NONE', 3,
 ( #17656, #863, #5616, #13046, #15589, #23022, #8602, #15738, #27606, #15265, #22727, #20666, #5932, #13191, #3078, #1023, #5462 ),
 .UNSPECIFIED., .F., .F.,
 ( 4, 2, 2, 1, 2, 2, 2, 2, 4 ),
 ( 0.5409539115281891686, 0.5983346725871655503, 0.6270250531166537966, 0.6557154336461419319, 0.7130961947051183136, 0.7704769557640946953, 0.8278577168230711880, 0.8852384778820474587, 1.000000000000000000 ),
 .UNSPECIFIED. ) ;
#12764 = CARTESIAN_POINT ( 'NONE',  ( -59.19999999999996732, -2.569786949633424022, -0.9498634748674686934 ) ) ;
#12765 = ORIENTED_EDGE ( 'NONE', *, *, #7061, .F. ) ;
#12766 = CARTESIAN_POINT ( 'NONE',  ( 15.41586008885046155, -0.2667568399899467591, -5.200000000294864755 ) ) ;
#12767 = CARTESIAN_POINT ( 'NONE',  ( 50.25000000000003553, -1.470078920827295965, -1.470078920827526892 ) ) ;
#12768 = DIRECTION ( 'NONE',  ( -0.9993908270191184107, 0.03489949670185085034, 3.491481338843133355E-15 ) ) ;
#12769 = ORIENTED_EDGE ( 'NONE', *, *, #23398, .F. ) ;
#12770 = CARTESIAN_POINT ( 'NONE',  ( -69.22071067811863543, -0.4319272620111427874, 2.106166859565398397 ) ) ;
#12771 = LINE ( 'NONE', #17709, #3406 ) ;
#12772 = VERTEX_POINT ( 'NONE', #19314 ) ;
#12774 = CARTESIAN_POINT ( 'NONE',  ( -54.47328085509070661, -1.505517457405397774, -4.033720452520548783 ) ) ;
#12773 = CARTESIAN_POINT ( 'NONE',  ( -58.20655989232411542, -3.399999999999991029, -2.246812820714294660E-13 ) ) ;
#12775 = ORIENTED_EDGE ( 'NONE', *, *, #11865, .T. ) ;
#12776 = ORIENTED_EDGE ( 'NONE', *, *, #13915, .F. ) ;
#12777 = CARTESIAN_POINT ( 'NONE',  ( -59.56249999999996447, -0.8699069336946628761, 4.241846523238429256 ) ) ;
#12778 = CARTESIAN_POINT ( 'NONE',  ( -55.87499999999996447, 2.944486372867106905, -1.700000000000185363 ) ) ;
#12779 = EDGE_CURVE ( 'NONE', #6559, #29235, #30876, .T. ) ;
#12780 = CARTESIAN_POINT ( 'NONE',  ( -54.79806624327024167, 3.400000000000004796, 0.9110272542656339123 ) ) ;
#12781 = EDGE_CURVE ( 'NONE', #25939, #18759, #21639, .T. ) ;
#12782 = CARTESIAN_POINT ( 'NONE',  ( -59.59999999999997300, 2.337126060168390307, -1.249136413240100607 ) ) ;
#12784 = CARTESIAN_POINT ( 'NONE',  ( -54.94702994616205416, 4.156921938165313080, -1.801810997602979365E-13 ) ) ;
#12783 = CIRCLE ( 'NONE', #24918, 0.04999999999999989175 ) ;
#12785 = DIRECTION ( 'NONE',  ( 1.000000000000000000, 1.047444401652940007E-14, 0.000000000000000000 ) ) ;
#12786 = ORIENTED_EDGE ( 'NONE', *, *, #3415, .T. ) ;
#12787 = CARTESIAN_POINT ( 'NONE',  ( 15.61552784268253902, 3.561547362098769209, 4.076645242318642559 ) ) ;
#12788 = CARTESIAN_POINT ( 'NONE',  ( -60.63660384741033482, -2.513063517893788568, 0.9832629503941247018 ) ) ;
#12789 = EDGE_CURVE ( 'NONE', #3419, #3612, #29663, .T. ) ;
#12790 = DIRECTION ( 'NONE',  ( 0.000000000000000000, -1.000000000000000000, 0.000000000000000000 ) ) ;
#12791 = CARTESIAN_POINT ( 'NONE',  ( -57.69702994616205416, -2.078460969082671195, 3.599999999999778932 ) ) ;
#12792 = FACE_OUTER_BOUND ( 'NONE', #24750, .T. ) ;
#12793 = CARTESIAN_POINT ( 'NONE',  ( 48.39258289184584783, 1.342093792059667390, -3.874237195466570416 ) ) ;
#12794 = ORIENTED_EDGE ( 'NONE', *, *, #19523, .T. ) ;
#12795 = DIRECTION ( 'NONE',  ( 0.000000000000000000, -1.000000000000000000, 0.000000000000000000 ) ) ;
#12796 = VERTEX_POINT ( 'NONE', #16302 ) ;
#12797 = CYLINDRICAL_SURFACE ( 'NONE', #23202, 1.874999999999998668 ) ;
#12798 = AXIS2_PLACEMENT_3D ( 'NONE', #30051, #29753, #20277 ) ;
#12800 = CARTESIAN_POINT ( 'NONE',  ( 19.23646557533807666, -1.947877022684209034E-15, 0.000000000000000000 ) ) ;
#12799 = CARTESIAN_POINT ( 'NONE',  ( 57.03405126743467690, 0.7473881623357462312, -2.422979693216943176 ) ) ;
#12801 = AXIS2_PLACEMENT_3D ( 'NONE', #7495, #17299, #24566 ) ;
#12802 = ORIENTED_EDGE ( 'NONE', *, *, #12510, .F. ) ;
#12803 = ORIENTED_EDGE ( 'NONE', *, *, #16390, .T. ) ;
#12804 = CARTESIAN_POINT ( 'NONE',  ( 51.14630318392396902, -0.9364487020628400327, 1.503522130792752209 ) ) ;
#12805 = CARTESIAN_POINT ( 'NONE',  ( 30.08242191457678061, 7.215531071606934965, 1.424999999999894351 ) ) ;
#12806 = EDGE_LOOP ( 'NONE', ( #15187, #29119, #3675, #26382 ) ) ;
#12808 = DIRECTION ( 'NONE',  ( 1.000000000000000000, 3.053848253006669023E-16, -2.042510438544995415E-16 ) ) ;
#12807 = CARTESIAN_POINT ( 'NONE',  ( -58.38452994616204705, -3.117691453623976816, 1.799999999999780442 ) ) ;
#12809 = CARTESIAN_POINT ( 'NONE',  ( -54.54792740578361077, -1.073804522883516688, -3.225979517392336238 ) ) ;
#12810 = DIRECTION ( 'NONE',  ( 0.000000000000000000, -0.9996898646859344595, -0.02490330187381105745 ) ) ;
#12811 = EDGE_CURVE ( 'NONE', #12339, #30600, #20086, .T. ) ;
#12812 = CARTESIAN_POINT ( 'NONE',  ( 58.65263613458542835, -1.372222488449002187, -1.277852321299007610 ) ) ;
#12813 = EDGE_CURVE ( 'NONE', #21815, #23640, #28333, .T. ) ;
#12814 = ORIENTED_EDGE ( 'NONE', *, *, #12073, .F. ) ;
#12815 = CARTESIAN_POINT ( 'NONE',  ( -58.13452994616202574, 2.093608279459371404E-14, -3.600000000000206146 ) ) ;
#12816 = CARTESIAN_POINT ( 'NONE',  ( 53.12888913849683092, 4.216863368992567196, -2.050000000000185008 ) ) ;
#12817 = CARTESIAN_POINT ( 'NONE',  ( -56.51905989232411542, 2.273606599708566482E-14, -3.400000000000200640 ) ) ;
#12818 = CIRCLE ( 'NONE', #7280, 0.1000000000000000333 ) ;
#12819 = CARTESIAN_POINT ( 'NONE',  ( 15.68751737981905947, -0.3564988296780420840, 5.398869307934826445 ) ) ;
#12820 = CARTESIAN_POINT ( 'NONE',  ( 51.80000000000001847, 6.982261990806648555E-14, -1.796574372350448449E-13 ) ) ;
#12821 = ADVANCED_FACE ( 'NONE', ( #11853 ), #10461, .F. ) ;
#12823 = DIRECTION ( 'NONE',  ( 0.000000000000000000, -1.000000000000000000, 0.000000000000000000 ) ) ;
#12822 = CARTESIAN_POINT ( 'NONE',  ( 50.25000000000002842, -0.8897917884436942204, -1.791164585742600179 ) ) ;
#12824 = PRODUCT_DEFINITION_SHAPE ( 'NONE', 'NONE',  #11651 ) ;
#12825 = AXIS2_PLACEMENT_3D ( 'NONE', #5648, #17533, #18281 ) ;
#12826 = CARTESIAN_POINT ( 'NONE',  ( -62.06710100716625789, -2.517118187348250213, 0.1993515260053453086 ) ) ;
#12827 = CARTESIAN_POINT ( 'NONE',  ( 15.59055531549693896, -2.334444681449719283, 4.877899991435270977 ) ) ;
#12829 = CARTESIAN_POINT ( 'NONE',  ( 65.05000000000001137, -1.025519176787267142E-28, -6.813625832752373386E-13 ) ) ;
#12828 = CARTESIAN_POINT ( 'NONE',  ( -59.31249999999997868, -1.962990915244734236, 3.399999999999780975 ) ) ;
#12830 = ORIENTED_EDGE ( 'NONE', *, *, #9494, .F. ) ;
#12831 =( BOUNDED_CURVE ( )  B_SPLINE_CURVE ( 2, ( #17160, #15232, #3046, #29331, #29020, #14764, #22225, #24569, #17620 ),
 .UNSPECIFIED., .F., .T. ) 
 B_SPLINE_CURVE_WITH_KNOTS ( ( 3, 2, 2, 2, 3 ),
 ( 0.5277777777777777901, 0.5370370370370370905, 0.5555555555555555802, 0.5740740740740740700, 0.5833333333333333703 ),
 .UNSPECIFIED. ) 
 CURVE ( )  GEOMETRIC_REPRESENTATION_ITEM ( )  RATIONAL_B_SPLINE_CURVE ( ( 0.9330127018922194093, 0.9330127018922194093, 1.000000000000000000, 0.8660254037844387076, 1.000000000000000000, 0.8660254037844387076, 1.000000000000000000, 0.9330127018922189652, 0.9330127018922194093 ) ) 
 REPRESENTATION_ITEM ( '' )  );
#12832 = CARTESIAN_POINT ( 'NONE',  ( 50.40000000000001279, -0.6304760106459033064, -3.950000000000022826 ) ) ;
#12833 = CARTESIAN_POINT ( 'NONE',  ( -43.84599839145305111, -4.786668705877446861, 6.082865895343455568E-16 ) ) ;
#12835 = DIRECTION ( 'NONE',  ( 0.000000000000000000, 0.000000000000000000, 1.000000000000000000 ) ) ;
#12834 = CARTESIAN_POINT ( 'NONE',  ( 15.03925126672122659, 4.018128179617576734, -3.618665901676609842 ) ) ;
#12836 = CARTESIAN_POINT ( 'NONE',  ( 47.02093316935654599, -4.146898708459136884, 1.994789398600220309 ) ) ;
#12837 = ORIENTED_EDGE ( 'NONE', *, *, #23352, .T. ) ;
#12838 = DIRECTION ( 'NONE',  ( 1.282749433769087582E-30, 1.000000000000000000, 1.224646799147353207E-16 ) ) ;
#12839 = CARTESIAN_POINT ( 'NONE',  ( 47.07780211815985894, -4.178381389434672855, 1.001886780333041571 ) ) ;
#12840 = CIRCLE ( 'NONE', #17928, 3.500000000000000000 ) ;
#12841 = VERTEX_POINT ( 'NONE', #4420 ) ;
#12842 = AXIS2_PLACEMENT_3D ( 'NONE', #5038, #14370, #19311 ) ;
#12843 = CARTESIAN_POINT ( 'NONE',  ( 15.18459684427939749, -4.683225679163354194, 2.703237727951212754 ) ) ;
#12844 = VERTEX_POINT ( 'NONE', #9012 ) ;
#12845 = VERTEX_POINT ( 'NONE', #21531 ) ;
#12846 = CARTESIAN_POINT ( 'NONE',  ( -71.44999999999998863, -0.3062499654112579295, 1.493338310920507839 ) ) ;
#12847 = VERTEX_POINT ( 'NONE', #1888 ) ;
#12848 = DIRECTION ( 'NONE',  ( 0.000000000000000000, 0.3137254901960767617, -0.9495137264943732669 ) ) ;
#12849 = EDGE_CURVE ( 'NONE', #21812, #5852, #18565, .T. ) ;
#12850 = CARTESIAN_POINT ( 'NONE',  ( -55.51905989232413674, 2.944486372867092250, 1.699999999999814104 ) ) ;
#12851 = VERTEX_POINT ( 'NONE', #2041 ) ;
#12852 = DIRECTION ( 'NONE',  ( 1.344447539785323523E-44, -1.000000000000000000, -3.491481338843137300E-15 ) ) ;
#12853 = ORIENTED_EDGE ( 'NONE', *, *, #11756, .T. ) ;
#12854 = CIRCLE ( 'NONE', #14865, 3.950000000000000178 ) ;
#12855 = DIRECTION ( 'NONE',  ( 3.491481338843133355E-15, 3.491481338843133355E-15, -1.000000000000000000 ) ) ;
#12856 = EDGE_CURVE ( 'NONE', #22920, #507, #4465, .T. ) ;
#12857 = CARTESIAN_POINT ( 'NONE',  ( 23.13461596521384323, 6.279931474727747265, 2.049999999999918110 ) ) ;
#12858 = ORIENTED_EDGE ( 'NONE', *, *, #30925, .F. ) ;
#12859 = CARTESIAN_POINT ( 'NONE',  ( -54.62499999999997158, -2.944486372867076707, -1.700000000000204903 ) ) ;
#12860 = CARTESIAN_POINT ( 'NONE',  ( 61.25000000000001421, 1.000000000000641709, 1.586072192556190252 ) ) ;
#12861 = CARTESIAN_POINT ( 'NONE',  ( -54.44999999999997442, 1.549999999999999600, -4.029888335921975262 ) ) ;
#12862 = CARTESIAN_POINT ( 'NONE',  ( 36.50000000000002132, 0.000000000000000000, 0.000000000000000000 ) ) ;
#12863 = AXIS2_PLACEMENT_3D ( 'NONE', #1030, #2934, #27152 ) ;
#12864 = AXIS2_PLACEMENT_3D ( 'NONE', #4667, #1988, #11959 ) ;
#12865 = DIRECTION ( 'NONE',  ( 0.000000000000000000, 0.000000000000000000, 1.000000000000000000 ) ) ;
#12866 = EDGE_CURVE ( 'NONE', #29758, #8534, #9505, .T. ) ;
#12868 = FACE_OUTER_BOUND ( 'NONE', #23718, .T. ) ;
#12867 = DIRECTION ( 'NONE',  ( 9.754918421198724481E-16, 0.9601771338024399638, 0.2793919678926571892 ) ) ;
#12869 = VECTOR ( 'NONE', #9139, 1000.000000000000000 ) ;
#12870 = CARTESIAN_POINT ( 'NONE',  ( 58.66864673770970029, -0.4999999999993857136, 1.807442289571351335 ) ) ;
#12871 = PLANE ( 'NONE',  #10927 ) ;
#12872 = CARTESIAN_POINT ( 'NONE',  ( 58.73379417893110599, 1.267842757871880277, -1.381558089342544537 ) ) ;
#12873 = CARTESIAN_POINT ( 'NONE',  ( 54.06651298255822979, 5.714592026537127722, 2.049999999999811529 ) ) ;
#12874 = TOROIDAL_SURFACE ( 'NONE', #10874, 4.800000000000000711, 0.05000000000000000278 ) ;
#12875 = ORIENTED_EDGE ( 'NONE', *, *, #9015, .F. ) ;
#12876 = CARTESIAN_POINT ( 'NONE',  ( 52.10742184747378758, 0.5153941949047937676, 1.803012124260139570 ) ) ;
#12877 = ORIENTED_EDGE ( 'NONE', *, *, #13333, .F. ) ;
#12878 = EDGE_LOOP ( 'NONE', ( #20797, #29399, #26869, #26871 ) ) ;
#12879 = CARTESIAN_POINT ( 'NONE',  ( -62.06710100716626499, -2.504070139480777613, -0.3244344873171103316 ) ) ;
#12880 = CARTESIAN_POINT ( 'NONE',  ( -58.98542740578360366, 0.7887156198831661857, -3.845940847736173840 ) ) ;
#12882 = CARTESIAN_POINT ( 'NONE',  ( 58.65000000000004121, -1.877732920580617693, -0.6121634413826788634 ) ) ;
#12881 = CARTESIAN_POINT ( 'NONE',  ( -58.43749999999997158, -3.925981830489445379, -2.215933297149796442E-13 ) ) ;
#12883 = VERTEX_POINT ( 'NONE', #29107 ) ;
#12884 = ORIENTED_EDGE ( 'NONE', *, *, #1726, .T. ) ;
#12885 = CIRCLE ( 'NONE', #9880, 0.1000000000000002554 ) ;
#12886 = CARTESIAN_POINT ( 'NONE',  ( 50.80000000000001137, -4.319730106884872356, -1.256953381662414326 ) ) ;
#12887 = ORIENTED_EDGE ( 'NONE', *, *, #2514, .F. ) ;
#12888 = CARTESIAN_POINT ( 'NONE',  ( 51.76667388380258927, 3.850183871955880299, -1.478071712164887197 ) ) ;
#12889 = EDGE_CURVE ( 'NONE', #27700, #489, #4428, .T. ) ;
#12890 = ORIENTED_EDGE ( 'NONE', *, *, #17953, .F. ) ;
#12891 = CARTESIAN_POINT ( 'NONE',  ( 31.50816695936942224, 7.454773701385264850, -1.950000000000142286 ) ) ;
#12892 = EDGE_CURVE ( 'NONE', #15120, #15422, #18092, .T. ) ;
#12893 = AXIS2_PLACEMENT_3D ( 'NONE', #24135, #18764, #6871 ) ;
#12894 = CARTESIAN_POINT ( 'NONE',  ( -54.39999999999999147, 1.399999999999998135, 3.363870538531246623 ) ) ;
#12895 = EDGE_CURVE ( 'NONE', #30896, #28721, #27108, .T. ) ;
#12896 = CARTESIAN_POINT ( 'NONE',  ( -58.99999999999995737, 2.523434546734630224E-14, -3.400000000000209521 ) ) ;
#12897 = CARTESIAN_POINT ( 'NONE',  ( 15.03925126672133494, -5.377732432866644707, -0.5657657256215723462 ) ) ;
#12898 = AXIS2_PLACEMENT_3D ( 'NONE', #6644, #1895, #14232 ) ;
#12899 = CARTESIAN_POINT ( 'NONE',  ( -60.95655989232410121, 1.962990915244748891, -3.400000000000207301 ) ) ;
#12900 = B_SPLINE_CURVE_WITH_KNOTS ( 'NONE', 3,
 ( #15099, #25056, #22248, #22866 ),
 .UNSPECIFIED., .F., .F.,
 ( 4, 4 ),
 ( 0.0001886355468578361809, 0.0003849279710740182033 ),
 .UNSPECIFIED. ) ;
#12901 = DIRECTION ( 'NONE',  ( -1.000000000000000000, 1.219044193948983948E-29, -3.491481338843133355E-15 ) ) ;
#12902 = CARTESIAN_POINT ( 'NONE',  ( 47.44380078827037295, -3.851485842263134174, -1.408112718338090819 ) ) ;
#12903 = CARTESIAN_POINT ( 'NONE',  ( 51.36308620441098327, 1.097739233406258563, 1.198394850649636689 ) ) ;
#12904 = DIRECTION ( 'NONE',  ( -1.000000000000000000, -2.586136946169074517E-16, 0.000000000000000000 ) ) ;
#12905 = CARTESIAN_POINT ( 'NONE',  ( -56.93749999999996447, 0.7533615035078061739, -3.673546848079177973 ) ) ;
#12906 = VECTOR ( 'NONE', #428, 1000.000000000000000 ) ;
#12907 = CARTESIAN_POINT ( 'NONE',  ( -58.47085481156723574, 1.184343223768590692, 3.558065644182727194 ) ) ;
#12908 = CIRCLE ( 'NONE', #6845, 0.04999999999999987094 ) ;
#12909 = FACE_OUTER_BOUND ( 'NONE', #27353, .T. ) ;
#12910 = CARTESIAN_POINT ( 'NONE',  ( 51.59739104186229497, -1.010292945602101256, 1.272765950230260623 ) ) ;
#12911 = VERTEX_POINT ( 'NONE', #8043 ) ;
#12912 = B_SPLINE_CURVE_WITH_KNOTS ( 'NONE', 3,
 ( #14782, #21794, #79, #29489, #17028, #19562, #534, #24442, #9740, #384, #10048, #2610, #10191, #17322, #19718, #22391, #29352, #26966, #12255 ),
 .UNSPECIFIED., .F., .F.,
 ( 4, 3, 3, 3, 3, 3, 4 ),
 ( -1.463115107851837610E-06, 0.000000000000000000, 2.244303852771090691E-05, 4.060544239443336439E-05, 5.609829020924229540E-05, 7.063629490958459251E-05, 8.524507318609981404E-05 ),
 .UNSPECIFIED. ) ;
#12914 = EDGE_CURVE ( 'NONE', #9901, #8886, #12307, .T. ) ;
#12913 = AXIS2_PLACEMENT_3D ( 'NONE', #3585, #1195, #8489 ) ;
#12915 = CYLINDRICAL_SURFACE ( 'NONE', #20583, 0.09999999999999982514 ) ;
#12916 = CARTESIAN_POINT ( 'NONE',  ( 54.28867365409855950, 5.640057820322907922, 0.9749999999998116840 ) ) ;
#12917 = AXIS2_PLACEMENT_3D ( 'NONE', #7804, #682, #15098 ) ;
#12918 = ORIENTED_EDGE ( 'NONE', *, *, #909, .T. ) ;
#12919 = CARTESIAN_POINT ( 'NONE',  ( 59.35000000000002984, 1.401298464324817071E-42, -6.216582523810200043E-13 ) ) ;
#12920 = EDGE_LOOP ( 'NONE', ( #26608, #8031, #28701, #6888, #12590 ) ) ;
#12921 = AXIS2_PLACEMENT_3D ( 'NONE', #18137, #15592, #1480 ) ;
#12922 = EDGE_CURVE ( 'NONE', #18983, #23830, #20354, .T. ) ;
#12923 = CARTESIAN_POINT ( 'NONE',  ( 61.25000000000000000, 2.008165151418888072, -0.5380862305899540843 ) ) ;
#12924 = CARTESIAN_POINT ( 'NONE',  ( 52.08333333333334281, 4.368973594129894167, -2.050000000000181455 ) ) ;
#12926 = CARTESIAN_POINT ( 'NONE',  ( 58.75000000000000000, 1.996089927834530986, 0.1250000000010043355 ) ) ;
#12925 = CARTESIAN_POINT ( 'NONE',  ( 48.37818655883430807, -1.309616516426920230, -3.885368734293527471 ) ) ;
#12927 = EDGE_LOOP ( 'NONE', ( #9872, #6003, #31152, #21463 ) ) ;
#12928 = CARTESIAN_POINT ( 'NONE',  ( 60.82068433953604369, -0.6500001811771835003, -1.489337021788164739 ) ) ;
#12929 = CARTESIAN_POINT ( 'NONE',  ( -55.78335481156724285, 0.7533615035078067290, -3.673546848079180194 ) ) ;
#12930 = ORIENTED_EDGE ( 'NONE', *, *, #8109, .F. ) ;
#12932 = DIRECTION ( 'NONE',  ( 1.000000000000000000, 3.053848253006669023E-16, -2.042510438544995415E-16 ) ) ;
#12931 = CARTESIAN_POINT ( 'NONE',  ( 48.00000000000001421, -4.003661535119149129, -1.169131321892086017 ) ) ;
#12933 = CYLINDRICAL_SURFACE ( 'NONE', #29673, 4.299999999999998046 ) ;
#12934 = ORIENTED_EDGE ( 'NONE', *, *, #17523, .F. ) ;
#12935 = FACE_OUTER_BOUND ( 'NONE', #23936, .T. ) ;
#12936 = DIRECTION ( 'NONE',  ( 0.000000000000000000, 0.9996898646859343485, 0.02490330187381123439 ) ) ;
#12937 = ADVANCED_FACE ( 'NONE', ( #7720 ), #25665, .T. ) ;
#12938 = AXIS2_PLACEMENT_3D ( 'NONE', #905, #15629, #12605 ) ;
#12939 = DIRECTION ( 'NONE',  ( 0.000000000000000000, 0.000000000000000000, -1.000000000000000000 ) ) ;
#12940 = AXIS2_PLACEMENT_3D ( 'NONE', #2375, #14565, #2539 ) ;
#12941 = CARTESIAN_POINT ( 'NONE',  ( -62.04999999999998295, -2.671081280896084653, -0.3941126626315437642 ) ) ;
#12942 = AXIS2_PLACEMENT_3D ( 'NONE', #30289, #3689, #16046 ) ;
#12943 = CARTESIAN_POINT ( 'NONE',  ( -59.69999999999996732, 1.144555898245933179, -3.233327234211546219 ) ) ;
#12944 = CARTESIAN_POINT ( 'NONE',  ( 51.98914612709258876, -0.7788013043298228633, 1.433123603079414776 ) ) ;
#12945 = CIRCLE ( 'NONE', #6372, 1.975000000000001865 ) ;
#12946 = AXIS2_PLACEMENT_3D ( 'NONE', #25852, #15734, #21132 ) ;
#12947 = VERTEX_POINT ( 'NONE', #9955 ) ;
#12948 = VECTOR ( 'NONE', #15406, 1000.000000000000000 ) ;
#12949 = AXIS2_PLACEMENT_3D ( 'NONE', #5256, #12838, #3049 ) ;
#12950 = CARTESIAN_POINT ( 'NONE',  ( 15.17214319754860696, 2.686240675664339328, 4.475885398016751004 ) ) ;
#12951 = CARTESIAN_POINT ( 'NONE',  ( -55.48542740578360366, -3.725040285533364859, 1.239922660687672540 ) ) ;
#12952 = CARTESIAN_POINT ( 'NONE',  ( -58.33155989232412963, -1.962990915244733348, 3.399999999999783640 ) ) ;
#12953 = AXIS2_PLACEMENT_3D ( 'NONE', #26892, #4896, #7438 ) ;
#12954 = ADVANCED_FACE ( 'NONE', ( #7873 ), #27202, .F. ) ;
#12955 = VECTOR ( 'NONE', #1163, 999.9999999999998863 ) ;
#12956 = CARTESIAN_POINT ( 'NONE',  ( -57.50952994616203995, -3.117691453623959941, -1.800000000000221645 ) ) ;
#12957 = CARTESIAN_POINT ( 'NONE',  ( -36.11122220296831387, 0.3980941177579020440, 5.199999998461541928 ) ) ;
#12958 = CARTESIAN_POINT ( 'NONE',  ( -54.49999999999999289, 1.599999999999998090, 3.363870538531247067 ) ) ;
#12959 = EDGE_CURVE ( 'NONE', #21014, #11082, #8476, .T. ) ;
#12960 = ORIENTED_EDGE ( 'NONE', *, *, #2278, .F. ) ;
#12961 = LINE ( 'NONE', #29906, #19902 ) ;
#12962 = CIRCLE ( 'NONE', #9471, 2.263970382088065225 ) ;
#12963 = ORIENTED_EDGE ( 'NONE', *, *, #9226, .T. ) ;
#12964 = ADVANCED_FACE ( 'NONE', ( #19630 ), #22310, .F. ) ;
#12965 = CARTESIAN_POINT ( 'NONE',  ( -59.09999999999997300, 2.465712773623992327, -0.9709585562669131864 ) ) ;
#12967 = FACE_OUTER_BOUND ( 'NONE', #13772, .T. ) ;
#12966 = CARTESIAN_POINT ( 'NONE',  ( 15.87128154250933321, -3.738196885377849998, -3.908481927057574801 ) ) ;
#12968 = CIRCLE ( 'NONE', #25106, 0.1500000000000001887 ) ;
#12969 = VERTEX_POINT ( 'NONE', #21855 ) ;
#12970 = ORIENTED_EDGE ( 'NONE', *, *, #14756, .F. ) ;
#12971 = DIRECTION ( 'NONE',  ( -1.000000000000000000, -3.053848253006669023E-16, 2.042510438544995169E-16 ) ) ;
#12972 = CARTESIAN_POINT ( 'NONE',  ( -63.84999999999997300, 6.335931579819947332E-16, 2.555166080847169934E-15 ) ) ;
#12973 = ORIENTED_EDGE ( 'NONE', *, *, #8251, .F. ) ;
#12974 = AXIS2_PLACEMENT_3D ( 'NONE', #499, #348, #14750 ) ;
#12976 = CARTESIAN_POINT ( 'NONE',  ( -55.44184846062112371, 0.2309624077929101071, 3.875409454552791733 ) ) ;
#12975 = CARTESIAN_POINT ( 'NONE',  ( -57.38452994616203284, 2.093608279459370457E-14, -3.600000000000203926 ) ) ;
#12977 = CIRCLE ( 'NONE', #22112, 0.1000000000000000472 ) ;
#12978 = CARTESIAN_POINT ( 'NONE',  ( -56.98542740578360366, -3.725040285533364859, 1.239922660687675204 ) ) ;
#12979 = CARTESIAN_POINT ( 'NONE',  ( -54.49999999999996447, -1.514093959731525496, -3.183260039818593512 ) ) ;
#12980 = DIRECTION ( 'NONE',  ( 0.000000000000000000, 0.000000000000000000, 1.000000000000000000 ) ) ;
#12981 = EDGE_CURVE ( 'NONE', #3532, #2009, #27847, .T. ) ;
#12982 = CARTESIAN_POINT ( 'NONE',  ( -59.29999999999997584, -2.208048483361063852, 2.585444235547710967 ) ) ;
#12983 = SHAPE_REPRESENTATION_RELATIONSHIP ( 'NONE' , 'NONE' ,  #30888, #13430 ) ;
#12984 = VECTOR ( 'NONE', #27237, 1000.000000000000000 ) ;
#12985 = ORIENTED_EDGE ( 'NONE', *, *, #19931, .T. ) ;
#12986 = VECTOR ( 'NONE', #17702, 1000.000000000000000 ) ;
#12987 = DIRECTION ( 'NONE',  ( -1.000000000000000000, 1.219044193948983948E-29, -3.491481338843133355E-15 ) ) ;
#12988 = AXIS2_PLACEMENT_3D ( 'NONE', #16652, #13758, #4595 ) ;
#12989 = CARTESIAN_POINT ( 'NONE',  ( 53.55869261961984051, 7.702978059423601032, -1.861455469535500340 ) ) ;
#12990 = DIRECTION ( 'NONE',  ( 2.614375865348240525E-16, -0.2008964009354147762, 0.9796124928211140670 ) ) ;
#12991 = PRODUCT_RELATED_PRODUCT_CATEGORY ( 'part', '', ( #7773 ) ) ;
#12992 = CARTESIAN_POINT ( 'NONE',  ( 15.95705409078464498, 0.6016956010317275894, 5.375730734456589666 ) ) ;
#12993 = FACE_OUTER_BOUND ( 'NONE', #11295, .T. ) ;
#12994 = AXIS2_PLACEMENT_3D ( 'NONE', #21992, #5189, #29105 ) ;
#12995 = TOROIDAL_SURFACE ( 'NONE', #4418, 2.649999999999999911, 0.05000000000000000278 ) ;
#12997 = CARTESIAN_POINT ( 'NONE',  ( 68.00000000000005684, -1.025519176787267142E-28, 4.049999999999288391 ) ) ;
#12996 = CARTESIAN_POINT ( 'NONE',  ( -56.93749999999996447, -3.399999999999991473, -2.119568960425587465E-13 ) ) ;
#12998 = AXIS2_PLACEMENT_3D ( 'NONE', #12079, #16510, #11438 ) ;
#12999 = CARTESIAN_POINT ( 'NONE',  ( -71.44999999999998863, 0.3062499654112550429, -1.493338310920502066 ) ) ;
#13000 = CARTESIAN_POINT ( 'NONE',  ( 52.41492537898349013, 3.996662292477194178, -2.045735003821204767 ) ) ;
#13002 = CARTESIAN_POINT ( 'NONE',  ( -59.66355212511316353, 2.047887940248842575, 1.716336187188254314 ) ) ;
#13001 = DIRECTION ( 'NONE',  ( 0.000000000000000000, -0.3529411764705844834, -0.9356455129756994227 ) ) ;
#13003 = EDGE_CURVE ( 'NONE', #320, #363, #142, .T. ) ;
#13004 = EDGE_LOOP ( 'NONE', ( #18694, #15793, #14879, #21198, #17746, #10717, #20288, #28905 ) ) ;
#13005 = FACE_OUTER_BOUND ( 'NONE', #22702, .T. ) ;
#13006 = CARTESIAN_POINT ( 'NONE',  ( 58.45000000000001705, 0.7500000000000000000, 2.421260002560649660 ) ) ;
#13007 = VECTOR ( 'NONE', #13856, 1000.000000000000000 ) ;
#13009 = CARTESIAN_POINT ( 'NONE',  ( 58.65000000000002700, -0.8495817349395312634, -1.671477153794241666 ) ) ;
#13008 = CARTESIAN_POINT ( 'NONE',  ( 15.76623786017565187, 3.265074799938528116, -4.311675893544650862 ) ) ;
#13010 = DIRECTION ( 'NONE',  ( 0.000000000000000000, 0.000000000000000000, 1.000000000000000000 ) ) ;
#13011 = ORIENTED_EDGE ( 'NONE', *, *, #21720, .T. ) ;
#13012 = CARTESIAN_POINT ( 'NONE',  ( 51.65313719492862532, 3.829415913202793398, 2.049999999999819522 ) ) ;
#13013 = CARTESIAN_POINT ( 'NONE',  ( 47.01022879663531029, -4.154252208774217969, 1.054526470899727286 ) ) ;
#13014 = AXIS2_PLACEMENT_3D ( 'NONE', #9649, #26734, #22143 ) ;
#13015 = ORIENTED_EDGE ( 'NONE', *, *, #16984, .F. ) ;
#13016 = CARTESIAN_POINT ( 'NONE',  ( 51.86020163181184017, 8.198949176608044453, 2.049999999999819522 ) ) ;
#13017 = ORIENTED_EDGE ( 'NONE', *, *, #15779, .T. ) ;
#13018 = CARTESIAN_POINT ( 'NONE',  ( -54.39999999999997726, 3.624999999999963585, -1.915392816594897935E-13 ) ) ;
#13019 = CARTESIAN_POINT ( 'NONE',  ( 69.25000000000001421, 4.557543281186736018E-17, -7.253552481446610839E-13 ) ) ;
#13020 = ORIENTED_EDGE ( 'NONE', *, *, #529, .F. ) ;
#13021 = FILL_AREA_STYLE_COLOUR ( '', #28272 ) ;
#13022 = CARTESIAN_POINT ( 'NONE',  ( 51.43901883478556414, 0.9711235217376542606, -1.449592546241924573 ) ) ;
#13023 = VECTOR ( 'NONE', #28769, 1000.000000000000000 ) ;
#13024 = EDGE_CURVE ( 'NONE', #1709, #8004, #26171, .T. ) ;
#13025 = CARTESIAN_POINT ( 'NONE',  ( -54.45655989232412963, -3.925981830489445379, -2.076939516179772989E-13 ) ) ;
#13026 = EDGE_LOOP ( 'NONE', ( #1233, #18454, #23864, #26846 ) ) ;
#13027 = CARTESIAN_POINT ( 'NONE',  ( 56.95000000000001705, 0.6937162836135747357, -1.768873629894432975 ) ) ;
#13028 = VECTOR ( 'NONE', #25893, 1000.000000000000114 ) ;
#13029 = CARTESIAN_POINT ( 'NONE',  ( 51.64333574538934357, 0.8318165372350851960, -1.569663068107118642 ) ) ;
#13030 = CARTESIAN_POINT ( 'NONE',  ( 22.00282357718615245, 7.757228888719249760, 1.949999999999923128 ) ) ;
#13031 = CARTESIAN_POINT ( 'NONE',  ( -58.62499999999998579, -3.920666489018310435E-15, 3.399999999999791189 ) ) ;
#13032 = CARTESIAN_POINT ( 'NONE',  ( 60.99000702708163857, 0.5469907030331696562, 1.538545889480190665 ) ) ;
#13033 = DIRECTION ( 'NONE',  ( 0.000000000000000000, 0.000000000000000000, 1.000000000000000000 ) ) ;
#13034 = DIRECTION ( 'NONE',  ( -1.000000000000000000, 1.219044193948983948E-29, -3.491481338843133355E-15 ) ) ;
#13035 = CARTESIAN_POINT ( 'NONE',  ( 56.99999999998442490, -0.7044205509462206916, 2.449516039469794570 ) ) ;
#13036 = CIRCLE ( 'NONE', #30743, 2.136029617911934686 ) ;
#13037 =( BOUNDED_CURVE ( )  B_SPLINE_CURVE ( 3, ( #11405, #13451, #6813, #25495 ),
 .UNSPECIFIED., .F., .T. ) 
 B_SPLINE_CURVE_WITH_KNOTS ( ( 4, 4 ),
 ( 4.041453792691653391, 4.300872134317200945 ),
 .UNSPECIFIED. ) 
 CURVE ( )  GEOMETRIC_REPRESENTATION_ITEM ( )  RATIONAL_B_SPLINE_CURVE ( ( 1.000000000000000000, 0.9943997021150918769, 0.9943997021150918769, 1.000000000000000000 ) ) 
 REPRESENTATION_ITEM ( '' )  );
#13038 = VECTOR ( 'NONE', #19910, 1000.000000000000000 ) ;
#13040 = PLANE ( 'NONE',  #8327 ) ;
#13039 = DIRECTION ( 'NONE',  ( 0.000000000000000000, 0.000000000000000000, 1.000000000000000000 ) ) ;
#13041 = CARTESIAN_POINT ( 'NONE',  ( -54.44999999999997442, 0.000000000000000000, 2.168404344971008868E-14 ) ) ;
#13042 = CARTESIAN_POINT ( 'NONE',  ( -59.67318048135356179, 2.383480368854711262, -1.229362881338640801 ) ) ;
#13043 = CARTESIAN_POINT ( 'NONE',  ( 58.45000000000001705, -0.8000000000000000444, 2.421260002560649660 ) ) ;
#13044 = EDGE_CURVE ( 'NONE', #23827, #14659, #8655, .T. ) ;
#13045 = CARTESIAN_POINT ( 'NONE',  ( 58.75000000000000711, 1.320082690054482866, -1.469015551796560404 ) ) ;
#13046 = CARTESIAN_POINT ( 'NONE',  ( 54.05502230659780594, 7.179870641707980283, -2.050000000000187672 ) ) ;
#13047 = ORIENTED_EDGE ( 'NONE', *, *, #22720, .T. ) ;
#13048 = CARTESIAN_POINT ( 'NONE',  ( -54.49646078629579193, 1.531523113441620731, 3.320331042554034440 ) ) ;
#13049 = ORIENTED_EDGE ( 'NONE', *, *, #4164, .T. ) ;
#13050 = ORIENTED_EDGE ( 'NONE', *, *, #30024, .F. ) ;
#13051 = DIRECTION ( 'NONE',  ( 1.000000000000000000, -1.219044193948983948E-29, 3.491481338843133355E-15 ) ) ;
#13052 = CARTESIAN_POINT ( 'NONE',  ( -58.73542740578359656, 2.936324665650206889, 2.606018187048499080 ) ) ;
#13054 = CARTESIAN_POINT ( 'NONE',  ( 47.86735275623932750, -4.319730106884873244, 1.256953381662070379 ) ) ;
#13053 = CARTESIAN_POINT ( 'NONE',  ( -56.74999999999995737, 2.023778652682507474E-14, -3.400000000000201972 ) ) ;
#13055 = EDGE_LOOP ( 'NONE', ( #28941, #28328, #30780, #8573 ) ) ;
#13056 = ORIENTED_EDGE ( 'NONE', *, *, #3790, .T. ) ;
#13057 = ORIENTED_EDGE ( 'NONE', *, *, #10812, .T. ) ;
#13058 = DIRECTION ( 'NONE',  ( 0.000000000000000000, 0.000000000000000000, 1.000000000000000000 ) ) ;
#13059 = EDGE_CURVE ( 'NONE', #27956, #30450, #12509, .T. ) ;
#13060 = ORIENTED_EDGE ( 'NONE', *, *, #30510, .F. ) ;
#13061 = CARTESIAN_POINT ( 'NONE',  ( 22.40865038670843390, 7.071719536792667071, -2.050000000000077982 ) ) ;
#13062 = ORIENTED_EDGE ( 'NONE', *, *, #10014, .F. ) ;
#13063 = DIRECTION ( 'NONE',  ( 1.054009200593503061E-14, 0.000000000000000000, 1.000000000000000000 ) ) ;
#13064 = CARTESIAN_POINT ( 'NONE',  ( -54.44999999999997442, 5.694607616035192869E-16, -4.650000000000000355 ) ) ;
#13065 = CARTESIAN_POINT ( 'NONE',  ( 15.03925126672127988, -4.804073783693435296, -2.042134687550375638 ) ) ;
#13066 = CARTESIAN_POINT ( 'NONE',  ( -60.01905989232411542, 2.944486372867092250, 1.699999999999798339 ) ) ;
#13067 = EDGE_CURVE ( 'NONE', #2901, #1734, #28178, .T. ) ;
#13068 = DIRECTION ( 'NONE',  ( 0.000000000000000000, 0.000000000000000000, -1.000000000000000000 ) ) ;
#13069 = CARTESIAN_POINT ( 'NONE',  ( 47.73664259148971212, -4.023874009802445251, -1.198297772469074207 ) ) ;
#13070 = CARTESIAN_POINT ( 'NONE',  ( 51.80000000000000426, 7.038595743567426471E-14, -4.600000000000216360 ) ) ;
#13071 = FACE_OUTER_BOUND ( 'NONE', #25681, .T. ) ;
#13073 = FACE_OUTER_BOUND ( 'NONE', #6485, .T. ) ;
#13072 = CARTESIAN_POINT ( 'NONE',  ( -60.59540624230464800, -2.457874471988325205, 0.9407545623323243511 ) ) ;
#13074 = CARTESIAN_POINT ( 'NONE',  ( -58.74986116251333357, 1.737685414808516793, -3.471684241605569099 ) ) ;
#13075 = DIRECTION ( 'NONE',  ( 0.000000000000000000, 0.000000000000000000, -1.000000000000000000 ) ) ;
#13076 = CIRCLE ( 'NONE', #14601, 2.649999999999999911 ) ;
#13077 = ADVANCED_FACE ( 'NONE', ( #17713 ), #3424, .T. ) ;
#13078 = CARTESIAN_POINT ( 'NONE',  ( -45.15971931043468146, 0.000000000000000000, 0.000000000000000000 ) ) ;
#13079 = ADVANCED_FACE ( 'NONE', ( #27971 ), #3603, .T. ) ;
#13080 = ORIENTED_EDGE ( 'NONE', *, *, #7123, .F. ) ;
#13081 = ADVANCED_FACE ( 'NONE', ( #25292 ), #20721, .T. ) ;
#13082 = DIRECTION ( 'NONE',  ( 0.000000000000000000, 0.000000000000000000, -1.000000000000000000 ) ) ;
#13083 = CARTESIAN_POINT ( 'NONE',  ( 54.25934656145521018, 5.649896967619270960, 2.026383240762962057 ) ) ;
#13084 = EDGE_LOOP ( 'NONE', ( #14607, #30527, #9006, #9546 ) ) ;
#13085 = DIRECTION ( 'NONE',  ( 1.000000000000000000, 1.047444401652940007E-14, 0.000000000000000000 ) ) ;
#13086 = EDGE_LOOP ( 'NONE', ( #11738, #8459, #23346, #22527 ) ) ;
#13087 = CARTESIAN_POINT ( 'NONE',  ( 57.00000000000001421, 0.000000000000000000, 0.000000000000000000 ) ) ;
#13088 = CARTESIAN_POINT ( 'NONE',  ( -54.28335481156724285, 0.8699069336946697595, -4.241846523238430144 ) ) ;
#13089 = DIRECTION ( 'NONE',  ( 0.9993908270190956511, -0.03489949670250103858, -3.469446951953534514E-15 ) ) ;
#13090 = ORIENTED_EDGE ( 'NONE', *, *, #9527, .F. ) ;
#13091 = CARTESIAN_POINT ( 'NONE',  ( 61.25000000000000000, 1.791164585742741400, 0.8897917884450912140 ) ) ;
#13092 = FACE_OUTER_BOUND ( 'NONE', #16411, .T. ) ;
#13093 = EDGE_CURVE ( 'NONE', #6127, #7673, #13240, .T. ) ;
#13095 = CARTESIAN_POINT ( 'NONE',  ( 57.00000000000001421, 0.000000000000000000, 0.000000000000000000 ) ) ;
#13094 = DIRECTION ( 'NONE',  ( 0.000000000000000000, -1.000000000000000000, -0.000000000000000000 ) ) ;
#13096 = EDGE_LOOP ( 'NONE', ( #14653, #7467, #12026, #19042 ) ) ;
#13097 = DIRECTION ( 'NONE',  ( 3.384826294588897856E-15, 0.000000000000000000, 1.000000000000000000 ) ) ;
#13098 = CARTESIAN_POINT ( 'NONE',  ( -36.68133364217572989, 4.872718122832791821, -2.345308583460306462 ) ) ;
#13099 = CARTESIAN_POINT ( 'NONE',  ( 58.65000045311386145, 1.663878723408452442, -0.8645309767532183276 ) ) ;
#13100 = PRODUCT_DEFINITION_FORMATION_WITH_SPECIFIED_SOURCE ( 'ANY', '', #11370, .NOT_KNOWN. ) ;
#13101 = AXIS2_PLACEMENT_3D ( 'NONE', #7641, #9861, #2887 ) ;
#13102 = CARTESIAN_POINT ( 'NONE',  ( -35.85663232820584057, -4.018128179617557194, 3.618665901676652918 ) ) ;
#13103 = DIRECTION ( 'NONE',  ( 0.000000000000000000, 0.000000000000000000, -1.000000000000000000 ) ) ;
#13104 = FACE_OUTER_BOUND ( 'NONE', #16614, .T. ) ;
#13105 = ADVANCED_FACE ( 'NONE', ( #5820 ), #1532, .F. ) ;
#13106 = ORIENTED_EDGE ( 'NONE', *, *, #8280, .T. ) ;
#13107 = ADVANCED_FACE ( 'NONE', ( #1380 ), #20867, .T. ) ;
#13108 = CARTESIAN_POINT ( 'NONE',  ( 15.39414421509791353, 2.821511581828376247, 4.377605326016295706 ) ) ;
#13109 = CARTESIAN_POINT ( 'NONE',  ( -60.63087243001902493, -2.512277203407240034, 0.9787440703680012621 ) ) ;
#13110 = AXIS2_PLACEMENT_3D ( 'NONE', #11071, #3163, #22486 ) ;
#13111 = CARTESIAN_POINT ( 'NONE',  ( -58.39405989232412963, -2.016369211404101147E-14, 3.399999999999791633 ) ) ;
#13112 = EDGE_CURVE ( 'NONE', #21603, #18295, #30715, .T. ) ;
#13113 = ADVANCED_FACE ( 'NONE', ( #18018 ), #10578, .T. ) ;
#13114 = CARTESIAN_POINT ( 'NONE',  ( -57.94702994616203995, 4.156921938165313968, -1.791987581444107632E-13 ) ) ;
#13115 = CARTESIAN_POINT ( 'NONE',  ( 58.72200624034179839, -1.875003484780597418, -0.02193204975889442854 ) ) ;
#13116 = CARTESIAN_POINT ( 'NONE',  ( 27.80355388919737436, 5.537003769396955377, 2.049999999999903011 ) ) ;
#13117 = ORIENTED_EDGE ( 'NONE', *, *, #7690, .T. ) ;
#13118 = CIRCLE ( 'NONE', #2012, 0.4576450603546999840 ) ;
#13119 = AXIS2_PLACEMENT_3D ( 'NONE', #20303, #17905, #12990 ) ;
#13120 = CARTESIAN_POINT ( 'NONE',  ( -57.72499999999997300, 0.9643027244899933237, -4.702139965541347166 ) ) ;
#13121 = EDGE_LOOP ( 'NONE', ( #13201, #8159, #23204, #13412 ) ) ;
#13122 = CARTESIAN_POINT ( 'NONE',  ( -59.19174289917960863, 2.538702292234776170, -0.9450962354860914516 ) ) ;
#13123 = CARTESIAN_POINT ( 'NONE',  ( 52.20711756518984004, -0.4999999999994533817, -1.718465885608440269 ) ) ;
#13124 = VERTEX_POINT ( 'NONE', #17864 ) ;
#13125 = ORIENTED_EDGE ( 'NONE', *, *, #19781, .F. ) ;
#13126 = AXIS2_PLACEMENT_3D ( 'NONE', #6608, #25295, #6456 ) ;
#13127 = DIRECTION ( 'NONE',  ( -1.000000000000000000, -1.047444401652940007E-14, -0.000000000000000000 ) ) ;
#13128 = VERTEX_POINT ( 'NONE', #24962 ) ;
#13130 = CARTESIAN_POINT ( 'NONE',  ( 58.75000000000000711, 1.066009655020737856, 1.652371589364121984 ) ) ;
#13129 = CARTESIAN_POINT ( 'NONE',  ( -56.07202994616204705, -4.156921938165296204, -2.141547992439359634E-13 ) ) ;
#13131 = CARTESIAN_POINT ( 'NONE',  ( -56.54792740578360366, 3.330682475591790315, 0.6830477631804106053 ) ) ;
#13132 = DIRECTION ( 'NONE',  ( -1.000000000000000000, -1.786976680021908743E-16, 2.459562394685749209E-16 ) ) ;
#13133 = DIRECTION ( 'NONE',  ( 1.000000000000000000, 0.000000000000000000, 0.000000000000000000 ) ) ;
#13134 = CARTESIAN_POINT ( 'NONE',  ( -61.39879105983193597, -2.624675223805974511, -0.6332464253769281015 ) ) ;
#13135 = FILL_AREA_STYLE ('',( #25332 ) ) ;
#13136 = ADVANCED_FACE ( 'NONE', ( #3288 ), #8964, .T. ) ;
#13137 = ORIENTED_EDGE ( 'NONE', *, *, #12892, .T. ) ;
#13138 = EDGE_CURVE ( 'NONE', #2190, #7150, #25440, .T. ) ;
#13139 = CARTESIAN_POINT ( 'NONE',  ( -60.50952994616203284, -3.117691453623963938, -1.800000000000225864 ) ) ;
#13140 = ADVANCED_FACE ( 'NONE', ( #29886 ), #8196, .T. ) ;
#13141 = CARTESIAN_POINT ( 'NONE',  ( 53.87654288987800300, 4.973000991543902849, -2.050000000000187672 ) ) ;
#13142 = CARTESIAN_POINT ( 'NONE',  ( -56.67306624327023457, -3.399999999999988365, -0.9110272542660329265 ) ) ;
#13143 = AXIS2_PLACEMENT_3D ( 'NONE', #2124, #19089, #7052 ) ;
#13144 = CARTESIAN_POINT ( 'NONE',  ( 15.03925126672125856, -0.7747498368337712993, 5.363501452440941009 ) ) ;
#13145 = VECTOR ( 'NONE', #25254, 1000.000000000000000 ) ;
#13146 = DIRECTION ( 'NONE',  ( 0.000000000000000000, 0.000000000000000000, -1.000000000000000000 ) ) ;
#13148 = CARTESIAN_POINT ( 'NONE',  ( 58.74160516400037579, -1.833004249032245347, -0.3946733352255804017 ) ) ;
#13147 = DIRECTION ( 'NONE',  ( -3.002035892788116966E-16, 0.9996898646859343485, 0.02490330187381124133 ) ) ;
#13149 = CARTESIAN_POINT ( 'NONE',  ( 50.87826055314398133, 8.733544086820096197, -2.050000000000176570 ) ) ;
#13150 = DIRECTION ( 'NONE',  ( 2.586136946169074517E-16, -1.000000000000000000, 0.000000000000000000 ) ) ;
#13152 = DIRECTION ( 'NONE',  ( 0.000000000000000000, -1.000000000000000000, -4.336808689942015369E-15 ) ) ;
#13151 = CARTESIAN_POINT ( 'NONE',  ( 57.00000000000001421, 0.000000000000000000, 1.949999999999999956 ) ) ;
#13153 = ORIENTED_EDGE ( 'NONE', *, *, #8735, .F. ) ;
#13154 = DIRECTION ( 'NONE',  ( 0.000000000000000000, 0.000000000000000000, -1.000000000000000000 ) ) ;
#13155 = CARTESIAN_POINT ( 'NONE',  ( 58.75000000000002132, 6.153735859711025284E-13, 3.111507638930570854E-58 ) ) ;
#13157 = CARTESIAN_POINT ( 'NONE',  ( -57.22499999999997300, 0.8236752438352034078, -4.016411220566566520 ) ) ;
#13156 = CARTESIAN_POINT ( 'NONE',  ( 15.48686146417446530, 2.966783028120432153, -4.272059443775269472 ) ) ;
#13158 = DIRECTION ( 'NONE',  ( 0.000000000000000000, 0.000000000000000000, -1.000000000000000000 ) ) ;
#13159 = ORIENTED_EDGE ( 'NONE', *, *, #18150, .T. ) ;
#13160 = CARTESIAN_POINT ( 'NONE',  ( 54.21707933481623343, 5.861459378068796688, 2.049999999999810640 ) ) ;
#13161 = CARTESIAN_POINT ( 'NONE',  ( -60.60558231549867969, -2.446663424644156315, -1.077479343426181124 ) ) ;
#13162 = ORIENTED_EDGE ( 'NONE', *, *, #14355, .T. ) ;
#13163 = CARTESIAN_POINT ( 'NONE',  ( 69.00000000000001421, 4.557543281186736018E-17, -7.227366371405287181E-13 ) ) ;
#13164 = ORIENTED_EDGE ( 'NONE', *, *, #15765, .T. ) ;
#13165 = LINE ( 'NONE', #2044, #20374 ) ;
#13166 = CYLINDRICAL_SURFACE ( 'NONE', #17513, 3.399999999999999911 ) ;
#13167 = ORIENTED_EDGE ( 'NONE', *, *, #11692, .F. ) ;
#13168 =( NAMED_UNIT ( * ) SI_UNIT ( $, .STERADIAN. ) SOLID_ANGLE_UNIT ( ) );
#13169 = VECTOR ( 'NONE', #22793, 1000.000000000000000 ) ;
#13170 = CARTESIAN_POINT ( 'NONE',  ( -35.85663232820584057, -1.793057972834465108, 4.026191436120613254 ) ) ;
#13171 = CARTESIAN_POINT ( 'NONE',  ( -60.69702994616205416, -2.078460969082657872, 3.599999999999776712 ) ) ;
#13172 = ORIENTED_EDGE ( 'NONE', *, *, #5713, .T. ) ;
#13173 = CARTESIAN_POINT ( 'NONE',  ( 53.81457038914302871, 5.799118248596165870, 1.689328270749656191 ) ) ;
#13174 = EDGE_LOOP ( 'NONE', ( #26454, #7688, #15039, #25317, #17310, #18618, #14730, #12635, #2751, #23675, #4324, #3936, #5850, #7563, #30977, #2513, #2453, #22229, #12057, #9364, #3624, #14362 ) ) ;
#13175 = ORIENTED_EDGE ( 'NONE', *, *, #13315, .F. ) ;
#13176 = EDGE_CURVE ( 'NONE', #12697, #10836, #5450, .T. ) ;
#13177 = CARTESIAN_POINT ( 'NONE',  ( -58.37499999999996447, -2.944486372867076707, -1.700000000000217781 ) ) ;
#13178 =( BOUNDED_CURVE ( )  B_SPLINE_CURVE ( 3, ( #30459, #8620, #3574, #13522 ),
 .UNSPECIFIED., .F., .T. ) 
 B_SPLINE_CURVE_WITH_KNOTS ( ( 4, 4 ),
 ( 1.354022462013807049, 1.453942312199770548 ),
 .UNSPECIFIED. ) 
 CURVE ( )  GEOMETRIC_REPRESENTATION_ITEM ( )  RATIONAL_B_SPLINE_CURVE ( ( 1.000000000000000000, 0.9991681750023542197, 0.9991681750023542197, 1.000000000000000000 ) ) 
 REPRESENTATION_ITEM ( '' )  );
#13179 = CARTESIAN_POINT ( 'NONE',  ( 60.88861521483853778, 0.6775725165985903020, 1.477731239195284596 ) ) ;
#13180 = CARTESIAN_POINT ( 'NONE',  ( -61.34999999999997300, -2.520040662139441778, -0.7900246721901127422 ) ) ;
#13181 = CARTESIAN_POINT ( 'NONE',  ( 56.99976900444080030, -0.7668859551697654320, -1.738368808232523044 ) ) ;
#13182 = DIRECTION ( 'NONE',  ( 0.000000000000000000, 1.000000000000000000, 0.000000000000000000 ) ) ;
#13184 = DIRECTION ( 'NONE',  ( -3.491481338843133355E-15, 0.000000000000000000, -1.000000000000000000 ) ) ;
#13183 = CARTESIAN_POINT ( 'NONE',  ( -56.90835481156724285, -0.7533615035077978472, 3.673546848079179750 ) ) ;
#13185 = CIRCLE ( 'NONE', #55, 0.01000000000000001929 ) ;
#13186 = CARTESIAN_POINT ( 'NONE',  ( 50.49731030164353029, -0.9327905306641465222, -3.995066436131524235 ) ) ;
#13187 = DIRECTION ( 'NONE',  ( 1.000000000000000000, 3.054025858079668409E-16, -2.042474015755241579E-16 ) ) ;
#13188 = CARTESIAN_POINT ( 'NONE',  ( -55.62499999999997158, -3.673546848079173532, -0.7533615035078075062 ) ) ;
#13189 = ADVANCED_FACE ( 'NONE', ( #21496 ), #8798, .T. ) ;
#13190 = CARTESIAN_POINT ( 'NONE',  ( -54.48167032960165557, 1.510995100284905579, -3.307167554963766243 ) ) ;
#13191 = CARTESIAN_POINT ( 'NONE',  ( 52.78843926895370231, 8.494246790034939210, -2.050000000000183231 ) ) ;
#13192 = EDGE_LOOP ( 'NONE', ( #29984, #10547, #27388, #22018, #13666, #9356 ) ) ;
#13193 = CARTESIAN_POINT ( 'NONE',  ( 50.37823977475586190, -1.183413901109533706, 3.885761703493072705 ) ) ;
#13194 = CARTESIAN_POINT ( 'NONE',  ( -36.52757395963740095, -0.8926979523208378176, -5.334280177567952919 ) ) ;
#13195 = VERTEX_POINT ( 'NONE', #18489 ) ;
#13196 = ORIENTED_EDGE ( 'NONE', *, *, #25259, .T. ) ;
#13197 = DIRECTION ( 'NONE',  ( 0.000000000000000000, 0.2008964009354148039, -0.9796124928211140670 ) ) ;
#13198 = CARTESIAN_POINT ( 'NONE',  ( 58.75000000000003553, -1.320082690053552277, -1.469015551796290397 ) ) ;
#13200 = CARTESIAN_POINT ( 'NONE',  ( -61.36301639239449912, -2.595653720285160837, 0.6828058785558981381 ) ) ;
#13199 = CARTESIAN_POINT ( 'NONE',  ( -58.68749999999998579, 1.962990915244722689, 3.399999999999799627 ) ) ;
#13201 = ORIENTED_EDGE ( 'NONE', *, *, #20997, .F. ) ;
#13202 = ORIENTED_EDGE ( 'NONE', *, *, #2200, .F. ) ;
#13203 = CYLINDRICAL_SURFACE ( 'NONE', #2779, 0.2500000000000000000 ) ;
#13204 = AXIS2_PLACEMENT_3D ( 'NONE', #13883, #8825, #1879 ) ;
#13205 = VERTEX_POINT ( 'NONE', #28130 ) ;
#13206 = DIRECTION ( 'NONE',  ( 1.000000000000000000, 1.047444401652940007E-14, 0.000000000000000000 ) ) ;
#13207 = AXIS2_PLACEMENT_3D ( 'NONE', #15615, #20986, #10694 ) ;
#13208 = ORIENTED_EDGE ( 'NONE', *, *, #19964, .T. ) ;
#13209 = CARTESIAN_POINT ( 'NONE',  ( -60.59999999999998010, -2.408745774756101188, -1.060314564156378037 ) ) ;
#13210 = PLANE ( 'NONE',  #14676 ) ;
#13211 = DIRECTION ( 'NONE',  ( 0.000000000000000000, -8.881784197001252323E-16, -1.000000000000000000 ) ) ;
#13212 = ADVANCED_FACE ( 'NONE', ( #1677, #1843 ), #9462, .T. ) ;
#13213 =( BOUNDED_SURFACE ( )  B_SPLINE_SURFACE ( 2, 3, ( 
 ( #22350, #19819, #2870, #12219, #7478, #2714, #21903, #5094, #19674, #186, #7764, #2414, #14744, #19513, #12357, #24713, #17284, #5235 ),
 ( #7313, #14888, #14596, #3025, #12075, #9557, #28857, #7169, #16831, #16981, #14428, #21752, #41, #26632, #4939, #24262, #3794, #3338 ),
 ( #1117, #25186, #8239, #27545, #12816, #20448, #13141, #15532, #18233, #20302, #22829, #800, #17904, #3644, #27246, #27869, #6186, #15830 ),
 ( #20148, #19970, #8391, #10921, #10300, #20613, #5709, #5563, #29930, #25483, #18076, #29774, #10766, #15689, #13435, #30074, #29605, #27398 ),
 ( #15212, #1258, #13280, #8094, #972, #27720, #5871, #24858, #3500, #7934, #15360, #6038, #12989, #22968, #22675, #25339, #10623, #17760 ) ),
 .UNSPECIFIED., .F., .F., .F. ) 
 B_SPLINE_SURFACE_WITH_KNOTS ( ( 3, 2, 3 ),
 ( 4, 2, 2, 2, 2, 2, 2, 2, 4 ),
 ( -0.01000000000000000021, 0.000000000000000000, 1.000000000000000000 ),
 ( 1.413716694115406902, 1.826050729899067360, 2.238384765682727817, 2.650718801466387831, 3.063052837250048288, 3.475386873033708746, 3.887720908817368759, 4.300054944601029661, 4.712388980384689674 ),
 .UNSPECIFIED. ) 
 GEOMETRIC_REPRESENTATION_ITEM ( )  RATIONAL_B_SPLINE_SURFACE ( (
 ( 1.000000000000000000, 1.000000000000000000, 1.000000000000000000, 1.000000000000000000, 1.000000000000000000, 1.000000000000000000, 1.000000000000000000, 1.000000000000000000, 1.000000000000000000, 1.000000000000000000, 1.000000000000000000, 1.000000000000000000, 1.000000000000000000, 1.000000000000000000, 1.000000000000000000, 1.000000000000000000, 1.000000000000000000, 1.000000000000000000),
 ( 1.000000000000000000, 1.000000000000000000, 1.000000000000000000, 1.000000000000000000, 1.000000000000000000, 1.000000000000000000, 1.000000000000000000, 1.000000000000000000, 1.000000000000000000, 1.000000000000000000, 1.000000000000000000, 1.000000000000000000, 1.000000000000000000, 1.000000000000000000, 1.000000000000000000, 1.000000000000000000, 1.000000000000000000, 1.000000000000000000),
 ( 1.000000000000000000, 1.000000000000000000, 1.000000000000000000, 1.000000000000000000, 1.000000000000000000, 1.000000000000000000, 1.000000000000000000, 1.000000000000000000, 1.000000000000000000, 1.000000000000000000, 1.000000000000000000, 1.000000000000000000, 1.000000000000000000, 1.000000000000000000, 1.000000000000000000, 1.000000000000000000, 1.000000000000000000, 1.000000000000000000),
 ( 0.7071067811865476838, 0.7071067811865476838, 0.7071067811865475727, 0.7071067811865475727, 0.7071067811865476838, 0.7071067811865476838, 0.7071067811865475727, 0.7071067811865475727, 0.7071067811865473507, 0.7071067811865473507, 0.7071067811865479058, 0.7071067811865479058, 0.7071067811865475727, 0.7071067811865475727, 0.7071067811865463515, 0.7071067811865463515, 0.7071067811865475727, 0.7071067811865475727),
 ( 1.000000000000000000, 1.000000000000000000, 1.000000000000000000, 1.000000000000000000, 1.000000000000000000, 1.000000000000000000, 1.000000000000000000, 1.000000000000000000, 1.000000000000000000, 1.000000000000000000, 1.000000000000000000, 1.000000000000000000, 1.000000000000000000, 1.000000000000000000, 1.000000000000000000, 1.000000000000000000, 1.000000000000000000, 1.000000000000000000) ) ) 
 REPRESENTATION_ITEM ( '' )  SURFACE ( )  );
#13214 = CARTESIAN_POINT ( 'NONE',  ( 15.03925126672132961, 0.000000000000000000, 5.200000000000000178 ) ) ;
#13215 = CARTESIAN_POINT ( 'NONE',  ( -59.20655989232412963, 1.962990915244722245, 3.399999999999796962 ) ) ;
#13216 = CARTESIAN_POINT ( 'NONE',  ( 15.59055531549693541, 3.917775493694363398, 3.727542820438278337 ) ) ;
#13217 = AXIS2_PLACEMENT_3D ( 'NONE', #224, #29353, #7663 ) ;
#13218 = DIRECTION ( 'NONE',  ( 2.614375865348241018E-16, -0.2008964009354148039, 0.9796124928211140670 ) ) ;
#13219 = CARTESIAN_POINT ( 'NONE',  ( 58.66122331388437772, -0.5173534011631325535, 1.802520131073039433 ) ) ;
#13221 = CARTESIAN_POINT ( 'NONE',  ( 64.95000000000001705, 1.401298464324817071E-42, -6.803151388735846952E-13 ) ) ;
#13220 = LINE ( 'NONE', #18166, #30647 ) ;
#13222 = LINE ( 'NONE', #22906, #26696 ) ;
#13223 = AXIS2_PLACEMENT_3D ( 'NONE', #24018, #7388, #31140 ) ;
#13224 = EDGE_CURVE ( 'NONE', #11119, #16069, #6924, .T. ) ;
#13225 = CARTESIAN_POINT ( 'NONE',  ( 58.45000000000001705, 0.000000000000000000, 0.000000000000000000 ) ) ;
#13226 = ORIENTED_EDGE ( 'NONE', *, *, #22402, .F. ) ;
#13227 = CARTESIAN_POINT ( 'NONE',  ( 54.28867365409860213, 5.640057820322910587, -1.963089969304966820 ) ) ;
#13228 = EDGE_LOOP ( 'NONE', ( #18220, #2113, #15091, #26735 ) ) ;
#13229 = CARTESIAN_POINT ( 'NONE',  ( -59.45655989232410121, 1.962990915244762435, -3.400000000000193534 ) ) ;
#13230 = VERTEX_POINT ( 'NONE', #2008 ) ;
#13231 = CARTESIAN_POINT ( 'NONE',  ( -54.59585481156724285, -2.489203624310586616, 2.804704140674918023 ) ) ;
#13233 = CARTESIAN_POINT ( 'NONE',  ( -54.49999999999996447, -1.399999999999979039, -3.959797974644881258 ) ) ;
#13232 = DIRECTION ( 'NONE',  ( 1.000000000000000000, 1.018631342913014973E-14, 0.000000000000000000 ) ) ;
#13234 = ORIENTED_EDGE ( 'NONE', *, *, #18915, .T. ) ;
#13235 = ORIENTED_EDGE ( 'NONE', *, *, #8809, .F. ) ;
#13236 = DIRECTION ( 'NONE',  ( 0.000000000000000000, -0.9996898646859343485, -0.02490330187381116153 ) ) ;
#13237 = CARTESIAN_POINT ( 'NONE',  ( 57.02474788916244108, -0.7434350531339385393, -1.784201504348416067 ) ) ;
#13238 = EDGE_LOOP ( 'NONE', ( #253, #13062, #15634, #17459 ) ) ;
#13240 = LINE ( 'NONE', #22926, #14530 ) ;
#13239 = FACE_OUTER_BOUND ( 'NONE', #26029, .T. ) ;
#13241 = CYLINDRICAL_SURFACE ( 'NONE', #4858, 1.000000000000000000 ) ;
#13242 = VERTEX_POINT ( 'NONE', #6453 ) ;
#13243 = CARTESIAN_POINT ( 'NONE',  ( 58.74154451056406856, 1.668374833164396387, -0.8556855217776168088 ) ) ;
#13244 = EDGE_CURVE ( 'NONE', #12772, #4965, #5957, .T. ) ;
#13245 = CARTESIAN_POINT ( 'NONE',  ( -60.59999999999997300, -2.524216908331983866, -0.06288083723137120884 ) ) ;
#13246 = FACE_OUTER_BOUND ( 'NONE', #31051, .T. ) ;
#13247 = CARTESIAN_POINT ( 'NONE',  ( -55.07202994616204705, 2.078460969082674747, -3.600000000000187494 ) ) ;
#13248 = EDGE_CURVE ( 'NONE', #27015, #24287, #15047, .T. ) ;
#13249 = ORIENTED_EDGE ( 'NONE', *, *, #4791, .T. ) ;
#13250 = CARTESIAN_POINT ( 'NONE',  ( 15.86395258069111769, 2.563573972737327455, 4.761506352252367513 ) ) ;
#13251 = CIRCLE ( 'NONE', #25901, 0.4999999999999996114 ) ;
#13252 = DIRECTION ( 'NONE',  ( 0.000000000000000000, 0.000000000000000000, -1.000000000000000000 ) ) ;
#13253 = ADVANCED_FACE ( 'NONE', ( #11520 ), #21352, .T. ) ;
#13254 = PLANE ( 'NONE',  #1296 ) ;
#13255 = CARTESIAN_POINT ( 'NONE',  ( 58.75000000000004263, -1.972190280207336555, -0.1053114364790863067 ) ) ;
#13256 = CARTESIAN_POINT ( 'NONE',  ( 58.66120520762562762, 0.4851925435088347838, 1.811135885493970976 ) ) ;
#13257 = EDGE_LOOP ( 'NONE', ( #29720, #4689, #17306, #22910 ) ) ;
#13258 = DIRECTION ( 'NONE',  ( 0.000000000000000000, 0.000000000000000000, -1.000000000000000000 ) ) ;
#13259 = ORIENTED_EDGE ( 'NONE', *, *, #11354, .F. ) ;
#13260 = PRODUCT_DEFINITION_CONTEXT ( 'detailed design', #16079, 'design' ) ;
#13261 = DIRECTION ( 'NONE',  ( -1.499696682456116357E-15, 0.9030524935654929974, 0.4295302013422865883 ) ) ;
#13263 = DIRECTION ( 'NONE',  ( 1.000000000000000000, 1.047444401652940007E-14, 0.000000000000000000 ) ) ;
#13262 = DIRECTION ( 'NONE',  ( -1.476344542015126068E-16, -0.2069455031814144141, -0.9783524716138818356 ) ) ;
#13264 = ADVANCED_FACE ( 'NONE', ( #9297 ), #8975, .T. ) ;
#13265 = ORIENTED_EDGE ( 'NONE', *, *, #14201, .F. ) ;
#13266 = ORIENTED_EDGE ( 'NONE', *, *, #8821, .T. ) ;
#13267 = DIRECTION ( 'NONE',  ( 0.9396926207859090940, -0.008517430876162981890, 0.3419140708010995899 ) ) ;
#13268 = PLANE ( 'NONE',  #14641 ) ;
#13270 = CARTESIAN_POINT ( 'NONE',  ( -45.15971931043468146, -8.341470767433328331E-15, 0.000000000000000000 ) ) ;
#13269 = CARTESIAN_POINT ( 'NONE',  ( -60.25952994616203284, 3.117691453623994580, -1.800000000000200329 ) ) ;
#13271 = CARTESIAN_POINT ( 'NONE',  ( -58.23542740578360366, 0.7887156198831662968, -3.845940847736174284 ) ) ;
#13272 = AXIS2_PLACEMENT_3D ( 'NONE', #21925, #26014, #13974 ) ;
#13273 = DIRECTION ( 'NONE',  ( 1.000000000000000000, -0.000000000000000000, -0.000000000000000000 ) ) ;
#13274 = EDGE_CURVE ( 'NONE', #30652, #18266, #26069, .T. ) ;
#13275 = CARTESIAN_POINT ( 'NONE',  ( -59.38929772167340104, 2.352105592641139609, 1.259504355517284457 ) ) ;
#13276 = EDGE_CURVE ( 'NONE', #10683, #24584, #27183, .T. ) ;
#13277 = ADVANCED_FACE ( 'NONE', ( #18650 ), #6755, .T. ) ;
#13278 = VERTEX_POINT ( 'NONE', #30827 ) ;
#13279 = CARTESIAN_POINT ( 'NONE',  ( -60.88452994616204705, 3.117691453623979481, 1.799999999999795985 ) ) ;
#13280 = CARTESIAN_POINT ( 'NONE',  ( 52.05393800078982025, 4.345106731198570493, -1.549654688285467596 ) ) ;
#13281 = CARTESIAN_POINT ( 'NONE',  ( 58.75000000000001421, 0.5380862305915415922, -2.008165151417984351 ) ) ;
#13282 = CARTESIAN_POINT ( 'NONE',  ( 15.81621483022874131, -0.7811288459611355206, 5.350925378100964913 ) ) ;
#13283 = DIRECTION ( 'NONE',  ( 0.000000000000000000, 0.000000000000000000, 1.000000000000000000 ) ) ;
#13285 = CARTESIAN_POINT ( 'NONE',  ( 58.75000000000004263, -1.922185811753762241, -0.4146205000034702826 ) ) ;
#13284 = LINE ( 'NONE', #3345, #1388 ) ;
#13286 = CIRCLE ( 'NONE', #10772, 0.04999999999999988481 ) ;
#13287 = AXIS2_PLACEMENT_3D ( 'NONE', #358, #14761, #19534 ) ;
#13288 = DIRECTION ( 'NONE',  ( 3.489354422748178582E-15, -1.218509414717996338E-16, 1.000000000000000000 ) ) ;
#13290 = LINE ( 'NONE', #15701, #4382 ) ;
#13289 = DIRECTION ( 'NONE',  ( -1.000000000000000000, -1.018631342913014973E-14, -0.000000000000000000 ) ) ;
#13291 = VERTEX_POINT ( 'NONE', #11673 ) ;
#13292 = CARTESIAN_POINT ( 'NONE',  ( 50.40918227724429101, -1.198378070452279509, -3.921585382224056282 ) ) ;
#13293 = CARTESIAN_POINT ( 'NONE',  ( 58.65000000000002700, -0.8495817349406442620, 1.671477153793675896 ) ) ;
#13295 = DIRECTION ( 'NONE',  ( 1.000000000000000000, -1.219044193948983948E-29, 3.491481338843133355E-15 ) ) ;
#13294 = CARTESIAN_POINT ( 'NONE',  ( -59.19495429951913223, 2.548385458854359964, -0.9469503383365888149 ) ) ;
#13296 = DIRECTION ( 'NONE',  ( 1.000000000000000000, 3.053848253006669023E-16, -2.042510438544995415E-16 ) ) ;
#13297 = ADVANCED_FACE ( 'NONE', ( #28607, #2159 ), #13712, .T. ) ;
#13298 = ORIENTED_EDGE ( 'NONE', *, *, #5713, .F. ) ;
#13299 = CARTESIAN_POINT ( 'NONE',  ( 61.25000000000002132, 6.415596960124259844E-13, 3.111507638930570854E-58 ) ) ;
#13300 = CARTESIAN_POINT ( 'NONE',  ( -60.61746561950877066, -2.456658750590456908, -1.090869315165489128 ) ) ;
#13301 = EDGE_CURVE ( 'NONE', #14560, #2157, #13324, .T. ) ;
#13302 = ORIENTED_EDGE ( 'NONE', *, *, #12385, .T. ) ;
#13303 = ADVANCED_FACE ( 'NONE', ( #8448 ), #2400, .T. ) ;
#13304 = CARTESIAN_POINT ( 'NONE',  ( 46.90000000000001279, 1.734723475976807094E-15, 0.000000000000000000 ) ) ;
#13305 = ORIENTED_EDGE ( 'NONE', *, *, #6983, .F. ) ;
#13306 = CARTESIAN_POINT ( 'NONE',  ( 47.00000000000002132, 2.428612866367529932E-14, 0.000000000000000000 ) ) ;
#13307 = CARTESIAN_POINT ( 'NONE',  ( 22.04321716858594016, 7.679566743993225586, -1.425000000000077316 ) ) ;
#13308 = ORIENTED_EDGE ( 'NONE', *, *, #16519, .F. ) ;
#13309 = CARTESIAN_POINT ( 'NONE',  ( -56.00952994616203995, -3.117691453623961273, -1.800000000000214762 ) ) ;
#13310 = CARTESIAN_POINT ( 'NONE',  ( -59.20655989232412963, 1.962990915244722245, 3.399999999999796962 ) ) ;
#13311 = VERTEX_POINT ( 'NONE', #20805 ) ;
#13312 = DIRECTION ( 'NONE',  ( -1.000000000000000000, 0.000000000000000000, 1.047444401652940007E-14 ) ) ;
#13313 = ORIENTED_EDGE ( 'NONE', *, *, #29078, .F. ) ;
#13314 = CIRCLE ( 'NONE', #4736, 1.875000000000000222 ) ;
#13315 = EDGE_CURVE ( 'NONE', #4931, #4841, #20110, .T. ) ;
#13316 = ORIENTED_EDGE ( 'NONE', *, *, #8388, .F. ) ;
#13317 = CARTESIAN_POINT ( 'NONE',  ( -55.68749999999999289, 1.962990915244722689, 3.399999999999809841 ) ) ;
#13318 = DIRECTION ( 'NONE',  ( 0.000000000000000000, -0.2008964009354148594, 0.9796124928211140670 ) ) ;
#13319 = CARTESIAN_POINT ( 'NONE',  ( -61.34999999999997300, -2.482504579955461477, 0.4612981795977083577 ) ) ;
#13320 = DIRECTION ( 'NONE',  ( -1.000000000000000000, -2.586136946169074517E-16, 0.000000000000000000 ) ) ;
#13321 = CARTESIAN_POINT ( 'NONE',  ( -54.49999999999996447, 2.023778652682504319E-14, -3.400000000000193978 ) ) ;
#13323 = FACE_OUTER_BOUND ( 'NONE', #7156, .T. ) ;
#13322 = DIRECTION ( 'NONE',  ( 0.000000000000000000, 0.000000000000000000, -1.000000000000000000 ) ) ;
#13324 = LINE ( 'NONE', #5762, #16040 ) ;
#13325 = CARTESIAN_POINT ( 'NONE',  ( -62.39999999999998437, -2.749147127886319542, -0.06848408015297867413 ) ) ;
#13326 = CARTESIAN_POINT ( 'NONE',  ( 57.02131420290184138, 0.8120900198065377218, 2.469921935184963502 ) ) ;
#13327 = CARTESIAN_POINT ( 'NONE',  ( 15.03925126672132961, -0.9159215771349653590, 4.311190327366007047 ) ) ;
#13328 = AXIS2_PLACEMENT_3D ( 'NONE', #13583, #11550, #21058 ) ;
#13329 = ORIENTED_EDGE ( 'NONE', *, *, #83, .F. ) ;
#13330 = CARTESIAN_POINT ( 'NONE',  ( 50.40000000000001279, -0.7711297561635979125, 3.938774833552910692 ) ) ;
#13331 = ADVANCED_FACE ( 'NONE', ( #1310 ), #7412, .T. ) ;
#13332 = FACE_OUTER_BOUND ( 'NONE', #913, .T. ) ;
#13333 = EDGE_CURVE ( 'NONE', #15285, #7818, #16072, .T. ) ;
#13334 = ORIENTED_EDGE ( 'NONE', *, *, #2433, .T. ) ;
#13335 = ADVANCED_FACE ( 'NONE', ( #10982 ), #25385, .T. ) ;
#13336 = LINE ( 'NONE', #1324, #7319 ) ;
#13337 = PRODUCT_DEFINITION_SHAPE ( 'NONE', 'NONE',  #31329 ) ;
#13338 = AXIS2_PLACEMENT_3D ( 'NONE', #13747, #26432, #1716 ) ;
#13339 = PLANE ( 'NONE',  #16325 ) ;
#13341 = CARTESIAN_POINT ( 'NONE',  ( -59.40950473592805281, 2.424939707643913867, 1.246983968401823795 ) ) ;
#13340 = CARTESIAN_POINT ( 'NONE',  ( -57.24999999999997158, 2.944486372867092250, 1.699999999999808109 ) ) ;
#13342 = ORIENTED_EDGE ( 'NONE', *, *, #4524, .F. ) ;
#13343 = ORIENTED_EDGE ( 'NONE', *, *, #24307, .T. ) ;
#13344 = AXIS2_PLACEMENT_3D ( 'NONE', #9647, #15880, #16051 ) ;
#13345 = CARTESIAN_POINT ( 'NONE',  ( 58.65000000000003411, -1.571497941946429444, 1.022750809560281970 ) ) ;
#13346 = ORIENTED_EDGE ( 'NONE', *, *, #24338, .F. ) ;
#13347 = CARTESIAN_POINT ( 'NONE',  ( 58.66118217212468977, -1.615348343401803666, 0.9521303665437267361 ) ) ;
#13348 = ORIENTED_EDGE ( 'NONE', *, *, #21902, .F. ) ;
#13349 = CARTESIAN_POINT ( 'NONE',  ( 22.00282357718609916, 7.757228888719899906, -1.949999999999942002 ) ) ;
#13350 =( BOUNDED_CURVE ( )  B_SPLINE_CURVE ( 3, ( #7373, #1327, #3701, #25245 ),
 .UNSPECIFIED., .F., .T. ) 
 B_SPLINE_CURVE_WITH_KNOTS ( ( 4, 4 ),
 ( 0.000000000000000000, 1.570796326794896558 ),
 .UNSPECIFIED. ) 
 CURVE ( )  GEOMETRIC_REPRESENTATION_ITEM ( )  RATIONAL_B_SPLINE_CURVE ( ( 1.000000000000000000, 0.8047378541243649375, 0.8047378541243649375, 1.000000000000000000 ) ) 
 REPRESENTATION_ITEM ( '' )  );
#13351 = DIRECTION ( 'NONE',  ( 0.000000000000000000, 0.000000000000000000, -1.000000000000000000 ) ) ;
#13352 = FACE_OUTER_BOUND ( 'NONE', #17853, .T. ) ;
#13353 = EDGE_LOOP ( 'NONE', ( #5629, #28468, #18032, #24072 ) ) ;
#13354 = EDGE_CURVE ( 'NONE', #23640, #1093, #14559, .T. ) ;
#13355 = CARTESIAN_POINT ( 'NONE',  ( -58.49999999999997158, -1.184343223768573594, -3.558065644182727638 ) ) ;
#13356 = CARTESIAN_POINT ( 'NONE',  ( 51.69060524974059945, -0.7995873297237187094, -1.427997211815841050 ) ) ;
#13358 = CARTESIAN_POINT ( 'NONE',  ( -57.39405989232411542, -2.944486372867076263, -1.700000000000214451 ) ) ;
#13357 = AXIS2_PLACEMENT_3D ( 'NONE', #4684, #22118, #15122 ) ;
#13359 = CARTESIAN_POINT ( 'NONE',  ( 58.45000000000001705, -0.8000000000000000444, -2.421260002560650104 ) ) ;
#13360 = CARTESIAN_POINT ( 'NONE',  ( 16.08093158123429234, 2.941172302008990602, 4.539591111929677680 ) ) ;
#13361 = CARTESIAN_POINT ( 'NONE',  ( 50.55258015808398397, 0.05176326469760456073, 1.177580158083963324 ) ) ;
#13362 = CIRCLE ( 'NONE', #21022, 1.874999999999998668 ) ;
#13363 = FACE_OUTER_BOUND ( 'NONE', #273, .T. ) ;
#13365 = CARTESIAN_POINT ( 'NONE',  ( -56.70655989232412963, -3.399999999999991029, -2.112596694108398230E-13 ) ) ;
#13364 = DIRECTION ( 'NONE',  ( 0.000000000000000000, 0.000000000000000000, -1.000000000000000000 ) ) ;
#13366 = DIRECTION ( 'NONE',  ( 0.000000000000000000, 0.000000000000000000, 1.000000000000000000 ) ) ;
#13367 = DIRECTION ( 'NONE',  ( 1.000000000000000000, 3.053848253006669023E-16, -2.042510438544995415E-16 ) ) ;
#13368 = CARTESIAN_POINT ( 'NONE',  ( 47.00000000000002132, 2.428612866367529932E-14, -1.640996229256273308E-13 ) ) ;
#13369 = EDGE_LOOP ( 'NONE', ( #14580, #9935, #28374, #17563, #24134, #29687 ) ) ;
#13370 = AXIS2_PLACEMENT_3D ( 'NONE', #688, #3226, #27294 ) ;
#13371 = CARTESIAN_POINT ( 'NONE',  ( 54.18345076886460987, 5.675359767207155848, -2.050000000000190781 ) ) ;
#13372 = ORIENTED_EDGE ( 'NONE', *, *, #5129, .F. ) ;
#13373 = ADVANCED_FACE ( 'NONE', ( #15586 ), #27766, .F. ) ;
#13374 = EDGE_LOOP ( 'NONE', ( #26259, #3092, #4726, #9483 ) ) ;
#13375 = CARTESIAN_POINT ( 'NONE',  ( 52.91918222397625726, 8.304852724747879833, 2.049999999999815525 ) ) ;
#13376 = TOROIDAL_SURFACE ( 'NONE', #14415, 1.975000000000001865, 0.1000000000000000056 ) ;
#13377 = CARTESIAN_POINT ( 'NONE',  ( -57.34585481156722864, -1.184343223768586251, -3.558065644182725862 ) ) ;
#13379 = CARTESIAN_POINT ( 'NONE',  ( -44.59999999999996589, -1.499999999999978906, -3.959797974644846619 ) ) ;
#13378 = DIRECTION ( 'NONE',  ( -1.000000000000000000, 1.219044193948983948E-29, -3.491481338843133355E-15 ) ) ;
#13380 = ORIENTED_EDGE ( 'NONE', *, *, #21037, .F. ) ;
#13381 = CARTESIAN_POINT ( 'NONE',  ( 30.67858157643048500, 7.123080578496862714, -2.050000000000106848 ) ) ;
#13382 = DIRECTION ( 'NONE',  ( 0.000000000000000000, -0.9996898646859344595, -0.02490330187381124480 ) ) ;
#13383 = VERTEX_POINT ( 'NONE', #27915 ) ;
#13385 = DIRECTION ( 'NONE',  ( 1.000000000000000000, 3.054025858079668409E-16, -2.042474015755241579E-16 ) ) ;
#13384 = CARTESIAN_POINT ( 'NONE',  ( 50.31907412294955861, 1.391939743175939048, 3.849999999996903899 ) ) ;
#13386 = DIRECTION ( 'NONE',  ( 0.000000000000000000, -0.2793919678926574668, 0.9601771338024398528 ) ) ;
#13387 = EDGE_LOOP ( 'NONE', ( #15164, #18048, #9429, #19497 ) ) ;
#13388 = CARTESIAN_POINT ( 'NONE',  ( -36.39645873810162868, 4.962973169597041156, -2.162832296644261021 ) ) ;
#13389 = CARTESIAN_POINT ( 'NONE',  ( -54.49999999999997868, -3.188085654472696540, 1.181570928782897267 ) ) ;
#13390 = EDGE_CURVE ( 'NONE', #28206, #12308, #4676, .T. ) ;
#13391 = CARTESIAN_POINT ( 'NONE',  ( -36.72207054450175434, -2.602043737612686591, 4.741394629686801920 ) ) ;
#13392 = CARTESIAN_POINT ( 'NONE',  ( 57.05000000000001847, 0.7794871794871794934, 1.732743413496389717 ) ) ;
#13393 = CARTESIAN_POINT ( 'NONE',  ( -54.38452994616203995, 2.093608279459366986E-14, -3.600000000000193268 ) ) ;
#13394 = AXIS2_PLACEMENT_3D ( 'NONE', #7023, #25851, #11607 ) ;
#13395 = CIRCLE ( 'NONE', #19519, 3.524999999999996358 ) ;
#13396 = CIRCLE ( 'NONE', #11913, 2.549999999999999822 ) ;
#13397 = CIRCLE ( 'NONE', #31129, 1.599188152294417131 ) ;
#13398 = CARTESIAN_POINT ( 'NONE',  ( -60.64877780295373810, -2.511331634963794190, 0.9915305058630268231 ) ) ;
#13399 = AXIS2_PLACEMENT_3D ( 'NONE', #14197, #26239, #18656 ) ;
#13400 = CARTESIAN_POINT ( 'NONE',  ( 61.21683709729225598, 0.7974544867251615043, 1.837034727152569769 ) ) ;
#13401 = CYLINDRICAL_SURFACE ( 'NONE', #10834, 3.750000000000000444 ) ;
#13402 = DIRECTION ( 'NONE',  ( -1.000000000000000000, -0.000000000000000000, -0.000000000000000000 ) ) ;
#13403 = CARTESIAN_POINT ( 'NONE',  ( -54.39999999999996305, 1.400000000000023670, -3.959797974644871044 ) ) ;
#13404 = ORIENTED_EDGE ( 'NONE', *, *, #18377, .T. ) ;
#13405 = EDGE_CURVE ( 'NONE', #4631, #19660, #8990, .T. ) ;
#13406 = CARTESIAN_POINT ( 'NONE',  ( -56.93749999999996447, -3.399999999999991473, -2.119568960425587465E-13 ) ) ;
#13407 = ORIENTED_EDGE ( 'NONE', *, *, #31322, .F. ) ;
#13408 = CARTESIAN_POINT ( 'NONE',  ( -54.65835481156723574, -0.7533615035078032873, 3.673546848079177973 ) ) ;
#13410 = CARTESIAN_POINT ( 'NONE',  ( -54.49999999999997868, -0.9643027244899872175, 4.702139965541346278 ) ) ;
#13409 = CARTESIAN_POINT ( 'NONE',  ( 48.29999997257028355, 0.7904052113207087338, 4.025738854575411807 ) ) ;
#13411 = EDGE_CURVE ( 'NONE', #7915, #23830, #9346, .T. ) ;
#13412 = ORIENTED_EDGE ( 'NONE', *, *, #27079, .F. ) ;
#13413 = AXIS2_PLACEMENT_3D ( 'NONE', #24683, #7734, #4735 ) ;
#13414 = ORIENTED_EDGE ( 'NONE', *, *, #26476, .F. ) ;
#13415 = CARTESIAN_POINT ( 'NONE',  ( 53.91582462592153746, 6.672259099522125148, 1.484227406530594262 ) ) ;
#13416 = CIRCLE ( 'NONE', #19549, 0.2500000000000000555 ) ;
#13417 = CARTESIAN_POINT ( 'NONE',  ( 30.08242191457676995, 7.215531071606934965, -1.425000000000104849 ) ) ;
#13419 = CARTESIAN_POINT ( 'NONE',  ( 41.48619405472010868, -151.3359592902261852, 1.549999999999835953 ) ) ;
#13418 = CARTESIAN_POINT ( 'NONE',  ( 51.80000000000001137, -3.933368109459640660, -2.186004417993355542 ) ) ;
#13420 = EDGE_LOOP ( 'NONE', ( #12501, #29911, #11845, #17862 ) ) ;
#13421 = CARTESIAN_POINT ( 'NONE',  ( -56.73542740578360366, 0.7887156198831665188, -3.845940847736174284 ) ) ;
#13422 = AXIS2_PLACEMENT_3D ( 'NONE', #2927, #15417, #18132 ) ;
#13423 = AXIS2_PLACEMENT_3D ( 'NONE', #27481, #10234, #20539 ) ;
#13424 = DIRECTION ( 'NONE',  ( 1.000000000000000000, -0.000000000000000000, -0.000000000000000000 ) ) ;
#13425 = VECTOR ( 'NONE', #18778, 1000.000000000000000 ) ;
#13426 = CIRCLE ( 'NONE', #10426, 0.09999999999999995004 ) ;
#13427 = ADVANCED_FACE ( 'NONE', ( #29975 ), #3364, .T. ) ;
#13428 = CARTESIAN_POINT ( 'NONE',  ( -59.39436078131932817, 2.362401244263863997, 1.255862057041944535 ) ) ;
#13429 = VECTOR ( 'NONE', #19382, 1000.000000000000000 ) ;
#13430 = ADVANCED_BREP_SHAPE_REPRESENTATION ( '', ( #15704, #9018 ), #18167 ) ;
#13431 = ORIENTED_EDGE ( 'NONE', *, *, #6988, .T. ) ;
#13432 = B_SPLINE_CURVE_WITH_KNOTS ( 'NONE', 3,
 ( #6454, #16114, #25763, #13714, #27298, #27141 ),
 .UNSPECIFIED., .F., .F.,
 ( 4, 2, 4 ),
 ( 0.000000000000000000, 0.5000000000000000000, 1.000000000000000000 ),
 .UNSPECIFIED. ) ;
#13433 = AXIS2_PLACEMENT_3D ( 'NONE', #8575, #1450, #13468 ) ;
#13434 = CARTESIAN_POINT ( 'NONE',  ( 47.04913391925882138, -4.173104349845818462, -1.013903299540405367 ) ) ;
#13435 = CARTESIAN_POINT ( 'NONE',  ( 52.91918222397625016, 8.304852724747879833, -2.050000000000184119 ) ) ;
#13436 = CARTESIAN_POINT ( 'NONE',  ( -59.32267277260975646, 3.229247813185812888, 1.250136525132572451 ) ) ;
#13437 = DIRECTION ( 'NONE',  ( -1.000000000000000000, -3.053848253006669023E-16, 2.042510438544995415E-16 ) ) ;
#13438 = EDGE_CURVE ( 'NONE', #13819, #11263, #21076, .T. ) ;
#13439 = TOROIDAL_SURFACE ( 'NONE', #9925, 4.279289321881344144, 0.05000000000000000278 ) ;
#13440 = CYLINDRICAL_SURFACE ( 'NONE', #14521, 0.2499999999999997780 ) ;
#13442 = CARTESIAN_POINT ( 'NONE',  ( 47.10000000000003695, 6.982261990806648555E-14, 4.499999999999873879 ) ) ;
#13441 = CARTESIAN_POINT ( 'NONE',  ( 50.75360625943719839, -0.3719558471739983774, -1.344678919698702124 ) ) ;
#13443 = AXIS2_PLACEMENT_3D ( 'NONE', #7990, #17329, #15262 ) ;
#13444 = CARTESIAN_POINT ( 'NONE',  ( 52.64059584688627780, 4.063092876230792072, -2.046235406917140232 ) ) ;
#13445 = CIRCLE ( 'NONE', #17526, 0.05000000000000143219 ) ;
#13447 = CARTESIAN_POINT ( 'NONE',  ( -62.09999999999997300, -2.722373408723269161, -0.3890241620917929133 ) ) ;
#13446 = DIRECTION ( 'NONE',  ( -3.696862594069160905E-15, 0.9356455129756995337, -0.3529411764705844834 ) ) ;
#13448 = ORIENTED_EDGE ( 'NONE', *, *, #21330, .T. ) ;
#13449 = CIRCLE ( 'NONE', #23097, 2.549999999999999822 ) ;
#13450 = ADVANCED_FACE ( 'NONE', ( #8438 ), #18119, .T. ) ;
#13451 = CARTESIAN_POINT ( 'NONE',  ( 51.64333574538934357, 0.8318165372350859732, 1.569663068107118198 ) ) ;
#13452 = VECTOR ( 'NONE', #9865, 1000.000000000000114 ) ;
#13453 = ADVANCED_FACE ( 'NONE', ( #23178 ), #15404, .T. ) ;
#13454 = CARTESIAN_POINT ( 'NONE',  ( 58.45000000000001705, 0.8000000000000000444, 3.499999999999999556 ) ) ;
#13456 = DIRECTION ( 'NONE',  ( 1.047444401652940007E-14, 0.000000000000000000, 1.000000000000000000 ) ) ;
#13455 = DIRECTION ( 'NONE',  ( 0.000000000000000000, -0.9996898646859343485, -0.02490330187381123786 ) ) ;
#13458 = ADVANCED_FACE ( 'NONE', ( #27908 ), #11154, .T. ) ;
#13457 = CARTESIAN_POINT ( 'NONE',  ( 15.03925126672126211, -5.340403872473332925, 0.9205822173395827868 ) ) ;
#13459 = ORIENTED_EDGE ( 'NONE', *, *, #28420, .T. ) ;
#13460 = CARTESIAN_POINT ( 'NONE',  ( 53.76063741390514394, 7.747904304409473752, 2.049999999999812417 ) ) ;
#13461 = DIRECTION ( 'NONE',  ( 0.000000000000000000, 0.000000000000000000, 1.000000000000000000 ) ) ;
#13462 = B_SPLINE_CURVE_WITH_KNOTS ( 'NONE', 3,
 ( #17013, #26193, #2270, #12102, #2116, #19243, #28733, #29032, #28882, #2442 ),
 .UNSPECIFIED., .F., .F.,
 ( 4, 3, 3, 4 ),
 ( 1.252429503699613567E-17, 0.0001369029408772380434, 0.0002053557494648628661, 0.0002738089271645095064 ),
 .UNSPECIFIED. ) ;
#13463 = ORIENTED_EDGE ( 'NONE', *, *, #7884, .F. ) ;
#13464 = CARTESIAN_POINT ( 'NONE',  ( 41.48619405471885102, -151.3359592902622239, 1.949999999999835865 ) ) ;
#13465 = VERTEX_POINT ( 'NONE', #27590 ) ;
#13466 = VECTOR ( 'NONE', #7238, 1000.000000000000000 ) ;
#13467 = DIRECTION ( 'NONE',  ( 1.000000000000000000, 1.047444401652940007E-14, 0.000000000000000000 ) ) ;
#13468 = DIRECTION ( 'NONE',  ( 0.000000000000000000, 1.734723475976807094E-15, 1.000000000000000000 ) ) ;
#13469 = ORIENTED_EDGE ( 'NONE', *, *, #24601, .F. ) ;
#13470 = FILL_AREA_STYLE_COLOUR ( '', #22208 ) ;
#13471 = AXIS2_PLACEMENT_3D ( 'NONE', #7032, #14137, #198 ) ;
#13472 = CARTESIAN_POINT ( 'NONE',  ( -54.94702994616205416, 4.156921938165313968, -1.801810997602979365E-13 ) ) ;
#13473 = EDGE_CURVE ( 'NONE', #12424, #22845, #23681, .T. ) ;
#13474 = CARTESIAN_POINT ( 'NONE',  ( -58.89405989232411542, -2.944486372867076263, -1.700000000000219558 ) ) ;
#13475 = VERTEX_POINT ( 'NONE', #23009 ) ;
#13476 = CIRCLE ( 'NONE', #31195, 0.1499999999999999667 ) ;
#13477 = DIRECTION ( 'NONE',  ( -1.000000000000000000, 0.000000000000000000, 8.673617379884989994E-15 ) ) ;
#13478 = ORIENTED_EDGE ( 'NONE', *, *, #29535, .F. ) ;
#13479 = AXIS2_PLACEMENT_3D ( 'NONE', #12999, #979, #351 ) ;
#13480 = ORIENTED_EDGE ( 'NONE', *, *, #5431, .F. ) ;
#13481 = CIRCLE ( 'NONE', #13982, 3.624999999999996447 ) ;
#13482 = CARTESIAN_POINT ( 'NONE',  ( -57.87499999999997868, -3.920666489018319112E-15, 3.399999999999793854 ) ) ;
#13483 = CIRCLE ( 'NONE', #3893, 0.04999999999999991257 ) ;
#13484 = AXIS2_PLACEMENT_3D ( 'NONE', #21641, #11647, #4516 ) ;
#13485 = DIRECTION ( 'NONE',  ( 1.000000000000000000, -0.000000000000000000, -1.047444401652940007E-14 ) ) ;
#13486 = CARTESIAN_POINT ( 'NONE',  ( 48.50000000000002132, -1.391941090707485396, -3.750000000000022649 ) ) ;
#13487 = CARTESIAN_POINT ( 'NONE',  ( -56.56249999999997158, 3.400000000000008349, -1.863919195461975120E-13 ) ) ;
#13488 = ADVANCED_FACE ( 'NONE', ( #11122 ), #17644, .F. ) ;
#13489 = DIRECTION ( 'NONE',  ( 1.000000000000000000, 0.000000000000000000, 0.000000000000000000 ) ) ;
#13490 = EDGE_CURVE ( 'NONE', #5852, #3831, #29155, .T. ) ;
#13492 = DIRECTION ( 'NONE',  ( -1.000000000000000000, -0.000000000000000000, 0.000000000000000000 ) ) ;
#13491 = DIRECTION ( 'NONE',  ( 1.000000000000000000, -0.000000000000000000, 0.000000000000000000 ) ) ;
#13493 = VECTOR ( 'NONE', #17590, 999.9999999999998863 ) ;
#13494 = VECTOR ( 'NONE', #13378, 1000.000000000000000 ) ;
#13495 =( LENGTH_UNIT ( ) NAMED_UNIT ( * ) SI_UNIT ( .MILLI., .METRE. ) );
#13496 = CARTESIAN_POINT ( 'NONE',  ( -59.60675767627765964, 2.338930541566064392, -1.245993773302328744 ) ) ;
#13497 = CARTESIAN_POINT ( 'NONE',  ( 58.45000000000001705, -0.8000000000000000444, 2.421260002560650104 ) ) ;
#13498 = CARTESIAN_POINT ( 'NONE',  ( 58.75000000000003553, -1.652350234724367262, -1.065927491743898115 ) ) ;
#13500 = CARTESIAN_POINT ( 'NONE',  ( 57.00000000000001421, 0.7263196003080392149, -2.437012689524181486 ) ) ;
#13499 = AXIS2_PLACEMENT_3D ( 'NONE', #2342, #29395, #4705 ) ;
#13501 = ADVANCED_FACE ( 'NONE', ( #27439 ), #5752, .F. ) ;
#13502 = CARTESIAN_POINT ( 'NONE',  ( -59.29999999999994742, 2.202783890937385358, 2.955168114964210613 ) ) ;
#13503 = ORIENTED_EDGE ( 'NONE', *, *, #20264, .T. ) ;
#13504 = CARTESIAN_POINT ( 'NONE',  ( 51.78416995154973534, 0.8999235898787812937, -1.360374659026170718 ) ) ;
#13505 = EDGE_CURVE ( 'NONE', #5427, #23231, #20876, .T. ) ;
#13506 = CARTESIAN_POINT ( 'NONE',  ( -36.40878371307407235, -0.9780988077348349297, -5.318542208600382182 ) ) ;
#13507 = TOROIDAL_SURFACE ( 'NONE', #14008, 3.525000000000025224, 0.1000000000000000056 ) ;
#13508 = ORIENTED_EDGE ( 'NONE', *, *, #11831, .F. ) ;
#13509 = CIRCLE ( 'NONE', #17071, 3.750000000000000444 ) ;
#13510 = AXIS2_PLACEMENT_3D ( 'NONE', #2194, #28488, #16781 ) ;
#13511 = FACE_OUTER_BOUND ( 'NONE', #14478, .T. ) ;
#13512 = CARTESIAN_POINT ( 'NONE',  ( 61.20721104068438478, 0.7580073711298901395, -1.657084523451298308 ) ) ;
#13514 = CARTESIAN_POINT ( 'NONE',  ( 47.00000000000002842, -3.933368109459640660, 2.186004417993010485 ) ) ;
#13513 = CARTESIAN_POINT ( 'NONE',  ( -57.81249999999998579, -1.962990915244731793, 3.399999999999786304 ) ) ;
#13515 = VERTEX_POINT ( 'NONE', #6685 ) ;
#13516 = VERTEX_POINT ( 'NONE', #30757 ) ;
#13517 = DIRECTION ( 'NONE',  ( -1.000000000000000000, -0.000000000000000000, -0.000000000000000000 ) ) ;
#13518 = ORIENTED_EDGE ( 'NONE', *, *, #15172, .T. ) ;
#13519 = CARTESIAN_POINT ( 'NONE',  ( 58.65000038048067665, -1.580579251835808829, 1.008797009995473504 ) ) ;
#13520 = ORIENTED_EDGE ( 'NONE', *, *, #26125, .T. ) ;
#13521 = CARTESIAN_POINT ( 'NONE',  ( 60.87838368727346960, 0.5125281646394148627, 1.858409122016860371 ) ) ;
#13522 = CARTESIAN_POINT ( 'NONE',  ( -62.06710100716625789, -2.637635658083895329, 0.1963493119579511614 ) ) ;
#13523 = VECTOR ( 'NONE', #30348, 1000.000000000000000 ) ;
#13524 = CARTESIAN_POINT ( 'NONE',  ( -54.46614378277664059, -2.255560380866761250, -2.805788190199900889 ) ) ;
#13525 = ORIENTED_EDGE ( 'NONE', *, *, #24118, .F. ) ;
#13526 = AXIS2_PLACEMENT_3D ( 'NONE', #17265, #12056, #5375 ) ;
#13527 = CARTESIAN_POINT ( 'NONE',  ( 51.87416143049284756, 8.598705507415683513, 1.949999999999818767 ) ) ;
#13528 = DIRECTION ( 'NONE',  ( 1.000000000000000000, 3.054025858079668409E-16, -2.042474015755241579E-16 ) ) ;
#13529 = CARTESIAN_POINT ( 'NONE',  ( 57.02131420290184138, -0.8120900198065377218, -2.469921935184963502 ) ) ;
#13530 = CARTESIAN_POINT ( 'NONE',  ( 52.16611735465139077, 8.588510181886395145, -1.949999998429221337 ) ) ;
#13531 = EDGE_CURVE ( 'NONE', #1995, #4702, #9943, .T. ) ;
#13532 = CARTESIAN_POINT ( 'NONE',  ( 58.74999999305994436, 1.382203543031596649, 1.345908541131239478 ) ) ;
#13533 = ADVANCED_FACE ( 'NONE', ( #21589 ), #2088, .F. ) ;
#13534 = DIRECTION ( 'NONE',  ( 1.000000000000000000, 0.000000000000000000, 0.000000000000000000 ) ) ;
#13535 = EDGE_CURVE ( 'NONE', #7542, #14261, #26705, .T. ) ;
#13536 = CARTESIAN_POINT ( 'NONE',  ( 57.00000000000001421, 0.6999999999999999556, -1.820027472320129736 ) ) ;
#13538 = FACE_OUTER_BOUND ( 'NONE', #3119, .T. ) ;
#13537 = CARTESIAN_POINT ( 'NONE',  ( 51.13341687362769505, -0.9248174436469303039, 1.495576127286106338 ) ) ;
#13539 = CARTESIAN_POINT ( 'NONE',  ( -59.49861073854652460, -2.239724662550681700, 1.422539515414428024 ) ) ;
#13540 = DIRECTION ( 'NONE',  ( -1.000000000000000000, 0.000000000000000000, 1.047444401652940007E-14 ) ) ;
#13541 = DIRECTION ( 'NONE',  ( -1.000000000000000000, -3.054025858079668409E-16, 2.042474015755241579E-16 ) ) ;
#13542 = ORIENTED_EDGE ( 'NONE', *, *, #4131, .T. ) ;
#13543 = AXIS2_PLACEMENT_3D ( 'NONE', #19249, #28887, #21155 ) ;
#13544 = CARTESIAN_POINT ( 'NONE',  ( 54.04559870188514736, 5.332923641039334584, -2.050000000000188116 ) ) ;
#13545 = VERTEX_POINT ( 'NONE', #4149 ) ;
#13546 = ORIENTED_EDGE ( 'NONE', *, *, #20722, .F. ) ;
#13547 = CARTESIAN_POINT ( 'NONE',  ( 51.52211690305919944, -3.792101016927673207, 1.560991511224173900 ) ) ;
#13548 = ORIENTED_EDGE ( 'NONE', *, *, #6577, .F. ) ;
#13549 =( BOUNDED_CURVE ( )  B_SPLINE_CURVE ( 2, ( #31179, #1893, #11558, #16454, #4425, #23902, #2195, #13590, #14073 ),
 .UNSPECIFIED., .F., .T. ) 
 B_SPLINE_CURVE_WITH_KNOTS ( ( 3, 2, 2, 2, 3 ),
 ( 0.1388888888888888951, 0.1481481481481481399, 0.1666666666666666574, 0.1851851851851851749, 0.1944444444444444475 ),
 .UNSPECIFIED. ) 
 CURVE ( )  GEOMETRIC_REPRESENTATION_ITEM ( )  RATIONAL_B_SPLINE_CURVE ( ( 0.9330127018922192983, 0.9330127018922194093, 1.000000000000000000, 0.8660254037844387076, 1.000000000000000000, 0.8660254037844387076, 1.000000000000000000, 0.9330127018922191873, 0.9330127018922192983 ) ) 
 REPRESENTATION_ITEM ( '' )  );
#13550 = CARTESIAN_POINT ( 'NONE',  ( 53.12888913849685224, 4.216863368992567196, 2.049999999999814637 ) ) ;
#13551 = CARTESIAN_POINT ( 'NONE',  ( -56.15835481156723574, -0.8699069336946627651, 4.241846523238430144 ) ) ;
#13553 = CARTESIAN_POINT ( 'NONE',  ( 51.30415252705748941, -3.900546889229941971, -1.266936454265872314 ) ) ;
#13552 = CARTESIAN_POINT ( 'NONE',  ( 60.99999997330887425, -0.8151934526808929382, 1.407049160682770417 ) ) ;
#13554 = VERTEX_POINT ( 'NONE', #25993 ) ;
#13555 = EDGE_LOOP ( 'NONE', ( #9220, #6607, #13159, #10587 ) ) ;
#13556 = CARTESIAN_POINT ( 'NONE',  ( 32.27298585237639372, 7.910008090200282282, -2.050000000000112177 ) ) ;
#13557 = CARTESIAN_POINT ( 'NONE',  ( 47.07708546080151280, 8.766223091587681537, 1.549999999999835953 ) ) ;
#13558 = VERTEX_POINT ( 'NONE', #4299 ) ;
#13560 = DIRECTION ( 'NONE',  ( 2.117927888850091331E-16, -0.02490330187381135929, 0.9996898646859343485 ) ) ;
#13559 = CARTESIAN_POINT ( 'NONE',  ( 52.20711756518982583, 0.7500000000005468959, 1.718465885608440269 ) ) ;
#13561 = CARTESIAN_POINT ( 'NONE',  ( -54.49999999999997868, 2.818925648462311528E-15, 9.856100559121352825E-17 ) ) ;
#13562 = ORIENTED_EDGE ( 'NONE', *, *, #16519, .T. ) ;
#13563 = CARTESIAN_POINT ( 'NONE',  ( 51.25000000000001421, 5.368152558471320595E-13, 3.111507638930570854E-58 ) ) ;
#13564 = CARTESIAN_POINT ( 'NONE',  ( -54.49999999999996447, -1.599999999999981215, -3.363870538531692489 ) ) ;
#13565 = DIRECTION ( 'NONE',  ( 1.000000000000000000, -1.219044193948983948E-29, 3.491481338843133355E-15 ) ) ;
#13566 = LINE ( 'NONE', #20570, #17271 ) ;
#13567 = CARTESIAN_POINT ( 'NONE',  ( -56.00952994616203995, -3.117691453623963938, -1.800000000000210099 ) ) ;
#13568 = CIRCLE ( 'NONE', #20679, 1.000000000000000000 ) ;
#13569 =( GEOMETRIC_REPRESENTATION_CONTEXT ( 3 ) GLOBAL_UNCERTAINTY_ASSIGNED_CONTEXT ( ( #12052 ) ) GLOBAL_UNIT_ASSIGNED_CONTEXT ( ( #25837, #26316, #28849 ) ) REPRESENTATION_CONTEXT ( 'NONE', 'WORKASPACE' ) );
#13570 = EDGE_CURVE ( 'NONE', #3568, #1750, #30659, .T. ) ;
#13571 = CARTESIAN_POINT ( 'NONE',  ( 15.17256654081422163, 3.426725948577415526, 3.937891352654330213 ) ) ;
#13572 = CARTESIAN_POINT ( 'NONE',  ( -58.98542740578360366, 0.7887156198831923870, -3.845940847736168511 ) ) ;
#13573 = DIRECTION ( 'NONE',  ( 0.000000000000000000, 0.000000000000000000, 1.000000000000000000 ) ) ;
#13574 = CARTESIAN_POINT ( 'NONE',  ( 53.30089595108377409, 4.970692136877041811, 1.612337884061097348 ) ) ;
#13575 = CARTESIAN_POINT ( 'NONE',  ( 57.05000000000001847, -0.8000000000000000444, -2.421260002560649660 ) ) ;
#13576 = VERTEX_POINT ( 'NONE', #2239 ) ;
#13577 = EDGE_CURVE ( 'NONE', #21772, #15123, #11904, .T. ) ;
#13578 = CARTESIAN_POINT ( 'NONE',  ( 58.75000000000000711, 1.671477153794444170, 0.8495817349409561237 ) ) ;
#13579 = EDGE_LOOP ( 'NONE', ( #16107, #21485, #2559, #25988 ) ) ;
#13580 = CARTESIAN_POINT ( 'NONE',  ( 51.87582967299545800, 8.646477722258158138, 2.039222690360799728 ) ) ;
#13581 = CARTESIAN_POINT ( 'NONE',  ( 48.48122134030800368, 1.391940262981064214, 3.850000000000022293 ) ) ;
#13582 = VERTEX_POINT ( 'NONE', #21426 ) ;
#13583 = CARTESIAN_POINT ( 'NONE',  ( -59.29999999999997584, 2.330309927981284638E-15, 4.253626757584726372E-16 ) ) ;
#13584 = AXIS2_PLACEMENT_3D ( 'NONE', #4488, #16694, #30929 ) ;
#13585 = DIRECTION ( 'NONE',  ( 3.489354422748178582E-15, -1.218509414717996338E-16, 1.000000000000000000 ) ) ;
#13587 = CARTESIAN_POINT ( 'NONE',  ( -55.72085481156724285, 2.489203624310592833, -2.804704140674919799 ) ) ;
#13586 = CARTESIAN_POINT ( 'NONE',  ( -60.07202994616204705, 2.078460969082646770, 3.599999999999794031 ) ) ;
#13588 = ORIENTED_EDGE ( 'NONE', *, *, #19754, .F. ) ;
#13589 = CARTESIAN_POINT ( 'NONE',  ( -58.54792740578360366, -2.256877952708263635, 2.542931754211924744 ) ) ;
#13590 = CARTESIAN_POINT ( 'NONE',  ( -55.54806624327024167, 3.400000000000003908, 0.9110272542656333572 ) ) ;
#13591 = PRODUCT_CONTEXT ( 'NONE', #7524, 'mechanical' ) ;
#13592 = CARTESIAN_POINT ( 'NONE',  ( 50.80000000000002558, 0.2793919678926817252, 0.9601771338022635494 ) ) ;
#13593 = CARTESIAN_POINT ( 'NONE',  ( 22.61091062207858116, 6.637672121856524221, 2.049999999999720934 ) ) ;
#13594 = AXIS2_PLACEMENT_3D ( 'NONE', #15292, #11166, #11488 ) ;
#13595 = ORIENTED_EDGE ( 'NONE', *, *, #26940, .T. ) ;
#13596 = EDGE_CURVE ( 'NONE', #30852, #24179, #407, .T. ) ;
#13597 = CARTESIAN_POINT ( 'NONE',  ( 47.00587335483849216, -4.148449925053760090, -1.066233527417929761 ) ) ;
#13598 = CIRCLE ( 'NONE', #31316, 0.1000000000000000472 ) ;
#13599 = EDGE_CURVE ( 'NONE', #5317, #11953, #17107, .T. ) ;
#13600 = CARTESIAN_POINT ( 'NONE',  ( 61.24179192282278450, 0.9092026280841983832, -1.724287941703093630 ) ) ;
#13601 = CARTESIAN_POINT ( 'NONE',  ( -54.39999999999999147, 1.399999999999995914, 3.959797974644419849 ) ) ;
#13602 = CARTESIAN_POINT ( 'NONE',  ( 50.87477060347375613, 8.633605004118185988, 2.008578643762513050 ) ) ;
#13604 = CARTESIAN_POINT ( 'NONE',  ( -61.39999999999998437, -2.652806974455509170, 0.5026083527760007996 ) ) ;
#13603 = CARTESIAN_POINT ( 'NONE',  ( -61.34999999999997300, -2.661068980108069137, 0.4568499568858441773 ) ) ;
#13606 = AXIS2_PLACEMENT_3D ( 'NONE', #25443, #25597, #16267 ) ;
#13605 = CARTESIAN_POINT ( 'NONE',  ( 52.44049727168176389, 4.003343267869601263, -2.045783429862717995 ) ) ;
#13608 = CARTESIAN_POINT ( 'NONE',  ( -54.49999999999998579, 2.574607476582620347, -2.455998688455712120 ) ) ;
#13607 = DIRECTION ( 'NONE',  ( 0.000000000000000000, 0.9996898646859343485, 0.02490330187381124133 ) ) ;
#13609 = ORIENTED_EDGE ( 'NONE', *, *, #18865, .T. ) ;
#13610 = EDGE_CURVE ( 'NONE', #24812, #24817, #25527, .T. ) ;
#13611 = CARTESIAN_POINT ( 'NONE',  ( -62.06125279754600399, -2.664633900085208396, -0.3536699491376213977 ) ) ;
#13612 = DIRECTION ( 'NONE',  ( -1.000000000000000000, 0.000000000000000000, -0.000000000000000000 ) ) ;
#13614 = CARTESIAN_POINT ( 'NONE',  ( -59.61639066107911589, -2.342446846742894717, -1.242019481833328776 ) ) ;
#13613 = CARTESIAN_POINT ( 'NONE',  ( 58.72204580543404262, 1.816949979609431276, 0.4634803957301549260 ) ) ;
#13615 = CARTESIAN_POINT ( 'NONE',  ( 51.25000000000001421, 0.9938153758931693726, -1.589954715908409755 ) ) ;
#13616 = VERTEX_POINT ( 'NONE', #25690 ) ;
#13617 = CARTESIAN_POINT ( 'NONE',  ( 54.12895949791517580, 5.523355893849346110, 2.049999999999811084 ) ) ;
#13618 = CARTESIAN_POINT ( 'NONE',  ( 58.75000000000000711, 1.655311165516932803, 1.077297519405395310 ) ) ;
#13619 = VERTEX_POINT ( 'NONE', #28226 ) ;
#13621 = B_SPLINE_CURVE_WITH_KNOTS ( 'NONE', 3,
 ( #16019, #998, #20479, #30102 ),
 .UNSPECIFIED., .F., .F.,
 ( 4, 4 ),
 ( 0.000000000000000000, 0.0003845111068534305416 ),
 .UNSPECIFIED. ) ;
#13620 = CARTESIAN_POINT ( 'NONE',  ( -63.86464466094066239, 2.684522515537854481, 0.06687421464704730589 ) ) ;
#13622 = EDGE_CURVE ( 'NONE', #20056, #30092, #4539, .T. ) ;
#13623 = EDGE_LOOP ( 'NONE', ( #18754, #10406, #10763, #10207 ) ) ;
#13624 = CARTESIAN_POINT ( 'NONE',  ( 15.03925126672132961, 2.199885893005992799, -4.939696249117662141 ) ) ;
#13625 = CARTESIAN_POINT ( 'NONE',  ( -59.69999999999995310, -3.120538811013533032, -1.606221934090561687 ) ) ;
#13626 = PRODUCT_DEFINITION_FORMATION_WITH_SPECIFIED_SOURCE ( 'ANY', '', #23518, .NOT_KNOWN. ) ;
#13627 = ORIENTED_EDGE ( 'NONE', *, *, #5798, .F. ) ;
#13628 = SURFACE_STYLE_FILL_AREA ( #6210 ) ;
#13629 = CARTESIAN_POINT ( 'NONE',  ( 21.97322666366011745, 8.076925076899298617, 1.949999999999923128 ) ) ;
#13630 = AXIS2_PLACEMENT_3D ( 'NONE', #30056, #30226, #24990 ) ;
#13631 = CARTESIAN_POINT ( 'NONE',  ( -57.58155989232413674, -1.962990915244731571, 3.399999999999786748 ) ) ;
#13632 = AXIS2_PLACEMENT_3D ( 'NONE', #4472, #14125, #2089 ) ;
#13633 = ORIENTED_EDGE ( 'NONE', *, *, #1080, .F. ) ;
#13634 = DIRECTION ( 'NONE',  ( 0.000000000000000000, 0.000000000000000000, -1.000000000000000000 ) ) ;
#13635 = ORIENTED_EDGE ( 'NONE', *, *, #9863, .T. ) ;
#13636 = ORIENTED_EDGE ( 'NONE', *, *, #5205, .F. ) ;
#13637 = TOROIDAL_SURFACE ( 'NONE', #3057, 4.050000000000000711, 0.05000000000000000278 ) ;
#13638 = EDGE_CURVE ( 'NONE', #12162, #22178, #18121, .T. ) ;
#13639 = CARTESIAN_POINT ( 'NONE',  ( -56.56249999999997158, 3.925981830489463142, -1.866702293926226148E-13 ) ) ;
#13640 = EDGE_CURVE ( 'NONE', #13558, #6742, #24102, .T. ) ;
#13641 = CARTESIAN_POINT ( 'NONE',  ( 56.98113911906671092, -0.7884861235339004626, 2.477567088838556586 ) ) ;
#13642 = CARTESIAN_POINT ( 'NONE',  ( 22.04321716858594016, 7.679566743993225586, -1.425000000000077316 ) ) ;
#13644 = EDGE_CURVE ( 'NONE', #30441, #10060, #19215, .T. ) ;
#13643 = CARTESIAN_POINT ( 'NONE',  ( 64.95000000000005969, 4.837354856632045057E-16, 3.949999999999320277 ) ) ;
#13645 = DIRECTION ( 'NONE',  ( 0.000000000000000000, -1.000000000000000000, 0.000000000000000000 ) ) ;
#13646 = CIRCLE ( 'NONE', #21280, 0.04999999999999991257 ) ;
#13648 = DIRECTION ( 'NONE',  ( 0.000000000000000000, 0.000000000000000000, 1.000000000000000000 ) ) ;
#13647 = LINE ( 'NONE', #1947, #8435 ) ;
#13649 = CARTESIAN_POINT ( 'NONE',  ( -59.60063969940316753, 2.337287690019632880, -1.248834004845440715 ) ) ;
#13650 = CARTESIAN_POINT ( 'NONE',  ( -36.72207054450174724, -3.705258523861251430, -3.939862169952880411 ) ) ;
#13651 = DIRECTION ( 'NONE',  ( 1.000000000000000000, -7.137062321707633821E-17, 7.924918191883221096E-17 ) ) ;
#13652 = EDGE_CURVE ( 'NONE', #6633, #11953, #4873, .T. ) ;
#13653 = CARTESIAN_POINT ( 'NONE',  ( 50.55258015808398397, 5.295040916136730406E-13, 1.177580158083963546 ) ) ;
#13654 = CARTESIAN_POINT ( 'NONE',  ( 47.10000000000000853, 7.038595743567426471E-14, -4.600000000000200373 ) ) ;
#13655 = ORIENTED_EDGE ( 'NONE', *, *, #30536, .T. ) ;
#13657 = CARTESIAN_POINT ( 'NONE',  ( 51.80000000000001137, 4.350000000000017408, -1.550321101314903194 ) ) ;
#13656 = CARTESIAN_POINT ( 'NONE',  ( 51.11922224407864945, -0.9310536428529800901, -1.338077479437885131 ) ) ;
#13658 = AXIS2_PLACEMENT_3D ( 'NONE', #1896, #9020, #16456 ) ;
#13659 = ORIENTED_EDGE ( 'NONE', *, *, #6908, .F. ) ;
#13660 = SURFACE_STYLE_FILL_AREA ( #16366 ) ;
#13661 = LINE ( 'NONE', #23343, #20388 ) ;
#13663 = CARTESIAN_POINT ( 'NONE',  ( 57.05000000000001847, -0.7500000000000000000, -1.778341924377873751 ) ) ;
#13662 = CARTESIAN_POINT ( 'NONE',  ( -60.68749999999996447, -3.925981830489445379, -2.294491627273766911E-13 ) ) ;
#13664 = ORIENTED_EDGE ( 'NONE', *, *, #10781, .T. ) ;
#13665 = EDGE_CURVE ( 'NONE', #10573, #27318, #27632, .T. ) ;
#13666 = ORIENTED_EDGE ( 'NONE', *, *, #28044, .T. ) ;
#13667 = DIRECTION ( 'NONE',  ( -0.7071067811865561215, 8.659560562354918067E-17, -0.7071067811865388020 ) ) ;
#13668 = ORIENTED_EDGE ( 'NONE', *, *, #3153, .F. ) ;
#13669 = CARTESIAN_POINT ( 'NONE',  ( 51.02976068049075309, 1.019450805965481877, -1.268081568884019017 ) ) ;
#13670 =( BOUNDED_SURFACE ( )  B_SPLINE_SURFACE ( 3, 2, ( 
 ( #19079, #14304, #31085 ),
 ( #11631, #9410, #21310 ),
 ( #9729, #4649, #18918 ),
 ( #26495, #23975, #16372 ),
 ( #11934, #4800, #21621 ),
 ( #31258, #19389, #14459 ),
 ( #4496, #9582, #7341 ),
 ( #28407, #26018, #21149 ),
 ( #14150, #23826, #4327 ),
 ( #13980, #23674, #30939 ),
 ( #28559, #27112, #29804 ),
 ( #17461, #24579, #29476 ),
 ( #21928, #10327, #5432 ),
 ( #371, #209, #19998 ),
 ( #15087, #17168, #24743 ),
 ( #520, #5738, #29640 ) ),
 .UNSPECIFIED., .F., .F., .F. ) 
 B_SPLINE_SURFACE_WITH_KNOTS ( ( 4, 2, 2, 2, 2, 2, 2, 4 ),
 ( 3, 3 ),
 ( 0.001780502285214185815, 0.002558945925323762027, 0.002753556835351156189, 0.002948167745378550350, 0.003337389565433338673, 0.003726611385488126996, 0.004115833205542915318, 0.004894276845652491097 ),
 ( 0.000000000000000000, 1.000000000000000000 ),
 .UNSPECIFIED. ) 
 GEOMETRIC_REPRESENTATION_ITEM ( )  RATIONAL_B_SPLINE_SURFACE ( (
 ( 1.000000000000000000, 0.9418517008537251600, 1.000000000000000000),
 ( 1.000000000000000000, 0.9417987965885094015, 1.000000000000000000),
 ( 1.000000000000000000, 0.9418198861734091709, 1.000000000000000000),
 ( 1.000000000000000000, 0.9434060303845579476, 1.000000000000000000),
 ( 1.000000000000000000, 0.9437939819948207854, 1.000000000000000000),
 ( 1.000000000000000000, 0.9445989566712774677, 1.000000000000000000),
 ( 1.000000000000000000, 0.9450169930049769906, 1.000000000000000000),
 ( 1.000000000000000000, 0.9461610507673769987, 1.000000000000000000),
 ( 1.000000000000000000, 0.9467217966427221576, 1.000000000000000000),
 ( 1.000000000000000000, 0.9467345476124371384, 1.000000000000000000),
 ( 1.000000000000000000, 0.9461964028052877174, 1.000000000000000000),
 ( 1.000000000000000000, 0.9446801822473928079, 1.000000000000000000),
 ( 1.000000000000000000, 0.9437582546536690264, 1.000000000000000000),
 ( 1.000000000000000000, 0.9418129560295395164, 1.000000000000000000),
 ( 1.000000000000000000, 0.9418016889777716116, 1.000000000000000000),
 ( 1.000000000000000000, 0.9418517008537247159, 1.000000000000000000) ) ) 
 REPRESENTATION_ITEM ( '' )  SURFACE ( )  );
#13671 = DIRECTION ( 'NONE',  ( -1.040834085586084257E-14, 0.000000000000000000, -1.000000000000000000 ) ) ;
#13672 = ORIENTED_EDGE ( 'NONE', *, *, #5182, .T. ) ;
#13673 = CARTESIAN_POINT ( 'NONE',  ( 22.68548117337039471, 6.704541182151974255, -2.050000000000079314 ) ) ;
#13674 = FACE_OUTER_BOUND ( 'NONE', #15641, .T. ) ;
#13675 = LINE ( 'NONE', #28739, #26808 ) ;
#13676 = ORIENTED_EDGE ( 'NONE', *, *, #8420, .F. ) ;
#13677 = ORIENTED_EDGE ( 'NONE', *, *, #9841, .T. ) ;
#13678 = EDGE_CURVE ( 'NONE', #25510, #16074, #11985, .T. ) ;
#13679 = DIRECTION ( 'NONE',  ( 0.000000000000000000, 0.000000000000000000, 1.000000000000000000 ) ) ;
#13680 = ADVANCED_FACE ( 'NONE', ( #19366 ), #13213, .T. ) ;
#13681 = DIRECTION ( 'NONE',  ( -0.000000000000000000, -0.000000000000000000, 1.000000000000000000 ) ) ;
#13682 = CARTESIAN_POINT ( 'NONE',  ( -67.88621053311027254, -1.613288973786559444, -0.04018868625472774014 ) ) ;
#13683 = CIRCLE ( 'NONE', #18777, 0.4576450603546999840 ) ;
#13684 = ADVANCED_FACE ( 'NONE', ( #30243 ), #19566, .T. ) ;
#13685 = CARTESIAN_POINT ( 'NONE',  ( 58.73379417893121968, 1.381558089342225015, 1.267842757872280623 ) ) ;
#13686 = AXIS2_PLACEMENT_3D ( 'NONE', #2820, #17721, #29737 ) ;
#13687 = CARTESIAN_POINT ( 'NONE',  ( 48.40000000000001990, 2.428612866367529932E-14, 4.000000000000022204 ) ) ;
#13688 = DIRECTION ( 'NONE',  ( 1.000000000000000000, 1.047444401652940007E-14, 0.000000000000000000 ) ) ;
#13690 = CARTESIAN_POINT ( 'NONE',  ( 51.68195507589560123, -4.249103233463753071, 1.767380283559480958 ) ) ;
#13689 = CARTESIAN_POINT ( 'NONE',  ( -36.80043232705924083, -2.728070298465809618, 4.669343935538287305 ) ) ;
#13691 = CARTESIAN_POINT ( 'NONE',  ( 51.90000000000001279, -4.227689052994015206, 1.125730994152045916 ) ) ;
#13692 = CARTESIAN_POINT ( 'NONE',  ( -77.28999999999996362, -3.470778894058966809E-15, 5.300300110251643219E-15 ) ) ;
#13693 = DIRECTION ( 'NONE',  ( 1.000000000000000000, 1.047444401652940007E-14, 0.000000000000000000 ) ) ;
#13694 = CARTESIAN_POINT ( 'NONE',  ( 50.35762544161294585, 8.151359338959888845, -1.950000000000174927 ) ) ;
#13695 = ORIENTED_EDGE ( 'NONE', *, *, #15966, .F. ) ;
#13696 = AXIS2_PLACEMENT_3D ( 'NONE', #29874, #22301, #8498 ) ;
#13697 = VERTEX_POINT ( 'NONE', #17601 ) ;
#13698 = DIRECTION ( 'NONE',  ( 1.000000000000000000, 2.586136946169074517E-16, -0.000000000000000000 ) ) ;
#13699 = ORIENTED_EDGE ( 'NONE', *, *, #27412, .F. ) ;
#13700 = CARTESIAN_POINT ( 'NONE',  ( 52.05393800078974920, 4.345106731198625560, 2.049999999999818190 ) ) ;
#13701 = CARTESIAN_POINT ( 'NONE',  ( -55.53335481156722864, 3.238593381231848145, 2.874284765127022467 ) ) ;
#13703 = CARTESIAN_POINT ( 'NONE',  ( 36.50000000000002132, 0.7794871794871797155, 1.732743413496390161 ) ) ;
#13702 = DIRECTION ( 'NONE',  ( 3.489354422748178582E-15, -1.218509414717996338E-16, 1.000000000000000000 ) ) ;
#13704 = VERTEX_POINT ( 'NONE', #22501 ) ;
#13705 = ADVANCED_FACE ( 'NONE', ( #10466 ), #27369, .T. ) ;
#13706 = CARTESIAN_POINT ( 'NONE',  ( 15.03925126672132784, 5.086913985776164715, -1.171642053949048856 ) ) ;
#13707 = VERTEX_POINT ( 'NONE', #21395 ) ;
#13708 = EDGE_CURVE ( 'NONE', #21736, #26230, #18372, .T. ) ;
#13709 = DIRECTION ( 'NONE',  ( 0.9993908270191184107, -0.03489949670185085034, -3.491481338843133355E-15 ) ) ;
#13710 = ORIENTED_EDGE ( 'NONE', *, *, #25696, .F. ) ;
#13712 = PLANE ( 'NONE',  #7983 ) ;
#13711 = CARTESIAN_POINT ( 'NONE',  ( 69.20000000000001705, 0.7500000000000000000, -1.988246715074083237 ) ) ;
#13713 = EDGE_CURVE ( 'NONE', #24203, #2488, #26623, .T. ) ;
#13714 = CARTESIAN_POINT ( 'NONE',  ( 51.87453755317503834, 8.609476251808864333, -2.002198665876508521 ) ) ;
#13715 = ORIENTED_EDGE ( 'NONE', *, *, #25014, .F. ) ;
#13716 = DIRECTION ( 'NONE',  ( -1.047444401652940007E-14, 1.000000000000000000, 0.000000000000000000 ) ) ;
#13717 = CARTESIAN_POINT ( 'NONE',  ( -36.14504829323104218, -2.228024565339430385, 4.927420728799218885 ) ) ;
#13718 = CARTESIAN_POINT ( 'NONE',  ( 56.95000000000001705, 0.6999999999999999556, -1.820027472320129736 ) ) ;
#13719 = CARTESIAN_POINT ( 'NONE',  ( -57.94702994616203995, 4.156921938165313080, -1.906555437768272735E-13 ) ) ;
#13720 = VECTOR ( 'NONE', #6461, 1000.000000000000000 ) ;
#13721 = CARTESIAN_POINT ( 'NONE',  ( 15.22842924604237247, 3.779372845002901382, 3.883777290285411077 ) ) ;
#13722 = CARTESIAN_POINT ( 'NONE',  ( -59.29895813073913047, -2.232665607824515952, 2.564420458051888563 ) ) ;
#13723 = DIRECTION ( 'NONE',  ( 0.000000000000000000, 0.5333333333333335480, -0.8459051693633012903 ) ) ;
#13724 = DIRECTION ( 'NONE',  ( 1.015447888376667464E-14, 0.000000000000000000, 1.000000000000000000 ) ) ;
#13725 = DIRECTION ( 'NONE',  ( 0.000000000000000000, 0.9783524716136867694, -0.2069455031823359825 ) ) ;
#13726 = CARTESIAN_POINT ( 'NONE',  ( -35.85663232820592583, -0.4576450603546987073, 5.200000000000000178 ) ) ;
#13727 = CARTESIAN_POINT ( 'NONE',  ( 58.75000000000001421, 0.6373668173466265907, 1.895722432253563516 ) ) ;
#13728 = EDGE_LOOP ( 'NONE', ( #17736, #16152, #13202, #4506 ) ) ;
#13729 = CARTESIAN_POINT ( 'NONE',  ( 58.74999981196283727, 1.649561145038380028, 1.050519579373024426 ) ) ;
#13730 = ORIENTED_EDGE ( 'NONE', *, *, #24181, .F. ) ;
#13731 = AXIS2_PLACEMENT_3D ( 'NONE', #14346, #12144, #21823 ) ;
#13733 = CARTESIAN_POINT ( 'NONE',  ( 58.72204580543429842, -1.309860786662360832, 1.341784641881585971 ) ) ;
#13732 = CARTESIAN_POINT ( 'NONE',  ( 48.50000000000002132, 1.426739617975228525, 3.843750000000022649 ) ) ;
#13734 = EDGE_LOOP ( 'NONE', ( #24244, #31314, #19443, #9143, #11979, #5078 ) ) ;
#13735 = ADVANCED_FACE ( 'NONE', ( #14711 ), #12320, .T. ) ;
#13736 = DIRECTION ( 'NONE',  ( 0.000000000000000000, 0.000000000000000000, 1.000000000000000000 ) ) ;
#13737 = EDGE_CURVE ( 'NONE', #8353, #20985, #24171, .T. ) ;
#13738 = B_SPLINE_CURVE_WITH_KNOTS ( 'NONE', 3,
 ( #17754, #10148, #29306, #7621, #27394, #15207, #5232, #17900, #10617, #5705, #14739, #19815, #15354, #29447, #795, #25004, #3331, #12982 ),
 .UNSPECIFIED., .F., .F.,
 ( 4, 2, 2, 2, 2, 2, 2, 2, 4 ),
 ( 1.306736722590954369E-14, 0.0007570489093058673305, 0.001514097818598667423, 0.002271146727891467081, 0.003028195637184267174, 0.003785244546477067266, 0.004542293455769867358, 0.005299342365062667884, 0.006056391274355467542 ),
 .UNSPECIFIED. ) ;
#13739 = CARTESIAN_POINT ( 'NONE',  ( 50.78793970012934267, -0.4223115601891286874, -0.9680023493207206009 ) ) ;
#13740 = DIRECTION ( 'NONE',  ( 3.384826294588897856E-15, 0.000000000000000000, 1.000000000000000000 ) ) ;
#13741 = EDGE_CURVE ( 'NONE', #28051, #22264, #638, .T. ) ;
#13742 = ORIENTED_EDGE ( 'NONE', *, *, #26865, .F. ) ;
#13743 = CARTESIAN_POINT ( 'NONE',  ( -55.74999999999997158, -2.489203624310585283, 2.804704140674916690 ) ) ;
#13744 = CARTESIAN_POINT ( 'NONE',  ( 47.00000000000002132, -4.131056160354152240, -1.100000000000000089 ) ) ;
#13745 = CARTESIAN_POINT ( 'NONE',  ( 53.29166889513722793, 4.961539162849967433, -1.611464872099122481 ) ) ;
#13746 = DIRECTION ( 'NONE',  ( 0.000000000000000000, -1.000000000000000000, 0.000000000000000000 ) ) ;
#13747 = CARTESIAN_POINT ( 'NONE',  ( 64.00000000000001421, 1.163569835200988601E-28, -2.234548056859606357E-13 ) ) ;
#13748 = ORIENTED_EDGE ( 'NONE', *, *, #3117, .T. ) ;
#13749 = ADVANCED_FACE ( 'NONE', ( #24371 ), #15578, .F. ) ;
#13750 = CARTESIAN_POINT ( 'NONE',  ( 57.04171473382086077, -0.7493275531345221507, 1.778946371510476077 ) ) ;
#13751 = CARTESIAN_POINT ( 'NONE',  ( -63.82928932188132620, 2.649178141417727339, 0.06599374996560235240 ) ) ;
#13752 = CARTESIAN_POINT ( 'NONE',  ( 58.75000000000000711, 1.499837071477960304, 1.323060376182421782 ) ) ;
#13753 = CARTESIAN_POINT ( 'NONE',  ( -35.85663232820584057, -4.018128179617548312, -3.618665901676662244 ) ) ;
#13754 = CARTESIAN_POINT ( 'NONE',  ( 57.00000000000001421, -0.7058179832143345322, -2.448718171069995009 ) ) ;
#13756 = CARTESIAN_POINT ( 'NONE',  ( 69.25000000000000000, 0.7500000000000000000, -1.988246715074084126 ) ) ;
#13755 = DIRECTION ( 'NONE',  ( -1.000000000000000000, 1.219044193948983948E-29, -3.491481338843133355E-15 ) ) ;
#13757 = CARTESIAN_POINT ( 'NONE',  ( 47.02503650169320082, -4.051364836627049826, -1.951815467915571922 ) ) ;
#13759 = CARTESIAN_POINT ( 'NONE',  ( 61.25000000000001421, 1.000000000000641709, -1.586072192556190474 ) ) ;
#13758 = DIRECTION ( 'NONE',  ( 0.000000000000000000, -1.000000000000000000, 0.000000000000000000 ) ) ;
#13760 = ORIENTED_EDGE ( 'NONE', *, *, #24314, .F. ) ;
#13761 = DIRECTION ( 'NONE',  ( 0.000000000000000000, 0.000000000000000000, -1.000000000000000000 ) ) ;
#13762 = FACE_OUTER_BOUND ( 'NONE', #20044, .T. ) ;
#13763 = CIRCLE ( 'NONE', #2679, 0.4576450603546982632 ) ;
#13765 = DIRECTION ( 'NONE',  ( 0.000000000000000000, 0.000000000000000000, -1.000000000000000000 ) ) ;
#13764 = CARTESIAN_POINT ( 'NONE',  ( -59.69999999999997442, 8.366749974758454467E-15, -2.120534355533670266E-13 ) ) ;
#13766 = CARTESIAN_POINT ( 'NONE',  ( 15.76623786017565187, -5.175840503946257165, 1.569056257078743855 ) ) ;
#13767 = EDGE_LOOP ( 'NONE', ( #11371, #22607, #13226, #27895 ) ) ;
#13768 = ORIENTED_EDGE ( 'NONE', *, *, #8184, .F. ) ;
#13769 = CARTESIAN_POINT ( 'NONE',  ( 50.25000000000002132, 5.314096449039845576E-13, -0.8749999999999991118 ) ) ;
#13770 = CARTESIAN_POINT ( 'NONE',  ( 50.40000000000001990, -0.6304760106459028624, 3.950000000000022826 ) ) ;
#13771 = EDGE_CURVE ( 'NONE', #6209, #31257, #335, .T. ) ;
#13772 = EDGE_LOOP ( 'NONE', ( #8207, #4560, #28890, #878 ) ) ;
#13773 = CARTESIAN_POINT ( 'NONE',  ( 47.00000000000002132, -3.726179070414207040, -1.041421356237309581 ) ) ;
#13774 = ORIENTED_EDGE ( 'NONE', *, *, #28050, .T. ) ;
#13775 = CARTESIAN_POINT ( 'NONE',  ( 58.75000018803716273, 1.936004331707595894, 0.04945370822498024871 ) ) ;
#13776 = VERTEX_POINT ( 'NONE', #2203 ) ;
#13777 =( LENGTH_UNIT ( ) NAMED_UNIT ( * ) SI_UNIT ( .MILLI., .METRE. ) );
#13778 = CARTESIAN_POINT ( 'NONE',  ( -55.32202994616205416, -4.156921938165296204, -2.162464288268359870E-13 ) ) ;
#13779 = CARTESIAN_POINT ( 'NONE',  ( -57.33155989232411542, -1.962990915244706924, -3.400000000000209521 ) ) ;
#13780 = ORIENTED_EDGE ( 'NONE', *, *, #2713, .F. ) ;
#13781 = ORIENTED_EDGE ( 'NONE', *, *, #9569, .F. ) ;
#13782 = ORIENTED_EDGE ( 'NONE', *, *, #25467, .F. ) ;
#13783 = EDGE_CURVE ( 'NONE', #26230, #22920, #28967, .T. ) ;
#13784 = CARTESIAN_POINT ( 'NONE',  ( -55.13452994616203995, 2.093608279459367933E-14, -3.600000000000195932 ) ) ;
#13785 = CARTESIAN_POINT ( 'NONE',  ( -55.14405989232412253, -2.944486372867075819, -1.700000000000207345 ) ) ;
#13786 = CARTESIAN_POINT ( 'NONE',  ( 28.86359278493677039, 5.838313002610202140, -1.425000000000100409 ) ) ;
#13787 = VECTOR ( 'NONE', #24347, 1000.000000000000000 ) ;
#13788 = DIRECTION ( 'NONE',  ( 1.000000000000000000, 0.000000000000000000, -3.491481338843133355E-15 ) ) ;
#13789 = CARTESIAN_POINT ( 'NONE',  ( 57.05000000000001847, 0.7500000000000000000, 2.421260002560649660 ) ) ;
#13790 = B_SPLINE_CURVE_WITH_KNOTS ( 'NONE', 3,
 ( #5260, #14768, #24884, #29955, #29636, #22073 ),
 .UNSPECIFIED., .F., .F.,
 ( 4, 2, 4 ),
 ( 0.0001690239924570914956, 0.0002786457176453306390, 0.0003882674428335697553 ),
 .UNSPECIFIED. ) ;
#13792 = CARTESIAN_POINT ( 'NONE',  ( 50.87477060347373481, 8.633605004118187765, -2.050000000000176570 ) ) ;
#13791 = CARTESIAN_POINT ( 'NONE',  ( 69.20000000000001705, -0.7500000000000000000, -2.288246715074080839 ) ) ;
#13793 = PRESENTATION_STYLE_ASSIGNMENT (( #28234 ) ) ;
#13794 = CARTESIAN_POINT ( 'NONE',  ( -54.49999999999997868, -4.179189514726507682, 0.8999999999999994671 ) ) ;
#13795 = CARTESIAN_POINT ( 'NONE',  ( 15.22780280894161287, 5.340403875750862284, -0.9205822004573419592 ) ) ;
#13796 = CARTESIAN_POINT ( 'NONE',  ( 58.72204580543421315, -1.635081356932600372, -0.9179489429353107077 ) ) ;
#13797 = DIRECTION ( 'NONE',  ( -1.000000000000000000, -3.053848253006669023E-16, 2.042510438544995415E-16 ) ) ;
#13798 = DIRECTION ( 'NONE',  ( 1.054009200593503061E-14, 0.000000000000000000, 1.000000000000000000 ) ) ;
#13799 = ORIENTED_EDGE ( 'NONE', *, *, #9009, .T. ) ;
#13800 = DIRECTION ( 'NONE',  ( 0.000000000000000000, 0.000000000000000000, 1.000000000000000000 ) ) ;
#13801 = CARTESIAN_POINT ( 'NONE',  ( 51.80000000000002558, 6.475000000000062705, 1.949999999999818767 ) ) ;
#13802 = EDGE_CURVE ( 'NONE', #27700, #16231, #28202, .T. ) ;
#13803 = ORIENTED_EDGE ( 'NONE', *, *, #3684, .F. ) ;
#13804 = CARTESIAN_POINT ( 'NONE',  ( 54.15675781068899397, 5.684314874070254042, -2.050000000000189004 ) ) ;
#13805 = AXIS2_PLACEMENT_3D ( 'NONE', #12919, #914, #2799 ) ;
#13806 = CARTESIAN_POINT ( 'NONE',  ( 51.70000000000001705, -4.259181259350203419, -1.000000000000000000 ) ) ;
#13807 = CARTESIAN_POINT ( 'NONE',  ( -59.81249999999995026, -1.962990915244707368, -3.400000000000219291 ) ) ;
#13808 = ORIENTED_EDGE ( 'NONE', *, *, #18332, .F. ) ;
#13809 = ORIENTED_EDGE ( 'NONE', *, *, #22998, .T. ) ;
#13810 = CARTESIAN_POINT ( 'NONE',  ( 51.80290302015603032, -4.086844330038878148, -2.115703333131829567 ) ) ;
#13811 = ORIENTED_EDGE ( 'NONE', *, *, #24504, .T. ) ;
#13812 = CARTESIAN_POINT ( 'NONE',  ( 51.08379317338046377, 0.8723108729837811826, -1.374656996893403038 ) ) ;
#13813 = DIRECTION ( 'NONE',  ( 1.000000000000000000, 3.054025858079668409E-16, -2.042474015755241579E-16 ) ) ;
#13814 = ORIENTED_EDGE ( 'NONE', *, *, #7161, .F. ) ;
#13815 = CARTESIAN_POINT ( 'NONE',  ( 56.95000000000001705, 0.000000000000000000, 1.949999999999999956 ) ) ;
#13816 = CARTESIAN_POINT ( 'NONE',  ( -60.59999999999997300, 2.524216908331987419, 0.06288083723137531666 ) ) ;
#13817 = CYLINDRICAL_SURFACE ( 'NONE', #7099, 2.000000000000000000 ) ;
#13818 = ORIENTED_EDGE ( 'NONE', *, *, #4482, .T. ) ;
#13819 = VERTEX_POINT ( 'NONE', #2372 ) ;
#13820 = ADVANCED_FACE ( 'NONE', ( #7131 ), #21944, .T. ) ;
#13821 = LINE ( 'NONE', #4509, #4653 ) ;
#13822 = DIRECTION ( 'NONE',  ( -1.000000000000000000, -3.053848253006669023E-16, 2.042510438544995415E-16 ) ) ;
#13823 = CARTESIAN_POINT ( 'NONE',  ( 57.03253626007334987, -0.8141194241917997232, -2.469252834999610791 ) ) ;
#13824 = ORIENTED_EDGE ( 'NONE', *, *, #19889, .F. ) ;
#13825 = CYLINDRICAL_SURFACE ( 'NONE', #298, 3.399999999999999911 ) ;
#13826 = CARTESIAN_POINT ( 'NONE',  ( -55.03335481156724995, 0.7533615035078067290, -3.673546848079180194 ) ) ;
#13827 = CARTESIAN_POINT ( 'NONE',  ( 69.25000000000004263, 3.819818661513594083E-16, 2.729289321880612906 ) ) ;
#13828 = CARTESIAN_POINT ( 'NONE',  ( -35.85663232820584057, 5.086913985776147840, -1.171642053949061513 ) ) ;
#13830 = CARTESIAN_POINT ( 'NONE',  ( 58.66133336607585136, -1.819551968140056264, -0.4538287010057830972 ) ) ;
#13829 = CARTESIAN_POINT ( 'NONE',  ( -36.39645873810207632, -2.743848709681594222, 4.666930520580660158 ) ) ;
#13831 = VECTOR ( 'NONE', #17743, 1000.000000000000000 ) ;
#13832 = EDGE_CURVE ( 'NONE', #826, #1451, #4946, .T. ) ;
#13833 = CARTESIAN_POINT ( 'NONE',  ( 15.03925126672132784, 4.817150320980643663, 2.203324261490556157 ) ) ;
#13834 = CARTESIAN_POINT ( 'NONE',  ( 61.24012582333646293, -0.9011229182321967013, -1.742583661751029300 ) ) ;
#13835 = DIRECTION ( 'NONE',  ( 1.000000000000000000, 3.054025858079668409E-16, -2.042474015755241579E-16 ) ) ;
#13836 = ORIENTED_EDGE ( 'NONE', *, *, #24181, .T. ) ;
#13837 = CONICAL_SURFACE ( 'NONE', #5777, 2.150000000000000355, 0.03277514440407566787 ) ;
#13838 = ORIENTED_EDGE ( 'NONE', *, *, #27210, .F. ) ;
#13839 = EDGE_CURVE ( 'NONE', #30026, #6950, #24952, .T. ) ;
#13840 = DIRECTION ( 'NONE',  ( 0.000000000000000000, 0.000000000000000000, 1.000000000000000000 ) ) ;
#13841 =( BOUNDED_CURVE ( )  B_SPLINE_CURVE ( 3, ( #5283, #88, #19729, #12122 ),
 .UNSPECIFIED., .F., .T. ) 
 B_SPLINE_CURVE_WITH_KNOTS ( ( 4, 4 ),
 ( -8.881784197001252323E-16, 1.570796326794897446 ),
 .UNSPECIFIED. ) 
 CURVE ( )  GEOMETRIC_REPRESENTATION_ITEM ( )  RATIONAL_B_SPLINE_CURVE ( ( 1.000000000000000000, 0.8047378541243646044, 0.8047378541243646044, 1.000000000000000000 ) ) 
 REPRESENTATION_ITEM ( '' )  );
#13842 = ORIENTED_EDGE ( 'NONE', *, *, #23966, .T. ) ;
#13843 = ADVANCED_FACE ( 'NONE', ( #15657 ), #1282, .T. ) ;
#13844 = CARTESIAN_POINT ( 'NONE',  ( 52.11520194349620283, 3.840337079369375406, 2.049999999999818190 ) ) ;
#13845 = CARTESIAN_POINT ( 'NONE',  ( -57.90835481156723574, 4.108500314926515351, -1.367561758111407899 ) ) ;
#13847 = CARTESIAN_POINT ( 'NONE',  ( 50.80000000000001847, -4.031600731908414836, -1.173113608511851647 ) ) ;
#13846 = DIRECTION ( 'NONE',  ( 0.000000000000000000, -1.000000000000000000, 0.000000000000000000 ) ) ;
#13848 = EDGE_CURVE ( 'NONE', #28571, #7964, #21157, .T. ) ;
#13849 = ORIENTED_EDGE ( 'NONE', *, *, #1766, .F. ) ;
#13850 = CARTESIAN_POINT ( 'NONE',  ( -74.39999999999997726, -2.588216748940040213E-15, 4.710014593512140639E-15 ) ) ;
#13851 = ORIENTED_EDGE ( 'NONE', *, *, #1402, .F. ) ;
#13852 = AXIS2_PLACEMENT_3D ( 'NONE', #18654, #3919, #11523 ) ;
#13853 = DIRECTION ( 'NONE',  ( -1.000000000000000000, -1.047444401652940007E-14, -0.000000000000000000 ) ) ;
#13854 = ORIENTED_EDGE ( 'NONE', *, *, #23992, .T. ) ;
#13856 = DIRECTION ( 'NONE',  ( -1.000000000000000000, -2.586136946169074517E-16, 0.000000000000000000 ) ) ;
#13855 = CARTESIAN_POINT ( 'NONE',  ( 50.50000002815836098, 0.7900353715961344614, 4.025797886239747214 ) ) ;
#13857 = ORIENTED_EDGE ( 'NONE', *, *, #2046, .F. ) ;
#13858 = AXIS2_PLACEMENT_3D ( 'NONE', #7254, #28643, #17236 ) ;
#13859 = CARTESIAN_POINT ( 'NONE',  ( 57.00000000000002132, -0.6820512820512792951, 1.773360101234991770 ) ) ;
#13860 = CARTESIAN_POINT ( 'NONE',  ( 58.65844932252363009, 1.819473848874897159, -0.4532319986943835199 ) ) ;
#13861 = CARTESIAN_POINT ( 'NONE',  ( 47.44023805160308882, -4.327157167232345003, 1.563052875988448776 ) ) ;
#13862 = DIRECTION ( 'NONE',  ( -1.000000000000000000, -3.053848253006669023E-16, 2.042510438544995415E-16 ) ) ;
#13863 = CARTESIAN_POINT ( 'NONE',  ( -59.38452994616203995, 3.117691453623979481, 1.799999999999801092 ) ) ;
#13864 = CARTESIAN_POINT ( 'NONE',  ( 69.25000000000001421, 4.557543281186736018E-17, -7.253552481446610839E-13 ) ) ;
#13865 = CARTESIAN_POINT ( 'NONE',  ( -62.09999999999997300, -2.524216908331983422, -0.06288083723137104231 ) ) ;
#13866 = CARTESIAN_POINT ( 'NONE',  ( -56.47085481156723574, 2.489203624310592389, -2.804704140674919355 ) ) ;
#13867 = EDGE_CURVE ( 'NONE', #30656, #16179, #25453, .T. ) ;
#13868 = CIRCLE ( 'NONE', #30067, 0.2500000000000000000 ) ;
#13869 = CARTESIAN_POINT ( 'NONE',  ( -55.92292740578360366, 2.256877952708273405, -2.542931754211921636 ) ) ;
#13871 = EDGE_CURVE ( 'NONE', #5904, #12772, #28654, .T. ) ;
#13870 = CARTESIAN_POINT ( 'NONE',  ( -55.64405989232412253, 2.944486372867106905, -1.700000000000184253 ) ) ;
#13872 = CIRCLE ( 'NONE', #17954, 0.05000000000000005829 ) ;
#13873 = VERTEX_POINT ( 'NONE', #25608 ) ;
#13874 = CYLINDRICAL_SURFACE ( 'NONE', #21088, 2.874999999999999112 ) ;
#13875 = CARTESIAN_POINT ( 'NONE',  ( 44.98443556292537693, -3.726179070414207928, 1.000000000000002220 ) ) ;
#13876 = B_SPLINE_CURVE_WITH_KNOTS ( 'NONE', 3,
 ( #15378, #3045, #5420, #15075, #2590, #12688, #27100, #12236, #19695, #361, #10168, #24568, #199, #10030, #29330, #22368, #19837, #29467, #14763, #658 ),
 .UNSPECIFIED., .F., .F.,
 ( 4, 2, 2, 2, 2, 2, 2, 2, 2, 4 ),
 ( -9.867963739368879538E-05, 0.0004287238591677978820, 0.0009561273557292845459, 0.001483530852290771643, 0.002010934348852258524, 0.002538337845413745405, 0.003065741341975232719, 0.003329443090255982448, 0.003593144838536732177, 0.004120548335098232068 ),
 .UNSPECIFIED. ) ;
#13877 = CARTESIAN_POINT ( 'NONE',  ( -36.42771574642760868, 0.4841707035673717407, 5.391286593723181753 ) ) ;
#13878 = DIRECTION ( 'NONE',  ( 1.000000000000000000, 1.047444401652940007E-14, 0.000000000000000000 ) ) ;
#13879 = ORIENTED_EDGE ( 'NONE', *, *, #29608, .T. ) ;
#13880 = CARTESIAN_POINT ( 'NONE',  ( 58.73379417893120547, 1.662624490947003153, 0.8670685180651535040 ) ) ;
#13881 = EDGE_LOOP ( 'NONE', ( #27793, #8582, #5006, #17659 ) ) ;
#13882 = CIRCLE ( 'NONE', #4295, 1.375000000000001332 ) ;
#13883 = CARTESIAN_POINT ( 'NONE',  ( -54.49999999999997868, -6.102218906431378987E-14, -2.216533082070118739E-13 ) ) ;
#13885 = DIRECTION ( 'NONE',  ( 1.000000000000000000, 0.000000000000000000, 0.000000000000000000 ) ) ;
#13884 = CARTESIAN_POINT ( 'NONE',  ( 51.90000000000001279, -4.131056160354152240, 1.099999999999999867 ) ) ;
#13886 = B_SPLINE_SURFACE_WITH_KNOTS ( 'NONE', 3, 1, ( 
 ( #9995, #18910 ),
 ( #28554, #6865 ),
 ( #16533, #21448 ),
 ( #20287, #10754 ),
 ( #15347, #22957 ),
 ( #18060, #20753 ),
 ( #15678, #3322 ),
 ( #6174, #29763 ),
 ( #8683, #18363 ),
 ( #8080, #959 ),
 ( #13417, #12805 ),
 ( #20436, #17745 ),
 ( #28001, #1411 ),
 ( #27387, #30230 ),
 ( #8538, #8376 ) ),
 .UNSPECIFIED., .F., .F., .F.,
 ( 4, 1, 1, 1, 1, 1, 1, 1, 1, 1, 1, 1, 4 ),
 ( 2, 2 ),
 ( 0.03200690811995968860, 0.06212998257909596589, 0.1242599651581919318, 0.2485199303163838636, 0.3727798954745757953, 0.4970398606327676716, 0.6212998257909596589, 0.6834298083700556248, 0.7455597909491514796, 0.8076897735282474455, 0.8387547648177954285, 0.8698197561073434114, 0.8953196945511240346 ),
 ( 0.000000000000000000, 1.000000000000000000 ),
 .UNSPECIFIED. ) ;
#13887 = EDGE_CURVE ( 'NONE', #17048, #3273, #13952, .T. ) ;
#13888 = ORIENTED_EDGE ( 'NONE', *, *, #2095, .T. ) ;
#13889 = EDGE_LOOP ( 'NONE', ( #15518, #27148, #5894, #18148 ) ) ;
#13890 = CYLINDRICAL_SURFACE ( 'NONE', #4766, 0.1499999999999999667 ) ;
#13891 = LINE ( 'NONE', #28805, #12020 ) ;
#13893 = CARTESIAN_POINT ( 'NONE',  ( 60.99999276535461945, 0.5623636236612823414, -1.858165151419263639 ) ) ;
#13892 = CARTESIAN_POINT ( 'NONE',  ( 51.70000000000002416, 6.982261990806648555E-14, -1.793082891011605378E-13 ) ) ;
#13894 = VERTEX_POINT ( 'NONE', #1393 ) ;
#13895 = CARTESIAN_POINT ( 'NONE',  ( -55.37499999999997868, 2.489203624310591056, -2.804704140674918023 ) ) ;
#13896 = CIRCLE ( 'NONE', #264, 160.5997717543497743 ) ;
#13897 = CARTESIAN_POINT ( 'NONE',  ( 51.80000000000001137, 6.475000000000062705, -2.050000000000180123 ) ) ;
#13898 = PRODUCT_CONTEXT ( 'NONE', #26924, 'mechanical' ) ;
#13899 = AXIS2_PLACEMENT_3D ( 'NONE', #21917, #2883, #26942 ) ;
#13900 = CARTESIAN_POINT ( 'NONE',  ( -61.37134253426428643, -2.620685193807273272, -0.6125669275117787693 ) ) ;
#13901 = DIRECTION ( 'NONE',  ( 1.000000000000000000, 3.053848253006669023E-16, -2.042510438544995415E-16 ) ) ;
#13902 = CARTESIAN_POINT ( 'NONE',  ( 51.23644008536124517, -1.080112125195908046, 1.214076932077873039 ) ) ;
#13903 = ORIENTED_EDGE ( 'NONE', *, *, #30850, .T. ) ;
#13904 = CIRCLE ( 'NONE', #4309, 4.099999999999992539 ) ;
#13905 = DIRECTION ( 'NONE',  ( -1.000000000000000000, -1.047444401652940007E-14, -0.000000000000000000 ) ) ;
#13906 = AXIS2_PLACEMENT_3D ( 'NONE', #10296, #27241, #26923 ) ;
#13907 = CARTESIAN_POINT ( 'NONE',  ( -36.21152527658243514, 2.821511581828426429, -4.377605326016285936 ) ) ;
#13908 = CARTESIAN_POINT ( 'NONE',  ( 58.65000000000003411, -1.671477153793625714, -0.8495817349401489915 ) ) ;
#13909 = CARTESIAN_POINT ( 'NONE',  ( 41.48619405471883681, -151.3359592902622239, -1.950000000000163380 ) ) ;
#13910 = EDGE_CURVE ( 'NONE', #4338, #22781, #12443, .T. ) ;
#13911 = EDGE_CURVE ( 'NONE', #17696, #5594, #1826, .T. ) ;
#13912 = CARTESIAN_POINT ( 'NONE',  ( 57.03008957414009217, -0.7461961634598838211, -2.423767181580114727 ) ) ;
#13915 = EDGE_CURVE ( 'NONE', #10186, #3598, #15802, .T. ) ;
#13914 = CARTESIAN_POINT ( 'NONE',  ( 58.75000000000004263, -1.877732920580616804, -0.6121634413826785304 ) ) ;
#13913 = CARTESIAN_POINT ( 'NONE',  ( 56.95000000000001705, -0.6820512820512819596, -1.773360101234998210 ) ) ;
#13916 = AXIS2_PLACEMENT_3D ( 'NONE', #30349, #27673, #28299 ) ;
#13917 = CARTESIAN_POINT ( 'NONE',  ( 47.10000001624534605, -4.079529477378120994, -2.128865254697307474 ) ) ;
#13919 = DIRECTION ( 'NONE',  ( 0.000000000000000000, 1.224646799147353207E-16, 1.000000000000000000 ) ) ;
#13918 = LINE ( 'NONE', #21091, #10465 ) ;
#13920 = AXIS2_PLACEMENT_3D ( 'NONE', #25959, #20910, #30877 ) ;
#13921 = EDGE_LOOP ( 'NONE', ( #12198, #4894, #9757, #23347 ) ) ;
#13922 = CARTESIAN_POINT ( 'NONE',  ( -59.19999999999996732, -2.580747833305891970, -0.9498634748674686934 ) ) ;
#13923 = CARTESIAN_POINT ( 'NONE',  ( 58.75000000000002132, 6.153735859711025284E-13, 3.111507638930570854E-58 ) ) ;
#13925 = CARTESIAN_POINT ( 'NONE',  ( 57.00000000000001421, 0.000000000000000000, 2.549999999999999822 ) ) ;
#13924 = CARTESIAN_POINT ( 'NONE',  ( 58.66118217212512320, 1.815481606355567878, 0.4689659288418223104 ) ) ;
#13926 = CARTESIAN_POINT ( 'NONE',  ( 15.29384114148389884, -5.068511731019460065, 1.228278365482025070 ) ) ;
#13927 = CIRCLE ( 'NONE', #1303, 0.05000000000000008604 ) ;
#13928 = ORIENTED_EDGE ( 'NONE', *, *, #2681, .F. ) ;
#13929 = VERTEX_POINT ( 'NONE', #13865 ) ;
#13930 = CARTESIAN_POINT ( 'NONE',  ( -36.27260443516959754, -4.885888067249525513, 1.790336215468749215 ) ) ;
#13931 = LINE ( 'NONE', #9214, #9306 ) ;
#13932 = CIRCLE ( 'NONE', #8384, 2.625000000000000444 ) ;
#13933 = ADVANCED_FACE ( 'NONE', ( #23256 ), #1542, .F. ) ;
#13934 = ORIENTED_EDGE ( 'NONE', *, *, #6790, .T. ) ;
#13935 = VECTOR ( 'NONE', #28875, 1000.000000000000000 ) ;
#13936 = CARTESIAN_POINT ( 'NONE',  ( 51.80000000000002558, 3.987920669275808905, 2.032050446608677507 ) ) ;
#13937 = EDGE_LOOP ( 'NONE', ( #13814, #9580, #6399, #17210 ) ) ;
#13938 = DIRECTION ( 'NONE',  ( 0.000000000000000000, 0.000000000000000000, -1.000000000000000000 ) ) ;
#13939 = ORIENTED_EDGE ( 'NONE', *, *, #26246, .T. ) ;
#13940 = CONICAL_SURFACE ( 'NONE', #8389, 4.299999999999998934, 0.7853981633974466137 ) ;
#13941 = CARTESIAN_POINT ( 'NONE',  ( -60.26905989232410121, 2.023778652682511261E-14, -3.400000000000213518 ) ) ;
#13942 = ORIENTED_EDGE ( 'NONE', *, *, #11013, .F. ) ;
#13943 = ORIENTED_EDGE ( 'NONE', *, *, #2823, .T. ) ;
#13944 = AXIS2_PLACEMENT_3D ( 'NONE', #1056, #578, #5973 ) ;
#13945 = EDGE_LOOP ( 'NONE', ( #8371, #24737, #17010, #7798 ) ) ;
#13946 = CARTESIAN_POINT ( 'NONE',  ( -56.07202994616204705, -4.156921938165296204, -2.141547992439359634E-13 ) ) ;
#13947 = AXIS2_PLACEMENT_3D ( 'NONE', #7635, #24561, #4950 ) ;
#13948 = DIRECTION ( 'NONE',  ( -0.9993908270191123044, 0.03489949670202457249, 4.336808689942002748E-15 ) ) ;
#13949 = CARTESIAN_POINT ( 'NONE',  ( 54.50000000000002132, 1.734723475976807094E-15, 0.000000000000000000 ) ) ;
#13950 = CARTESIAN_POINT ( 'NONE',  ( -59.19495429951913223, -2.548385458854336871, -0.9469503383366065785 ) ) ;
#13951 = FACE_OUTER_BOUND ( 'NONE', #10221, .T. ) ;
#13952 = CIRCLE ( 'NONE', #16511, 0.05000000000000012768 ) ;
#13953 = ADVANCED_FACE ( 'NONE', ( #9156 ), #4394, .F. ) ;
#13954 = VECTOR ( 'NONE', #23477, 1000.000000000000227 ) ;
#13955 = VECTOR ( 'NONE', #12239, 999.9999999999998863 ) ;
#13957 = DIRECTION ( 'NONE',  ( 1.000000000000000000, 0.000000000000000000, 0.000000000000000000 ) ) ;
#13956 = SURFACE_SIDE_STYLE ('',( #30432 ) ) ;
#13958 = CARTESIAN_POINT ( 'NONE',  ( 69.25000000000000000, 0.7500000000000000000, -2.288246715074081283 ) ) ;
#13959 = FACE_OUTER_BOUND ( 'NONE', #24293, .T. ) ;
#13960 = CARTESIAN_POINT ( 'NONE',  ( -35.85663232820584057, -2.199885893005943949, -4.939696249117691451 ) ) ;
#13961 = CARTESIAN_POINT ( 'NONE',  ( 58.75000018803720536, -1.651902078983118916, -1.010830333486722798 ) ) ;
#13962 = CARTESIAN_POINT ( 'NONE',  ( 57.05000000000002558, 0.7500000000000000000, -2.490438859776669123 ) ) ;
#13963 = CARTESIAN_POINT ( 'NONE',  ( 60.75000000000002842, -0.4999999999993638977, 1.863080903344643380 ) ) ;
#13964 = ORIENTED_EDGE ( 'NONE', *, *, #23542, .T. ) ;
#13966 = CARTESIAN_POINT ( 'NONE',  ( 50.31877865969203611, -1.391940262980897236, 3.850000000000022293 ) ) ;
#13965 = CARTESIAN_POINT ( 'NONE',  ( 51.08379317338048509, -0.8723108729827115937, -1.374656996893404148 ) ) ;
#13967 = CIRCLE ( 'NONE', #3881, 4.600000000000000533 ) ;
#13968 = CARTESIAN_POINT ( 'NONE',  ( -61.34999999999997300, -2.609922480197373940, 0.4591346723570145505 ) ) ;
#13969 = AXIS2_PLACEMENT_3D ( 'NONE', #10639, #29947, #19986 ) ;
#13970 = EDGE_CURVE ( 'NONE', #15300, #23886, #10174, .T. ) ;
#13971 = AXIS2_PLACEMENT_3D ( 'NONE', #12958, #22327, #5842 ) ;
#13972 = VERTEX_POINT ( 'NONE', #4227 ) ;
#13973 = LINE ( 'NONE', #4321, #18451 ) ;
#13974 = DIRECTION ( 'NONE',  ( 1.040834085586084257E-14, 0.000000000000000000, 1.000000000000000000 ) ) ;
#13975 = CARTESIAN_POINT ( 'NONE',  ( -54.69702994616206837, -2.078460969082657872, 3.599999999999797584 ) ) ;
#13977 = VERTEX_POINT ( 'NONE', #23559 ) ;
#13976 = B_SPLINE_CURVE_WITH_KNOTS ( 'NONE', 3,
 ( #12045, #7445, #21719, #9676, #28972, #7279, #26594, #4904, #14569, #24232, #2543, #21872, #10271, #30043, #3760, #5839, #27217, #15496 ),
 .UNSPECIFIED., .F., .F.,
 ( 4, 2, 2, 2, 2, 1, 1, 2, 2, 4 ),
 ( 0.000000000000000000, 0.1171184220236923118, 0.2342368440473846236, 0.2488766468003461019, 0.2525365974885872000, 0.2561965481768282982, 0.2635164495533074969, 0.2927960550592145217, 0.3513552660710277942, 0.4684736880946559490 ),
 .UNSPECIFIED. ) ;
#13978 = TOROIDAL_SURFACE ( 'NONE', #8918, 3.020710678118645909, 0.05000000000000000278 ) ;
#13979 = EDGE_LOOP ( 'NONE', ( #25756, #24002 ) ) ;
#13980 = CARTESIAN_POINT ( 'NONE',  ( 16.10705563471229596, 5.191204783933242695, 1.522159526382794059 ) ) ;
#13981 = ORIENTED_EDGE ( 'NONE', *, *, #7094, .T. ) ;
#13982 = AXIS2_PLACEMENT_3D ( 'NONE', #9196, #16466, #1577 ) ;
#13983 = CARTESIAN_POINT ( 'NONE',  ( 58.72204580543428420, -1.612507782425395719, 0.9570475208902531339 ) ) ;
#13984 = EDGE_LOOP ( 'NONE', ( #27541, #8142 ) ) ;
#13985 = SPHERICAL_SURFACE ( 'NONE', #28230, 0.05000000000000000278 ) ;
#13986 = CIRCLE ( 'NONE', #21597, 0.1500000000000001887 ) ;
#13987 = VECTOR ( 'NONE', #27595, 1000.000000000000114 ) ;
#13988 = DIRECTION ( 'NONE',  ( -1.000000000000000000, -0.000000000000000000, 1.047444401652940007E-14 ) ) ;
#13989 = DIRECTION ( 'NONE',  ( 1.000000000000000000, 0.000000000000000000, 0.000000000000000000 ) ) ;
#13990 = EDGE_LOOP ( 'NONE', ( #6061, #18404, #18878, #1448 ) ) ;
#13991 = ORIENTED_EDGE ( 'NONE', *, *, #1897, .T. ) ;
#13992 = CARTESIAN_POINT ( 'NONE',  ( 52.06628335902946247, -0.5434431642975682264, -1.794517909405659806 ) ) ;
#13993 = CARTESIAN_POINT ( 'NONE',  ( -44.59999999999997300, -4.766731106216475591E-14, -1.489237264809750408E-13 ) ) ;
#13994 = DIRECTION ( 'NONE',  ( 0.000000000000000000, 0.000000000000000000, 1.000000000000000000 ) ) ;
#13995 = VERTEX_POINT ( 'NONE', #11054 ) ;
#13996 = TOROIDAL_SURFACE ( 'NONE', #12481, 4.800000000000000711, 0.05000000000000000278 ) ;
#13997 = FACE_OUTER_BOUND ( 'NONE', #13192, .T. ) ;
#13998 = CARTESIAN_POINT ( 'NONE',  ( 58.66054497608050866, 0.5000000000006143974, -1.807104036850122109 ) ) ;
#13999 = AXIS2_PLACEMENT_3D ( 'NONE', #18326, #13232, #1066 ) ;
#14000 = ADVANCED_FACE ( 'NONE', ( #28462 ), #18346, .T. ) ;
#14001 = DIRECTION ( 'NONE',  ( 0.000000000000000000, 0.000000000000000000, -1.000000000000000000 ) ) ;
#14002 = AXIS2_PLACEMENT_3D ( 'NONE', #21410, #23305, #21100 ) ;
#14003 = CARTESIAN_POINT ( 'NONE',  ( 58.65000000000001990, -0.5811678240974686993, 1.782657835994643891 ) ) ;
#14005 = DIRECTION ( 'NONE',  ( 0.000000000000000000, 0.000000000000000000, -1.000000000000000000 ) ) ;
#14004 =( NAMED_UNIT ( * ) PLANE_ANGLE_UNIT ( ) SI_UNIT ( $, .RADIAN. ) );
#14006 = DIRECTION ( 'NONE',  ( 0.000000000000000000, -0.2008964009354147484, 0.9796124928211140670 ) ) ;
#14007 = CARTESIAN_POINT ( 'NONE',  ( 46.90000000000001279, -4.227689052994015206, 1.125730994152046582 ) ) ;
#14008 = AXIS2_PLACEMENT_3D ( 'NONE', #14837, #24498, #12021 ) ;
#14009 = DIRECTION ( 'NONE',  ( -0.7313537016191670181, -0.6819983600625022513, 2.468850131082252327E-15 ) ) ;
#14010 = VECTOR ( 'NONE', #30394, 1000.000000000000000 ) ;
#14011 = ORIENTED_EDGE ( 'NONE', *, *, #7552, .F. ) ;
#14012 = EDGE_CURVE ( 'NONE', #23000, #16551, #16978, .T. ) ;
#14013 = CARTESIAN_POINT ( 'NONE',  ( -44.49999999999999289, 1.499999999999999556, -4.029888335921975262 ) ) ;
#14014 = ORIENTED_EDGE ( 'NONE', *, *, #2235, .F. ) ;
#14015 = CARTESIAN_POINT ( 'NONE',  ( 52.38400031671234558, 8.538946093000230775, 1.943109374214545770 ) ) ;
#14016 = CARTESIAN_POINT ( 'NONE',  ( -57.97085481156723574, 2.489203624310592389, -2.804704140674918911 ) ) ;
#14018 = CARTESIAN_POINT ( 'NONE',  ( 50.93220014711046417, -4.031600731540152083, -1.173113608404695585 ) ) ;
#14017 = DIRECTION ( 'NONE',  ( 3.491481338843133355E-15, 0.000000000000000000, 1.000000000000000000 ) ) ;
#14019 = ORIENTED_EDGE ( 'NONE', *, *, #9701, .F. ) ;
#14020 = VERTEX_POINT ( 'NONE', #30989 ) ;
#14021 = FACE_OUTER_BOUND ( 'NONE', #29472, .T. ) ;
#14022 = AXIS2_PLACEMENT_3D ( 'NONE', #19419, #15118, #2627 ) ;
#14023 = ORIENTED_EDGE ( 'NONE', *, *, #211, .F. ) ;
#14024 = CARTESIAN_POINT ( 'NONE',  ( -37.18272003341174781, -1.653865106024005792E-14, 0.000000000000000000 ) ) ;
#14025 = AXIS2_PLACEMENT_3D ( 'NONE', #30990, #30678, #11834 ) ;
#14026 = VERTEX_POINT ( 'NONE', #6153 ) ;
#14028 = DIRECTION ( 'NONE',  ( 0.000000000000000000, 0.9507508458638780358, -0.3099561728520990322 ) ) ;
#14027 = CARTESIAN_POINT ( 'NONE',  ( 50.33305158408655444, 1.365427245289844826, 3.854926352964885172 ) ) ;
#14029 = ORIENTED_EDGE ( 'NONE', *, *, #12223, .T. ) ;
#14030 = B_SPLINE_CURVE_WITH_KNOTS ( 'NONE', 3,
 ( #28894, #4983, #14635, #26507, #9886, #4814 ),
 .UNSPECIFIED., .F., .F.,
 ( 4, 2, 4 ),
 ( 2.185279341460844539E-19, 0.0001531825249253924851, 0.0003063650498507847534 ),
 .UNSPECIFIED. ) ;
#14031 = CARTESIAN_POINT ( 'NONE',  ( 53.32365433735401439, 7.956691627322815208, 1.890490914785547094 ) ) ;
#14032 = EDGE_CURVE ( 'NONE', #15811, #6214, #106, .T. ) ;
#14033 = CARTESIAN_POINT ( 'NONE',  ( 58.66122797211873063, 1.815363284468485716, -0.4694237433637749590 ) ) ;
#14034 = AXIS2_PLACEMENT_3D ( 'NONE', #7686, #9762, #2633 ) ;
#14035 = CARTESIAN_POINT ( 'NONE',  ( -54.48167032960165557, -1.510995100284905579, -3.307167554963765799 ) ) ;
#14036 = CARTESIAN_POINT ( 'NONE',  ( 36.55000000000001847, 2.326828918379971365E-16, 1.899999999999999911 ) ) ;
#14037 = CARTESIAN_POINT ( 'NONE',  ( -57.19702994616204705, 4.156921938165313080, -1.880369327726949834E-13 ) ) ;
#14038 = CARTESIAN_POINT ( 'NONE',  ( 51.89158610412761874, -1.677904505874998473E-13, 4.375000000000013323 ) ) ;
#14039 = EDGE_CURVE ( 'NONE', #24537, #1564, #21508, .T. ) ;
#14040 = DIRECTION ( 'NONE',  ( 1.000000000000000000, 1.047444401652940007E-14, 0.000000000000000000 ) ) ;
#14041 = EDGE_CURVE ( 'NONE', #31086, #1993, #19579, .T. ) ;
#14042 = DIRECTION ( 'NONE',  ( 0.000000000000000000, 0.000000000000000000, -1.000000000000000000 ) ) ;
#14043 = AXIS2_PLACEMENT_3D ( 'NONE', #29819, #15253, #13318 ) ;
#14044 = EDGE_CURVE ( 'NONE', #10580, #9917, #25604, .T. ) ;
#14045 = VECTOR ( 'NONE', #26714, 1000.000000000000000 ) ;
#14046 = CARTESIAN_POINT ( 'NONE',  ( -57.42292740578360366, 2.256877952708274737, -2.542931754211919859 ) ) ;
#14047 =( BOUNDED_CURVE ( )  B_SPLINE_CURVE ( 3, ( #27894, #13773, #1140, #1285 ),
 .UNSPECIFIED., .F., .T. ) 
 B_SPLINE_CURVE_WITH_KNOTS ( ( 4, 4 ),
 ( 3.141592653589793116, 4.712388980384689674 ),
 .UNSPECIFIED. ) 
 CURVE ( )  GEOMETRIC_REPRESENTATION_ITEM ( )  RATIONAL_B_SPLINE_CURVE ( ( 1.000000000000000000, 0.8047378541243649375, 0.8047378541243649375, 1.000000000000000000 ) ) 
 REPRESENTATION_ITEM ( '' )  );
#14048 = AXIS2_PLACEMENT_3D ( 'NONE', #15377, #22367, #27099 ) ;
#14049 = LINE ( 'NONE', #11686, #22047 ) ;
#14050 = ORIENTED_EDGE ( 'NONE', *, *, #14078, .T. ) ;
#14051 = CARTESIAN_POINT ( 'NONE',  ( -44.49999999999997868, -3.524999999999988365, -1.993951146718866384E-13 ) ) ;
#14052 = B_SPLINE_CURVE_WITH_KNOTS ( 'NONE', 3,
 ( #3878, #30464, #18460, #13823, #13529, #4344, #20989, #9270, #16386, #28422, #28575, #6887, #30624, #8936, #18775, #28097 ),
 .UNSPECIFIED., .F., .F.,
 ( 4, 3, 3, 3, 3, 4 ),
 ( 0.000000000000000000, 1.754151282668922588E-05, 5.222880005687533889E-05, 8.869434694929045231E-05, 0.0001259176481356621589, 0.0001632567749836554797 ),
 .UNSPECIFIED. ) ;
#14053 = CARTESIAN_POINT ( 'NONE',  ( -36.80043232705879319, 0.5375162698823430230, 5.381098085087389293 ) ) ;
#14054 = DIRECTION ( 'NONE',  ( 1.000000000000000000, 2.586136946169074517E-16, -0.000000000000000000 ) ) ;
#14055 = VERTEX_POINT ( 'NONE', #12286 ) ;
#14056 = ADVANCED_FACE ( 'NONE', ( #21680 ), #29652, .T. ) ;
#14057 = CARTESIAN_POINT ( 'NONE',  ( 58.45000000000001705, -0.8000000000000000444, 2.421260002560649660 ) ) ;
#14058 = ORIENTED_EDGE ( 'NONE', *, *, #3009, .F. ) ;
#14059 = CARTESIAN_POINT ( 'NONE',  ( 51.25000000000002842, -0.7499999999994634292, -1.718465885608440269 ) ) ;
#14061 = LINE ( 'NONE', #14216, #12619 ) ;
#14060 = CARTESIAN_POINT ( 'NONE',  ( 58.65000000000000568, 1.022750809562428476, -1.571497941946047083 ) ) ;
#14062 = EDGE_LOOP ( 'NONE', ( #28452, #18594, #30750, #28951 ) ) ;
#14063 = ORIENTED_EDGE ( 'NONE', *, *, #16676, .F. ) ;
#14064 = CARTESIAN_POINT ( 'NONE',  ( -59.09665968485343512, -2.466443774698472424, -0.9691001528487745986 ) ) ;
#14065 = DIRECTION ( 'NONE',  ( 0.03489949670250097613, 0.9993908270190957621, 0.000000000000000000 ) ) ;
#14067 = CARTESIAN_POINT ( 'NONE',  ( 58.74154451056417514, 0.8556855217786469847, 1.668374833163776882 ) ) ;
#14066 = DIRECTION ( 'NONE',  ( -1.000000000000000000, 0.000000000000000000, 0.000000000000000000 ) ) ;
#14068 = VERTEX_POINT ( 'NONE', #9638 ) ;
#14069 = CARTESIAN_POINT ( 'NONE',  ( -56.99999999999997158, -1.184343223768585807, -3.558065644182723641 ) ) ;
#14070 = CARTESIAN_POINT ( 'NONE',  ( 46.90000000000001279, -4.227689052994015206, -1.125730994152046804 ) ) ;
#14071 = ADVANCED_FACE ( 'NONE', ( #16903 ), #19558, .T. ) ;
#14072 = VECTOR ( 'NONE', #18715, 1000.000000000000000 ) ;
#14073 = CARTESIAN_POINT ( 'NONE',  ( -55.58155989232413674, 3.400000000000007461, -1.857527951337884861E-13 ) ) ;
#14074 = CONTEXT_DEPENDENT_SHAPE_REPRESENTATION ( #20933, #22975 ) ;
#14075 = CIRCLE ( 'NONE', #25192, 0.05000000000000014155 ) ;
#14076 = DIRECTION ( 'NONE',  ( 1.000000000000000000, 0.000000000000000000, 0.000000000000000000 ) ) ;
#14077 = FACE_OUTER_BOUND ( 'NONE', #3311, .T. ) ;
#14078 = EDGE_CURVE ( 'NONE', #21568, #203, #2787, .T. ) ;
#14079 = CARTESIAN_POINT ( 'NONE',  ( -62.06710100716626499, -2.637635658083895773, 0.1963493119579517165 ) ) ;
#14080 = ORIENTED_EDGE ( 'NONE', *, *, #11304, .F. ) ;
#14081 = CARTESIAN_POINT ( 'NONE',  ( -35.85663232820584767, 5.377732432866631385, -0.5657657256215208319 ) ) ;
#14082 = B_SPLINE_CURVE_WITH_KNOTS ( 'NONE', 3,
 ( #23205, #1493, #213, #29034, #12247, #9731, #70, #7045, #7651, #28735, #19392, #19246, #9875, #373 ),
 .UNSPECIFIED., .F., .F.,
 ( 4, 2, 2, 2, 2, 2, 4 ),
 ( 0.000000000000000000, 2.506106230924558877E-05, 5.012212461849117754E-05, 0.0001002442492369727192, 0.0002004884984739364396, 0.0004009769969478670787, 0.0008019539938957288448 ),
 .UNSPECIFIED. ) ;
#14083 = CARTESIAN_POINT ( 'NONE',  ( -35.85663232820592583, 3.426725943139576458, -3.937891353488712110 ) ) ;
#14084 = EDGE_CURVE ( 'NONE', #24615, #1696, #21090, .T. ) ;
#14085 = CARTESIAN_POINT ( 'NONE',  ( 48.43454905095371998, 1.397701019745849704, -3.854421226863028682 ) ) ;
#14086 = DIRECTION ( 'NONE',  ( 0.000000000000000000, 0.000000000000000000, 1.000000000000000000 ) ) ;
#14087 = ADVANCED_FACE ( 'NONE', ( #14677 ), #24336, .T. ) ;
#14088 = CARTESIAN_POINT ( 'NONE',  ( 57.02007310689670305, -0.7405013978967619481, -2.427462356522636533 ) ) ;
#14090 = CYLINDRICAL_SURFACE ( 'NONE', #29588, 0.1000000000000000472 ) ;
#14089 = DIRECTION ( 'NONE',  ( -1.000000000000000000, 0.000000000000000000, 1.047444401652940007E-14 ) ) ;
#14091 = DIRECTION ( 'NONE',  ( -1.000000000000000000, 0.000000000000000000, 3.491481338843133355E-15 ) ) ;
#14093 = DIRECTION ( 'NONE',  ( -1.000000000000000000, -3.385297212316258532E-16, 2.459562394685744279E-16 ) ) ;
#14092 = DIRECTION ( 'NONE',  ( 0.000000000000000000, 0.000000000000000000, 1.000000000000000000 ) ) ;
#14094 = ORIENTED_EDGE ( 'NONE', *, *, #9419, .T. ) ;
#14095 = AXIS2_PLACEMENT_3D ( 'NONE', #17116, #10436, #18046 ) ;
#14096 = CARTESIAN_POINT ( 'NONE',  ( -62.05964969381223284, -2.667838369614432548, -0.3597575050025147991 ) ) ;
#14097 = DIRECTION ( 'NONE',  ( 0.000000000000000000, -0.000000000000000000, 1.000000000000000000 ) ) ;
#14099 = CARTESIAN_POINT ( 'NONE',  ( -36.48821680285228553, 5.009497273852823618, 2.047744636826942521 ) ) ;
#14098 = DIRECTION ( 'NONE',  ( 1.000000000000000000, 3.125586771759065906E-16, 0.000000000000000000 ) ) ;
#14100 = CARTESIAN_POINT ( 'NONE',  ( 51.25000000000001421, 5.368159983410797313E-13, 3.111507638930570854E-58 ) ) ;
#14101 = ORIENTED_EDGE ( 'NONE', *, *, #23820, .T. ) ;
#14102 = ORIENTED_EDGE ( 'NONE', *, *, #16163, .T. ) ;
#14103 = DIRECTION ( 'NONE',  ( 0.000000000000000000, 0.000000000000000000, 1.000000000000000000 ) ) ;
#14104 = DIRECTION ( 'NONE',  ( 0.9913331294122580406, -0.1313720918981620966, 1.608844118403764524E-17 ) ) ;
#14105 = EDGE_LOOP ( 'NONE', ( #12333, #8791, #92, #19357 ) ) ;
#14106 = CYLINDRICAL_SURFACE ( 'NONE', #2784, 2.000000000000000000 ) ;
#14107 = B_SPLINE_CURVE_WITH_KNOTS ( 'NONE', 3,
 ( #3457, #20402, #22452, #8040, #27352, #10720, #10408, #1210, #8193, #8506, #13237, #25288, #18186, #30191, #17861, #27498, #3741, #3600, #27199 ),
 .UNSPECIFIED., .F., .F.,
 ( 4, 3, 3, 3, 3, 3, 4 ),
 ( 0.000000000000000000, 1.884866041445846106E-05, 3.951905945590748818E-05, 5.784447894079529801E-05, 7.452120580692728668E-05, 7.659178893127488138E-05, 9.043917046408786540E-05 ),
 .UNSPECIFIED. ) ;
#14108 = AXIS2_PLACEMENT_3D ( 'NONE', #23368, #4190, #14001 ) ;
#14109 = ORIENTED_EDGE ( 'NONE', *, *, #395, .T. ) ;
#14110 = EDGE_CURVE ( 'NONE', #30905, #16661, #27548, .T. ) ;
#14111 = CARTESIAN_POINT ( 'NONE',  ( 58.66122797211872353, 1.875002085570941057, 0.01642207461192947415 ) ) ;
#14112 = ORIENTED_EDGE ( 'NONE', *, *, #29660, .F. ) ;
#14113 = FILL_AREA_STYLE_COLOUR ( '', #16157 ) ;
#14114 = EDGE_CURVE ( 'NONE', #7683, #24892, #845, .T. ) ;
#14115 = CARTESIAN_POINT ( 'NONE',  ( -59.76905989232412253, -2.944486372867088697, 1.699999999999776579 ) ) ;
#14116 = EDGE_LOOP ( 'NONE', ( #9249, #31040, #16662, #25371 ) ) ;
#14117 =( NAMED_UNIT ( * ) SI_UNIT ( $, .STERADIAN. ) SOLID_ANGLE_UNIT ( ) );
#14118 = EDGE_CURVE ( 'NONE', #13124, #8009, #8659, .T. ) ;
#14119 = ORIENTED_EDGE ( 'NONE', *, *, #18901, .T. ) ;
#14120 = ORIENTED_EDGE ( 'NONE', *, *, #7894, .T. ) ;
#14121 = AXIS2_PLACEMENT_3D ( 'NONE', #15049, #5862, #13133 ) ;
#14122 = CIRCLE ( 'NONE', #26287, 0.1000000000000001860 ) ;
#14123 = CARTESIAN_POINT ( 'NONE',  ( -59.31249999999997868, -1.962990915244731793, 3.399999999999781419 ) ) ;
#14124 = DIRECTION ( 'NONE',  ( -1.054009200593503061E-14, 0.000000000000000000, -1.000000000000000000 ) ) ;
#14125 = DIRECTION ( 'NONE',  ( 1.000000000000000000, 0.000000000000000000, -1.047444401652940007E-14 ) ) ;
#14126 = LINE ( 'NONE', #14282, #26084 ) ;
#14127 = CARTESIAN_POINT ( 'NONE',  ( -35.85663232820584057, -2.686240680702151717, -4.475885388010727439 ) ) ;
#14128 = CARTESIAN_POINT ( 'NONE',  ( 51.75935175331192539, 4.143357532304555946, -1.955579579481696806 ) ) ;
#14129 = CARTESIAN_POINT ( 'NONE',  ( 48.40000000000001990, -1.391941090707485618, -3.850000000000022737 ) ) ;
#14130 = CARTESIAN_POINT ( 'NONE',  ( -61.34999999999997300, -2.399215024517336925, -0.7870147813924887048 ) ) ;
#14131 = CARTESIAN_POINT ( 'NONE',  ( -36.14504829323104929, -3.997758138077572632, -3.641634024966094341 ) ) ;
#14132 = ORIENTED_EDGE ( 'NONE', *, *, #21725, .F. ) ;
#14134 = AXIS2_PLACEMENT_3D ( 'NONE', #2264, #5225, #31079 ) ;
#14133 = DIRECTION ( 'NONE',  ( -1.000000000000000000, -3.054025858079668409E-16, 2.042474015755241579E-16 ) ) ;
#14135 = CARTESIAN_POINT ( 'NONE',  ( 53.96628743859024979, 7.375742867302039762, 2.049999999999812417 ) ) ;
#14136 = ORIENTED_EDGE ( 'NONE', *, *, #18412, .T. ) ;
#14138 = CARTESIAN_POINT ( 'NONE',  ( 50.37749466183669966, -1.328329461116575461, 3.879000873601222033 ) ) ;
#14137 = DIRECTION ( 'NONE',  ( -9.369508800225548439E-15, 0.8914544820235948963, -0.4531102586347439121 ) ) ;
#14139 = CARTESIAN_POINT ( 'NONE',  ( 54.25934562490486002, 5.649897281828979878, -2.026384253567227400 ) ) ;
#14140 = FACE_OUTER_BOUND ( 'NONE', #10528, .T. ) ;
#14141 = CARTESIAN_POINT ( 'NONE',  ( -55.99999999999997868, 3.673546848079180638, 0.7533615035078057298 ) ) ;
#14142 = AXIS2_PLACEMENT_3D ( 'NONE', #10901, #5848, #15674 ) ;
#14143 = AXIS2_PLACEMENT_3D ( 'NONE', #28707, #21590, #9558 ) ;
#14144 = ORIENTED_EDGE ( 'NONE', *, *, #7501, .T. ) ;
#14145 = CARTESIAN_POINT ( 'NONE',  ( 51.45655683570189609, 0.9591657938401634276, 1.468576096419530019 ) ) ;
#14146 = CARTESIAN_POINT ( 'NONE',  ( 58.65000000000000568, 1.571497941947157084, -1.022750809561052021 ) ) ;
#14147 = CARTESIAN_POINT ( 'NONE',  ( -60.06249999999997868, -1.962990915244731793, 3.399999999999778755 ) ) ;
#14148 = VERTEX_POINT ( 'NONE', #11833 ) ;
#14149 = ORIENTED_EDGE ( 'NONE', *, *, #6459, .F. ) ;
#14150 = CARTESIAN_POINT ( 'NONE',  ( 16.10624235918716352, 5.092377074781523127, 1.825725187625140133 ) ) ;
#14151 = ORIENTED_EDGE ( 'NONE', *, *, #4142, .T. ) ;
#14152 = AXIS2_PLACEMENT_3D ( 'NONE', #9585, #2600, #19550 ) ;
#14153 = ADVANCED_FACE ( 'NONE', ( #5018 ), #262, .F. ) ;
#14154 = CARTESIAN_POINT ( 'NONE',  ( 51.79856634703980944, 4.577364735441398658, 0.5261184863197011508 ) ) ;
#14155 = CARTESIAN_POINT ( 'NONE',  ( -57.94702994616203995, 4.156921938165313080, -1.906555437768272735E-13 ) ) ;
#14156 = ORIENTED_EDGE ( 'NONE', *, *, #20656, .T. ) ;
#14157 = DIRECTION ( 'NONE',  ( -2.117927888850090838E-16, 0.02490330187381123786, -0.9996898646859343485 ) ) ;
#14158 = EDGE_CURVE ( 'NONE', #247, #8353, #24592, .T. ) ;
#14159 = FACE_OUTER_BOUND ( 'NONE', #1224, .T. ) ;
#14160 = CARTESIAN_POINT ( 'NONE',  ( 28.70703846152719052, 5.747922418238211151, 1.949999999999901368 ) ) ;
#14161 = EDGE_LOOP ( 'NONE', ( #18284, #11061, #2437, #2777 ) ) ;
#14162 = ORIENTED_EDGE ( 'NONE', *, *, #30716, .T. ) ;
#14163 = FACE_OUTER_BOUND ( 'NONE', #24327, .T. ) ;
#14164 = DIRECTION ( 'NONE',  ( 0.000000000000000000, 0.9996898646859343485, 0.02490330187381123786 ) ) ;
#14165 = DIRECTION ( 'NONE',  ( 1.000000000000000000, -1.219044193948983948E-29, 3.491481338843133355E-15 ) ) ;
#14166 = VERTEX_POINT ( 'NONE', #20230 ) ;
#14167 = CARTESIAN_POINT ( 'NONE',  ( 48.40000000000001990, 1.409787217987196861, 3.950000000000022826 ) ) ;
#14168 = CARTESIAN_POINT ( 'NONE',  ( 56.95766603241608550, 0.7209790597604740503, 1.757928312873409116 ) ) ;
#14169 = ADVANCED_FACE ( 'NONE', ( #27642 ), #10086, .F. ) ;
#14171 = PLANE ( 'NONE',  #12864 ) ;
#14170 = FILL_AREA_STYLE ('',( #31108 ) ) ;
#14172 = B_SPLINE_SURFACE_WITH_KNOTS ( 'NONE', 3, 3, ( 
 ( #2940, #15431, #8005, #20043 ),
 ( #29686, #20369, #26990, #12584 ),
 ( #14802, #20213, #24780, #3089 ),
 ( #880, #19743, #17345, #12737 ),
 ( #22740, #27315, #10069, #5628 ),
 ( #24463, #5297, #2774, #705 ),
 ( #8155, #29373, #15278, #17826 ) ),
 .UNSPECIFIED., .F., .F., .F.,
 ( 4, 1, 1, 1, 4 ),
 ( 4, 4 ),
 ( 0.9434208788814886226, 0.9575656591611163559, 0.9717104394407443113, 0.9858552197203721557, 1.000000000000000000 ),
 ( 0.000000000000000000, 1.000000000000000000 ),
 .UNSPECIFIED. ) ;
#14173 = CARTESIAN_POINT ( 'NONE',  ( 58.74487987613210294, -0.4999999999991334154, 1.852860917433933219 ) ) ;
#14174 = CARTESIAN_POINT ( 'NONE',  ( -55.84599364905388086, 0.2309624077929090247, 3.875409454552789956 ) ) ;
#14175 = CARTESIAN_POINT ( 'NONE',  ( 41.48619405471883681, -151.3359592902621955, -2.050000000000163691 ) ) ;
#14176 = ORIENTED_EDGE ( 'NONE', *, *, #13044, .F. ) ;
#14177 = ORIENTED_EDGE ( 'NONE', *, *, #28931, .T. ) ;
#14178 = CARTESIAN_POINT ( 'NONE',  ( -59.13776767298602977, -2.346568386202238177, 1.245686009234607150 ) ) ;
#14179 = ORIENTED_EDGE ( 'NONE', *, *, #24512, .F. ) ;
#14180 = FACE_OUTER_BOUND ( 'NONE', #12542, .T. ) ;
#14181 = CARTESIAN_POINT ( 'NONE',  ( -54.42292740578361077, 2.256877952708269852, -2.542931754211926076 ) ) ;
#14183 = CARTESIAN_POINT ( 'NONE',  ( -36.30347965937239962, 3.148602930107292419, 4.139959549308673381 ) ) ;
#14182 = DIRECTION ( 'NONE',  ( 1.000000000000000000, 4.939082069373447378E-17, 1.520093157366847861E-16 ) ) ;
#14184 = ORIENTED_EDGE ( 'NONE', *, *, #26168, .T. ) ;
#14185 = DIRECTION ( 'NONE',  ( 1.000000000000000000, 0.000000000000000000, 0.000000000000000000 ) ) ;
#14186 = EDGE_LOOP ( 'NONE', ( #1362, #10313, #8183, #11426 ) ) ;
#14187 = EDGE_CURVE ( 'NONE', #4841, #12697, #4361, .T. ) ;
#14188 = DIRECTION ( 'NONE',  ( 0.000000000000000000, -0.9996898646859344595, -0.02490330187381124133 ) ) ;
#14189 = VERTEX_POINT ( 'NONE', #3433 ) ;
#14191 = DIRECTION ( 'NONE',  ( -1.000000000000000000, -3.053848253006669023E-16, 2.042510438544995169E-16 ) ) ;
#14190 = CARTESIAN_POINT ( 'NONE',  ( -36.40793637698147478, 4.755763096844229487, 2.574151833883839835 ) ) ;
#14192 = ORIENTED_EDGE ( 'NONE', *, *, #10405, .F. ) ;
#14193 = DIRECTION ( 'NONE',  ( 1.000000000000000000, -0.000000000000000000, -1.047444401652940007E-14 ) ) ;
#14194 = ADVANCED_FACE ( 'NONE', ( #898 ), #12601, .T. ) ;
#14195 = CARTESIAN_POINT ( 'NONE',  ( 57.02075198358709684, 0.7405530952691583568, 1.786721332245943428 ) ) ;
#14196 = AXIS2_PLACEMENT_3D ( 'NONE', #8126, #23595, #22536 ) ;
#14197 = CARTESIAN_POINT ( 'NONE',  ( -54.39999999999996305, -1.399999999999979039, -3.959797974644881258 ) ) ;
#14198 = CARTESIAN_POINT ( 'NONE',  ( -60.59999999999998010, -2.482306123512481477, -1.062147028039162944 ) ) ;
#14199 = CARTESIAN_POINT ( 'NONE',  ( -56.19702994616206837, -2.078460969082657872, 3.599999999999791811 ) ) ;
#14200 = CARTESIAN_POINT ( 'NONE',  ( -59.10189254065529951, -2.466111651437300267, -0.9699939416073426468 ) ) ;
#14201 = EDGE_CURVE ( 'NONE', #2157, #12035, #29859, .T. ) ;
#14202 = DIRECTION ( 'NONE',  ( -1.000000000000000000, 0.000000000000000000, 0.000000000000000000 ) ) ;
#14203 =( BOUNDED_SURFACE ( )  B_SPLINE_SURFACE ( 3, 2, ( 
 ( #7236, #9304, #26541 ),
 ( #14516, #6761, #16899 ),
 ( #19433, #16421, #29079 ),
 ( #6932, #21503, #26075 ) ),
 .UNSPECIFIED., .F., .F., .F. ) 
 B_SPLINE_SURFACE_WITH_KNOTS ( ( 4, 4 ),
 ( 3, 3 ),
 ( 7.500129584393919939E-05, 0.0002378367988924469107 ),
 ( 0.000000000000000000, 1.000000000000000000 ),
 .UNSPECIFIED. ) 
 GEOMETRIC_REPRESENTATION_ITEM ( )  RATIONAL_B_SPLINE_SURFACE ( (
 ( 1.000000000000000000, 0.7071067811864996111, 1.000000000000000000),
 ( 1.000000000000000000, 0.7717803178830575650, 1.000000000000000000),
 ( 1.000000000000000000, 0.8407248428044677979, 1.000000000000000000),
 ( 1.000000000000000000, 0.8397191227596303431, 1.000000000000000000) ) ) 
 REPRESENTATION_ITEM ( '' )  SURFACE ( )  );
#14204 = DIRECTION ( 'NONE',  ( -0.9993908270190957621, 0.03489949670250106634, 3.490838185622846777E-15 ) ) ;
#14205 = CARTESIAN_POINT ( 'NONE',  ( -58.54792740578360366, -2.256877952708278290, 2.542931754211911866 ) ) ;
#14206 = DIRECTION ( 'NONE',  ( 0.000000000000000000, 1.000000000000000000, 3.491481338843130594E-15 ) ) ;
#14207 = VERTEX_POINT ( 'NONE', #27176 ) ;
#14208 = DIRECTION ( 'NONE',  ( 0.000000000000000000, 0.000000000000000000, -1.000000000000000000 ) ) ;
#14209 = CARTESIAN_POINT ( 'NONE',  ( 53.24194194228307708, 4.913799063695436509, 1.606901569590256873 ) ) ;
#14210 = CARTESIAN_POINT ( 'NONE',  ( 53.92227604462289747, 6.075002921772748365, 1.819877325055229145 ) ) ;
#14211 = ORIENTED_EDGE ( 'NONE', *, *, #427, .T. ) ;
#14212 = CARTESIAN_POINT ( 'NONE',  ( -54.49999999999997868, 1.549598385535858380, 4.064203588144675194 ) ) ;
#14213 = ORIENTED_EDGE ( 'NONE', *, *, #502, .F. ) ;
#14214 = CARTESIAN_POINT ( 'NONE',  ( 58.45000000000001705, 0.7500000000000000000, 2.489477856900920383 ) ) ;
#14216 = CARTESIAN_POINT ( 'NONE',  ( 58.50000000000001421, 3.184081677783118191E-16, -2.600000000000000089 ) ) ;
#14215 = CARTESIAN_POINT ( 'NONE',  ( -57.43749999999995737, 1.962990915244761103, -3.400000000000188205 ) ) ;
#14217 = ORIENTED_EDGE ( 'NONE', *, *, #24704, .F. ) ;
#14218 = EDGE_LOOP ( 'NONE', ( #11898, #3195, #8882, #22785 ) ) ;
#14219 = CARTESIAN_POINT ( 'NONE',  ( 60.75000000000002842, -0.6499999999993638644, -1.489337100860647967 ) ) ;
#14220 = EDGE_CURVE ( 'NONE', #29305, #17261, #22594, .T. ) ;
#14221 = DIRECTION ( 'NONE',  ( 0.000000000000000000, 1.000000000000000000, 8.673617379884030739E-15 ) ) ;
#14223 = CARTESIAN_POINT ( 'NONE',  ( 58.72204580543412789, 0.9570475208906656928, 1.612507782426095382 ) ) ;
#14222 = CARTESIAN_POINT ( 'NONE',  ( 56.95000000000001705, 3.184081677783118191E-16, -2.600000000000000089 ) ) ;
#14224 = ORIENTED_EDGE ( 'NONE', *, *, #11181, .T. ) ;
#14225 = CARTESIAN_POINT ( 'NONE',  ( -61.04792740578359656, 3.330682475591789427, 0.6830477631804114935 ) ) ;
#14226 = CARTESIAN_POINT ( 'NONE',  ( 51.70000000000002416, 6.982261990806648555E-14, -1.793082891011605378E-13 ) ) ;
#14227 = DIRECTION ( 'NONE',  ( -1.499696682456116357E-15, -0.9030524935654959950, 0.4295302013422802601 ) ) ;
#14228 = EDGE_CURVE ( 'NONE', #19303, #29056, #10450, .T. ) ;
#14229 = CARTESIAN_POINT ( 'NONE',  ( -35.85663232820584057, 4.018128179617486140, 3.618665901676695995 ) ) ;
#14230 = B_SPLINE_CURVE_WITH_KNOTS ( 'NONE', 3,
 ( #6343, #21094, #23151, #28356, #16323, #1435 ),
 .UNSPECIFIED., .F., .F.,
 ( 4, 2, 4 ),
 ( 0.000000000000000000, 0.0003982002662752204356, 0.0007964005325504408712 ),
 .UNSPECIFIED. ) ;
#14231 = CIRCLE ( 'NONE', #13207, 2.625000000000000444 ) ;
#14232 = DIRECTION ( 'NONE',  ( 0.000000000000000000, 0.000000000000000000, 1.000000000000000000 ) ) ;
#14233 = CARTESIAN_POINT ( 'NONE',  ( -59.22099364905385954, -0.2309624077928886521, -3.875409454552786848 ) ) ;
#14234 = CARTESIAN_POINT ( 'NONE',  ( -62.04999999999998295, -2.687391533643780139, 0.2606275981160435240 ) ) ;
#14235 = ORIENTED_EDGE ( 'NONE', *, *, #25541, .F. ) ;
#14236 = ADVANCED_FACE ( 'NONE', ( #10232 ), #8172, .F. ) ;
#14237 = CYLINDRICAL_SURFACE ( 'NONE', #8928, 2.100000000000000089 ) ;
#14238 =( BOUNDED_CURVE ( )  B_SPLINE_CURVE ( 3, ( #4665, #21470, #28896, #23841 ),
 .UNSPECIFIED., .F., .T. ) 
 B_SPLINE_CURVE_WITH_KNOTS ( ( 4, 4 ),
 ( 5.004066724468453131, 5.113639620782133299 ),
 .UNSPECIFIED. ) 
 CURVE ( )  GEOMETRIC_REPRESENTATION_ITEM ( )  RATIONAL_B_SPLINE_CURVE ( ( 1.000000000000000000, 0.9989997319336324511, 0.9989997319336324511, 1.000000000000000000 ) ) 
 REPRESENTATION_ITEM ( '' )  );
#14239 = CARTESIAN_POINT ( 'NONE',  ( 15.86395258069112479, -3.736273719777164271, 3.909490113446820292 ) ) ;
#14240 = DIRECTION ( 'NONE',  ( 3.491481338843133355E-15, -0.000000000000000000, 1.000000000000000000 ) ) ;
#14241 = ADVANCED_BREP_SHAPE_REPRESENTATION ( '', ( #4661, #9018 ), #25740 ) ;
#14242 = CYLINDRICAL_SURFACE ( 'NONE', #5296, 0.4600000000000000755 ) ;
#14243 = FACE_OUTER_BOUND ( 'NONE', #10367, .T. ) ;
#14244 = CIRCLE ( 'NONE', #28400, 2.700000000000000178 ) ;
#14246 = LINE ( 'NONE', #6336, #18474 ) ;
#14245 = CARTESIAN_POINT ( 'NONE',  ( -61.34573509928848978, -2.599898133715064841, 0.4599265640150483336 ) ) ;
#14247 = EDGE_CURVE ( 'NONE', #15276, #25126, #10933, .T. ) ;
#14248 = VECTOR ( 'NONE', #13132, 1000.000000000000000 ) ;
#14249 = CARTESIAN_POINT ( 'NONE',  ( 51.25000000000001421, 1.163569835200988601E-28, -1.789384186157106949E-13 ) ) ;
#14251 = DIRECTION ( 'NONE',  ( -0.000000000000000000, 1.000000000000000000, 3.491481338843133355E-15 ) ) ;
#14250 = CARTESIAN_POINT ( 'NONE',  ( -74.38999999999998636, -1.239615432210561474, -0.03088009432352123093 ) ) ;
#14252 = EDGE_LOOP ( 'NONE', ( #10743, #28406, #23488, #14658, #2765, #8415, #123, #27454, #24511, #5370, #9697, #17223, #14729, #1839, #27683, #29431, #4527 ) ) ;
#14253 = AXIS2_PLACEMENT_3D ( 'NONE', #27719, #8548, #15688 ) ;
#14254 = CARTESIAN_POINT ( 'NONE',  ( 58.74160516400040422, -1.784764912519645197, 0.5747049900142376933 ) ) ;
#14255 = PRODUCT_DEFINITION_CONTEXT ( 'detailed design', #30768, 'design' ) ;
#14256 = CARTESIAN_POINT ( 'NONE',  ( 51.88812122917394021, 8.998461838226448961, -2.050000000000180123 ) ) ;
#14258 = CARTESIAN_POINT ( 'NONE',  ( -36.43290890416664496, 4.977698683490404008, 2.127480166903978454 ) ) ;
#14257 = CARTESIAN_POINT ( 'NONE',  ( -59.22085481156723574, 1.184343223768590692, 3.558065644182727638 ) ) ;
#14259 = CARTESIAN_POINT ( 'NONE',  ( 16.07279755198632287, -5.235729994560235134, 1.359191621353775137 ) ) ;
#14260 = ORIENTED_EDGE ( 'NONE', *, *, #29734, .T. ) ;
#14261 = VERTEX_POINT ( 'NONE', #25266 ) ;
#14262 = DIRECTION ( 'NONE',  ( 1.000000000000000000, 1.047444401652940007E-14, 0.000000000000000000 ) ) ;
#14263 = EDGE_CURVE ( 'NONE', #11253, #4710, #29703, .T. ) ;
#14264 = ORIENTED_EDGE ( 'NONE', *, *, #24930, .T. ) ;
#14265 = CARTESIAN_POINT ( 'NONE',  ( 47.38300905981536459, -4.256549615192540159, 1.449195206876313202 ) ) ;
#14266 = ADVANCED_FACE ( 'NONE', ( #13071 ), #5487, .T. ) ;
#14267 = CARTESIAN_POINT ( 'NONE',  ( -56.22099364905386665, -0.2309624077928977004, -3.875409454552789956 ) ) ;
#14268 = B_SPLINE_CURVE_WITH_KNOTS ( 'NONE', 3,
 ( #26728, #24193, #17221, #2499, #14354, #14819, #10088, #24480, #17360, #5020, #27007, #12444, #22135, #12154, #426, #29389 ),
 .UNSPECIFIED., .F., .F.,
 ( 4, 2, 2, 2, 2, 2, 2, 4 ),
 ( 1.738108305489988542E-18, 0.0004351083927046443789, 0.0008702167854092870232, 0.001740433570818579684, 0.002175541963523226503, 0.002610650356227873538, 0.003045758748932521007, 0.003480867141637168476 ),
 .UNSPECIFIED. ) ;
#14269 = ORIENTED_EDGE ( 'NONE', *, *, #23024, .F. ) ;
#14270 = ADVANCED_FACE ( 'NONE', ( #19900 ), #8922, .T. ) ;
#14271 = DIRECTION ( 'NONE',  ( 0.000000000000000000, 0.000000000000000000, 1.000000000000000000 ) ) ;
#14272 = ORIENTED_EDGE ( 'NONE', *, *, #15765, .F. ) ;
#14273 = DIRECTION ( 'NONE',  ( 1.000000000000000000, 0.000000000000000000, 0.000000000000000000 ) ) ;
#14274 = CYLINDRICAL_SURFACE ( 'NONE', #28608, 1.625000000000001332 ) ;
#14275 = ORIENTED_EDGE ( 'NONE', *, *, #14187, .F. ) ;
#14276 = ORIENTED_EDGE ( 'NONE', *, *, #18558, .F. ) ;
#14277 = B_SPLINE_CURVE_WITH_KNOTS ( 'NONE', 3,
 ( #19420, #10682, #5625, #30141, #10536, #27459, #15275, #29683, #13200, #17500, #7824, #22884, #27312, #702, #1175, #20366, #24921, #25078, #3240, #20675, #5774, #15426 ),
 .UNSPECIFIED., .F., .F.,
 ( 4, 3, 3, 3, 3, 3, 3, 4 ),
 ( 0.000000000000000000, 1.399909030954194845E-05, 2.803893251624930971E-05, 4.349111487736998725E-05, 6.146574527255033334E-05, 8.260060575193124254E-05, 8.548435886018167966E-05, 8.696130784903155486E-05 ),
 .UNSPECIFIED. ) ;
#14278 = EDGE_LOOP ( 'NONE', ( #11750, #2763, #28179, #19625 ) ) ;
#14279 = CARTESIAN_POINT ( 'NONE',  ( -54.50952994616204705, -3.117691453623963938, -1.800000000000204770 ) ) ;
#14280 = CARTESIAN_POINT ( 'NONE',  ( -57.49999999999997158, 3.673546848079180194, 0.7533615035078097266 ) ) ;
#14281 = CARTESIAN_POINT ( 'NONE',  ( 60.75000000000002842, -0.4999999999993638977, -1.863080903343643069 ) ) ;
#14282 = CARTESIAN_POINT ( 'NONE',  ( -67.99999999999997158, -0.6177564328764010293, 3.012308415424927777 ) ) ;
#14283 = CARTESIAN_POINT ( 'NONE',  ( -60.83824777938995965, -2.520112425590160576, -0.9763468200406411057 ) ) ;
#14284 = DIRECTION ( 'NONE',  ( 0.000000000000000000, -1.000000000000000000, 0.000000000000000000 ) ) ;
#14285 = AXIS2_PLACEMENT_3D ( 'NONE', #14552, #31176, #7585 ) ;
#14286 = EDGE_CURVE ( 'NONE', #27461, #27051, #27329, .T. ) ;
#14287 = FACE_OUTER_BOUND ( 'NONE', #28480, .T. ) ;
#14288 = CARTESIAN_POINT ( 'NONE',  ( 51.15311061045470353, -0.9578955619996478710, -1.386733222354205486 ) ) ;
#14289 = CARTESIAN_POINT ( 'NONE',  ( 57.00000000000001421, -0.6999999999999999556, 1.745709025009609228 ) ) ;
#14290 = EDGE_LOOP ( 'NONE', ( #23532, #26487, #18231, #19999 ) ) ;
#14291 = CARTESIAN_POINT ( 'NONE',  ( 57.00000000000001421, -0.7500000000000000000, 1.778341924377873751 ) ) ;
#14292 = EDGE_CURVE ( 'NONE', #28523, #8746, #5640, .T. ) ;
#14293 = CARTESIAN_POINT ( 'NONE',  ( 50.34656340841117839, 1.329326705022644051, -3.861343257506216098 ) ) ;
#14295 = CARTESIAN_POINT ( 'NONE',  ( 31.59287277085100243, 7.495449159457947097, -1.098631611690421797E-13 ) ) ;
#14294 = CARTESIAN_POINT ( 'NONE',  ( 48.47161145301956253, -1.409900272549268641, 3.850000494969540554 ) ) ;
#14296 = CARTESIAN_POINT ( 'NONE',  ( 54.22606406116597810, 5.661063141734079984, -2.046523645606439956 ) ) ;
#14297 = DIRECTION ( 'NONE',  ( 0.000000000000000000, 0.000000000000000000, 1.000000000000000000 ) ) ;
#14298 = ORIENTED_EDGE ( 'NONE', *, *, #21900, .T. ) ;
#14299 = DIRECTION ( 'NONE',  ( 1.000000000000000000, 1.047444401652940007E-14, 0.000000000000000000 ) ) ;
#14300 = CARTESIAN_POINT ( 'NONE',  ( 51.06445037214141536, -4.311893144378706744, 1.282556980650388700 ) ) ;
#14301 = CARTESIAN_POINT ( 'NONE',  ( -60.12499999999997868, -3.920666489018291502E-15, 3.399999999999785860 ) ) ;
#14302 = VERTEX_POINT ( 'NONE', #3262 ) ;
#14303 = ORIENTED_EDGE ( 'NONE', *, *, #19865, .T. ) ;
#14304 = CARTESIAN_POINT ( 'NONE',  ( 15.03925126672124968, 4.861582140531591989, 2.394243978978380927 ) ) ;
#14305 = ORIENTED_EDGE ( 'NONE', *, *, #11006, .T. ) ;
#14306 = CARTESIAN_POINT ( 'NONE',  ( 50.59602332238209499, 0.1408342061609073048, 0.8215393206232031176 ) ) ;
#14307 = CARTESIAN_POINT ( 'NONE',  ( -58.32202994616204705, -4.156921938165296204, -2.220106322563329850E-13 ) ) ;
#14308 = ORIENTED_EDGE ( 'NONE', *, *, #25882, .T. ) ;
#14309 = DIRECTION ( 'NONE',  ( 1.000000000000000000, 0.000000000000000000, 8.673617379883787770E-15 ) ) ;
#14310 = TOROIDAL_SURFACE ( 'NONE', #24413, 0.4399999999999999467, 0.01000000000000000021 ) ;
#14311 = DIRECTION ( 'NONE',  ( 0.000000000000000000, 0.000000000000000000, 1.000000000000000000 ) ) ;
#14312 = CARTESIAN_POINT ( 'NONE',  ( 31.77414890175571927, 7.582826005769804922, 2.049999999999889244 ) ) ;
#14313 = ORIENTED_EDGE ( 'NONE', *, *, #15021, .T. ) ;
#14314 = DIRECTION ( 'NONE',  ( 0.000000000000000000, 0.000000000000000000, -1.000000000000000000 ) ) ;
#14315 = CARTESIAN_POINT ( 'NONE',  ( 69.25000000000001421, 1.401298464324817071E-42, -7.253552481446610839E-13 ) ) ;
#14316 = CARTESIAN_POINT ( 'NONE',  ( 58.65000000000000568, 1.253243060178336643, -1.394635017528379928 ) ) ;
#14317 = ORIENTED_EDGE ( 'NONE', *, *, #30124, .F. ) ;
#14318 = DIRECTION ( 'NONE',  ( 1.040834085586084257E-14, 0.000000000000000000, 1.000000000000000000 ) ) ;
#14319 = CARTESIAN_POINT ( 'NONE',  ( 56.95000000000001705, 0.000000000000000000, 2.600000000000000089 ) ) ;
#14320 = CARTESIAN_POINT ( 'NONE',  ( -36.38012252111054323, -2.292272662153026719, 4.901537128432083001 ) ) ;
#14321 = ADVANCED_FACE ( 'NONE', ( #3105 ), #19722, .F. ) ;
#14322 = CARTESIAN_POINT ( 'NONE',  ( 51.45655683570189609, 0.9591657938401607630, 1.468576096419531130 ) ) ;
#14323 = EDGE_CURVE ( 'NONE', #6036, #18483, #29168, .T. ) ;
#14324 = DIRECTION ( 'NONE',  ( -2.117927888850090838E-16, 0.02490330187381123786, -0.9996898646859343485 ) ) ;
#14325 = CARTESIAN_POINT ( 'NONE',  ( 58.64999999999991331, -0.6121634413825071119, -1.877732920581102638 ) ) ;
#14326 = EDGE_CURVE ( 'NONE', #29298, #7417, #26111, .T. ) ;
#14327 = TOROIDAL_SURFACE ( 'NONE', #23442, 0.2600000000000000089, 0.01000000000000000021 ) ;
#14328 = ORIENTED_EDGE ( 'NONE', *, *, #20186, .T. ) ;
#14329 = AXIS2_PLACEMENT_3D ( 'NONE', #13454, #30089, #3356 ) ;
#14330 = ORIENTED_EDGE ( 'NONE', *, *, #19296, .F. ) ;
#14331 = CARTESIAN_POINT ( 'NONE',  ( 51.13989201884560742, 0.9305404255937191893, 1.499649012356343514 ) ) ;
#14332 = ORIENTED_EDGE ( 'NONE', *, *, #30479, .F. ) ;
#14333 = CARTESIAN_POINT ( 'NONE',  ( 53.88135321025247748, 4.969568719840013138, 2.049999999999811973 ) ) ;
#14334 = CARTESIAN_POINT ( 'NONE',  ( -54.92292740578361077, 1.073804522883522239, 3.225979517392335794 ) ) ;
#14336 = CARTESIAN_POINT ( 'NONE',  ( -62.39999999999998437, 2.699162634652023662, 0.06723891505929276147 ) ) ;
#14335 = CARTESIAN_POINT ( 'NONE',  ( 52.20711756518984714, -0.7499999999994533262, -1.718465885608440713 ) ) ;
#14337 = EDGE_LOOP ( 'NONE', ( #16979, #3590, #25022, #17332, #6784 ) ) ;
#14338 = ORIENTED_EDGE ( 'NONE', *, *, #16234, .T. ) ;
#14339 = DIRECTION ( 'NONE',  ( 1.000000000000000000, 3.054025858079668409E-16, -2.042474015755241579E-16 ) ) ;
#14340 = ORIENTED_EDGE ( 'NONE', *, *, #16759, .T. ) ;
#14341 = EDGE_CURVE ( 'NONE', #1709, #28800, #25650, .T. ) ;
#14342 = ORIENTED_EDGE ( 'NONE', *, *, #6394, .T. ) ;
#14343 = CARTESIAN_POINT ( 'NONE',  ( -36.14504829323105639, 5.374753047227021518, 0.5963205376974505256 ) ) ;
#14344 = EDGE_LOOP ( 'NONE', ( #10904, #11545, #19914, #9007 ) ) ;
#14345 = DIRECTION ( 'NONE',  ( -1.000000000000000000, -3.053848253006669023E-16, 2.042510438544995415E-16 ) ) ;
#14346 = CARTESIAN_POINT ( 'NONE',  ( 58.75000000000002132, 6.153735859711025284E-13, 3.111507638930570854E-58 ) ) ;
#14347 = LINE ( 'NONE', #23722, #11418 ) ;
#14348 = FACE_OUTER_BOUND ( 'NONE', #25170, .T. ) ;
#14350 = CARTESIAN_POINT ( 'NONE',  ( -56.64405989232412253, -2.944486372867076263, -1.700000000000211786 ) ) ;
#14349 = AXIS2_PLACEMENT_3D ( 'NONE', #22609, #5180, #3274 ) ;
#14351 = CARTESIAN_POINT ( 'NONE',  ( -59.15783187464324300, -2.494370574884575920, -0.9479319139174872122 ) ) ;
#14352 = CARTESIAN_POINT ( 'NONE',  ( -58.62499999999998579, -2.016369211404101147E-14, 3.399999999999791189 ) ) ;
#14353 = CARTESIAN_POINT ( 'NONE',  ( -56.40835481156723574, 4.108500314926515351, -1.367561758111408565 ) ) ;
#14354 = CARTESIAN_POINT ( 'NONE',  ( 15.70940947763171636, -5.349174094756193654, -0.7986533162261060248 ) ) ;
#14355 = EDGE_CURVE ( 'NONE', #17696, #19795, #20574, .T. ) ;
#14356 = VERTEX_POINT ( 'NONE', #13828 ) ;
#14357 = DIRECTION ( 'NONE',  ( -0.5000000000000029976, -3.023711536277451078E-15, 0.8660254037844369313 ) ) ;
#14358 = ORIENTED_EDGE ( 'NONE', *, *, #27476, .T. ) ;
#14359 = DIRECTION ( 'NONE',  ( 0.9993908270191184107, -0.03489949670185085034, -3.491481338843133355E-15 ) ) ;
#14360 = DIRECTION ( 'NONE',  ( 0.000000000000000000, 1.000000000000000000, -1.030899290251718945E-13 ) ) ;
#14361 = DIRECTION ( 'NONE',  ( 0.000000000000000000, 0.000000000000000000, 1.000000000000000000 ) ) ;
#14362 = ORIENTED_EDGE ( 'NONE', *, *, #21581, .F. ) ;
#14363 = DIRECTION ( 'NONE',  ( 1.000000000000000000, 0.000000000000000000, 0.000000000000000000 ) ) ;
#14364 = VERTEX_POINT ( 'NONE', #6117 ) ;
#14365 =( NAMED_UNIT ( * ) SI_UNIT ( $, .STERADIAN. ) SOLID_ANGLE_UNIT ( ) );
#14366 = VECTOR ( 'NONE', #7613, 1000.000000000000000 ) ;
#14368 = CYLINDRICAL_SURFACE ( 'NONE', #3022, 0.05000000000000143219 ) ;
#14367 = DIRECTION ( 'NONE',  ( 1.000000000000000000, 1.047444401652940007E-14, 0.000000000000000000 ) ) ;
#14369 = ORIENTED_EDGE ( 'NONE', *, *, #8696, .F. ) ;
#14370 = DIRECTION ( 'NONE',  ( -1.000000000000000000, -0.000000000000000000, -0.000000000000000000 ) ) ;
#14371 = EDGE_CURVE ( 'NONE', #9408, #25588, #13445, .T. ) ;
#14372 = CARTESIAN_POINT ( 'NONE',  ( -73.89999999999997726, -2.435524336289708093E-15, 4.607889071584891164E-15 ) ) ;
#14374 = CARTESIAN_POINT ( 'NONE',  ( 58.74999981196283727, 0.9033020670129489060, 1.734557215428763621 ) ) ;
#14373 = LINE ( 'NONE', #22625, #16586 ) ;
#14375 = ORIENTED_EDGE ( 'NONE', *, *, #11479, .F. ) ;
#14376 = CARTESIAN_POINT ( 'NONE',  ( -54.81249999999997868, -3.238593381231840151, -2.874284765127021579 ) ) ;
#14377 = AXIS2_PLACEMENT_3D ( 'NONE', #29485, #11385, #6646 ) ;
#14378 = DIRECTION ( 'NONE',  ( 0.000000000000000000, 0.2008964009354148594, -0.9796124928211140670 ) ) ;
#14379 = CARTESIAN_POINT ( 'NONE',  ( -44.59999999999996589, -1.514093959731525496, -3.183260039818558873 ) ) ;
#14380 = CARTESIAN_POINT ( 'NONE',  ( 16.10660252424457184, -3.410993390446848572, -4.205682099886866254 ) ) ;
#14381 = DIRECTION ( 'NONE',  ( 0.000000000000000000, -4.336808689942024836E-15, 1.000000000000000000 ) ) ;
#14382 = CARTESIAN_POINT ( 'NONE',  ( 57.00000000000001421, 0.7500000000000000000, 2.421260002560649660 ) ) ;
#14383 =( BOUNDED_CURVE ( )  B_SPLINE_CURVE ( 3, ( #24929, #3251, #5159, #24470 ),
 .UNSPECIFIED., .F., .T. ) 
 B_SPLINE_CURVE_WITH_KNOTS ( ( 4, 4 ),
 ( 4.050220903230332681, 4.465400561421047243 ),
 .UNSPECIFIED. ) 
 CURVE ( )  GEOMETRIC_REPRESENTATION_ITEM ( )  RATIONAL_B_SPLINE_CURVE ( ( 1.000000000000000000, 0.9856869983806465507, 0.9856869983806465507, 1.000000000000000000 ) ) 
 REPRESENTATION_ITEM ( '' )  );
#14384 = DIRECTION ( 'NONE',  ( -1.000000000000000000, 0.000000000000000000, 3.491481338843133355E-15 ) ) ;
#14385 = B_SPLINE_CURVE_WITH_KNOTS ( 'NONE', 3,
 ( #23438, #15690, #18234, #25340, #30722, #30075 ),
 .UNSPECIFIED., .F., .F.,
 ( 4, 2, 4 ),
 ( 0.000000000000000000, 0.0001701207528151761140, 0.0003402415056303522280 ),
 .UNSPECIFIED. ) ;
#14388 = VERTEX_POINT ( 'NONE', #15909 ) ;
#14387 = ADVANCED_FACE ( 'NONE', ( #30801 ), #25737, .T. ) ;
#14386 = AXIS2_PLACEMENT_3D ( 'NONE', #6226, #27447, #18423 ) ;
#14389 = CARTESIAN_POINT ( 'NONE',  ( 47.02992830280592074, -3.673656954000148023, -1.824471899732945879 ) ) ;
#14390 = CARTESIAN_POINT ( 'NONE',  ( 15.41217651307625758, -3.272340825137230347, 4.050058705652139324 ) ) ;
#14391 = CARTESIAN_POINT ( 'NONE',  ( 49.05000000000005400, 3.520859547548703549E-16, 2.874999999999485745 ) ) ;
#14392 = VECTOR ( 'NONE', #24663, 1000.000000000000000 ) ;
#14393 = CARTESIAN_POINT ( 'NONE',  ( 68.00000000000000000, -0.7500000000000000000, -1.988246715074068582 ) ) ;
#14394 = CARTESIAN_POINT ( 'NONE',  ( 61.25000000000002842, -0.4999999999993586797, 1.807104036850122109 ) ) ;
#14395 = EDGE_CURVE ( 'NONE', #29801, #22859, #15515, .T. ) ;
#14396 = AXIS2_PLACEMENT_3D ( 'NONE', #23629, #9545, #30747 ) ;
#14398 = LINE ( 'NONE', #9976, #4326 ) ;
#14397 = DIRECTION ( 'NONE',  ( 0.000000000000000000, -1.000000000000000000, -0.000000000000000000 ) ) ;
#14399 = CARTESIAN_POINT ( 'NONE',  ( -62.09999999999998010, -2.671081280896091759, -0.3941126626315458181 ) ) ;
#14401 = CARTESIAN_POINT ( 'NONE',  ( 26.87602198329691205, 5.247164978609345276, 1.424999999999906564 ) ) ;
#14400 = DIRECTION ( 'NONE',  ( -1.000000000000000000, 0.000000000000000000, 1.047444401652940007E-14 ) ) ;
#14402 = VERTEX_POINT ( 'NONE', #8486 ) ;
#14403 = CARTESIAN_POINT ( 'NONE',  ( 58.65000000000004121, -1.834410884275049947, 0.3880228184668815250 ) ) ;
#14404 = PLANE ( 'NONE',  #22189 ) ;
#14406 = CARTESIAN_POINT ( 'NONE',  ( -35.85663232820579793, 5.377732432866620726, 0.5657657256216184205 ) ) ;
#14405 = CARTESIAN_POINT ( 'NONE',  ( -54.49999999999997868, 1.734723475976807094E-15, 0.000000000000000000 ) ) ;
#14407 = DIRECTION ( 'NONE',  ( 0.000000000000000000, -0.9996898646859343485, -0.02490330187381123786 ) ) ;
#14408 = ORIENTED_EDGE ( 'NONE', *, *, #20049, .F. ) ;
#14409 = TOROIDAL_SURFACE ( 'NONE', #27611, 4.500000000000037303, 0.1000000000000000056 ) ;
#14410 = ORIENTED_EDGE ( 'NONE', *, *, #21435, .F. ) ;
#14411 = CARTESIAN_POINT ( 'NONE',  ( -57.34585481156722864, -1.184343223768586251, -3.558065644182725862 ) ) ;
#14412 = EDGE_CURVE ( 'NONE', #20276, #1256, #869, .T. ) ;
#14413 = VERTEX_POINT ( 'NONE', #20995 ) ;
#14414 = DIRECTION ( 'NONE',  ( -0.03489949670185085034, -0.9993908270191184107, -2.271278457551021927E-27 ) ) ;
#14415 = AXIS2_PLACEMENT_3D ( 'NONE', #28080, #8755, #15604 ) ;
#14416 = CARTESIAN_POINT ( 'NONE',  ( 58.66054497607991891, 0.5000000000007229772, 1.807104036850091910 ) ) ;
#14417 = VERTEX_POINT ( 'NONE', #8944 ) ;
#14418 = CARTESIAN_POINT ( 'NONE',  ( -36.43290890416663785, -4.977698683490452858, -2.127480166903659597 ) ) ;
#14419 = VERTEX_POINT ( 'NONE', #18628 ) ;
#14420 = CARTESIAN_POINT ( 'NONE',  ( -60.01905989232411542, 2.944486372867092250, 1.699999999999798339 ) ) ;
#14421 =( BOUNDED_CURVE ( )  B_SPLINE_CURVE ( 2, ( #11057, #20735, #18348, #30362, #27986, #6300, #15950, #25611, #3932 ),
 .UNSPECIFIED., .F., .T. ) 
 B_SPLINE_CURVE_WITH_KNOTS ( ( 3, 2, 2, 2, 3 ),
 ( 0.3611111111111111049, 0.3703703703703703498, 0.3888888888888888951, 0.4074074074074073848, 0.4166666666666666852 ),
 .UNSPECIFIED. ) 
 CURVE ( )  GEOMETRIC_REPRESENTATION_ITEM ( )  RATIONAL_B_SPLINE_CURVE ( ( 0.9330127018922194093, 0.9330127018922194093, 1.000000000000000000, 0.8660254037844387076, 1.000000000000000000, 0.8660254037844387076, 1.000000000000000000, 0.9330127018922191873, 0.9330127018922194093 ) ) 
 REPRESENTATION_ITEM ( '' )  );
#14422 = SURFACE_STYLE_USAGE ( .BOTH. , #29308 ) ;
#14423 = CIRCLE ( 'NONE', #9376, 1.949999999999999956 ) ;
#14424 = ORIENTED_EDGE ( 'NONE', *, *, #20359, .F. ) ;
#14425 = EDGE_CURVE ( 'NONE', #12841, #5179, #19995, .T. ) ;
#14426 = ORIENTED_EDGE ( 'NONE', *, *, #18783, .F. ) ;
#14427 = CARTESIAN_POINT ( 'NONE',  ( -54.82202994616206126, 2.078460969082646770, 3.599999999999812683 ) ) ;
#14428 = CARTESIAN_POINT ( 'NONE',  ( 54.16371155698126216, 6.950779743548840983, -2.050000000000189004 ) ) ;
#14429 = DIRECTION ( 'NONE',  ( -9.754918421198724481E-16, 0.9601771338024399638, -0.2793919678926571892 ) ) ;
#14430 = DIRECTION ( 'NONE',  ( 1.047444401652940007E-14, 0.000000000000000000, 1.000000000000000000 ) ) ;
#14431 = CIRCLE ( 'NONE', #3800, 0.1000000000000000472 ) ;
#14432 = CARTESIAN_POINT ( 'NONE',  ( -58.03335481156722864, 0.7533615035077975142, -3.673546848079180638 ) ) ;
#14433 = VECTOR ( 'NONE', #24564, 1000.000000000000000 ) ;
#14434 = ADVANCED_FACE ( 'NONE', ( #13363 ), #20016, .T. ) ;
#14436 = CARTESIAN_POINT ( 'NONE',  ( -36.63359589171323449, -0.7811288459611956947, -5.350925378100957808 ) ) ;
#14435 = CARTESIAN_POINT ( 'NONE',  ( 56.95000000000001705, -0.6999999999999998446, -1.820027472320129514 ) ) ;
#14437 = EDGE_CURVE ( 'NONE', #30441, #18960, #7761, .T. ) ;
#14438 = EDGE_CURVE ( 'NONE', #28113, #26864, #6429, .T. ) ;
#14439 = CARTESIAN_POINT ( 'NONE',  ( -55.43749999999997868, -3.399999999999991473, -2.094585006122325661E-13 ) ) ;
#14440 = DIRECTION ( 'NONE',  ( 0.000000000000000000, 0.000000000000000000, 1.000000000000000000 ) ) ;
#14441 = AXIS2_PLACEMENT_3D ( 'NONE', #7981, #24597, #4982 ) ;
#14442 = CARTESIAN_POINT ( 'NONE',  ( 54.50000000000002132, -0.003244837758069130020, -4.274998768541101057 ) ) ;
#14443 = ORIENTED_EDGE ( 'NONE', *, *, #9759, .T. ) ;
#14444 = AXIS2_PLACEMENT_3D ( 'NONE', #11283, #28245, #22878 ) ;
#14445 = CARTESIAN_POINT ( 'NONE',  ( -61.34999999999997300, -2.583824419212624957, -0.5885162450438690129 ) ) ;
#14447 = CARTESIAN_POINT ( 'NONE',  ( 48.41852494697948828, -1.153996415704668044, -3.890257736381618869 ) ) ;
#14446 = CARTESIAN_POINT ( 'NONE',  ( 48.34311953187607003, -1.211457450596347352, 3.917546004217186351 ) ) ;
#14448 = CARTESIAN_POINT ( 'NONE',  ( 54.22146708689643191, 6.361260388417356637, -2.050000000000189004 ) ) ;
#14449 = ORIENTED_EDGE ( 'NONE', *, *, #24023, .F. ) ;
#14450 = B_SPLINE_CURVE_WITH_KNOTS ( 'NONE', 3,
 ( #10134, #5073, #22021, #9820 ),
 .UNSPECIFIED., .F., .F.,
 ( 4, 4 ),
 ( 0.000000000000000000, 1.000000000000000000 ),
 .UNSPECIFIED. ) ;
#14451 = PLANE ( 'NONE',  #16490 ) ;
#14452 = EDGE_CURVE ( 'NONE', #6127, #9733, #16030, .T. ) ;
#14453 = EDGE_LOOP ( 'NONE', ( #27426, #7206, #12588, #21924, #10244, #23163, #22661, #3713 ) ) ;
#14454 = CARTESIAN_POINT ( 'NONE',  ( 31.35411506561226602, 7.935106537971987173, 1.424999999999891021 ) ) ;
#14455 = CARTESIAN_POINT ( 'NONE',  ( -56.57202994616203995, 2.078460969082674747, -3.600000000000191935 ) ) ;
#14456 = ORIENTED_EDGE ( 'NONE', *, *, #1306, .T. ) ;
#14457 = ORIENTED_EDGE ( 'NONE', *, *, #1318, .T. ) ;
#14458 = CIRCLE ( 'NONE', #28105, 0.2500000000000000000 ) ;
#14459 = CARTESIAN_POINT ( 'NONE',  ( 15.44259799936806132, 4.878092280899815059, 1.814329181850222072 ) ) ;
#14460 = ORIENTED_EDGE ( 'NONE', *, *, #1528, .T. ) ;
#14461 = AXIS2_PLACEMENT_3D ( 'NONE', #11086, #4114, #16315 ) ;
#14462 = CARTESIAN_POINT ( 'NONE',  ( 51.83503441027635716, 4.481775199104232499, 1.044099630206801743 ) ) ;
#14463 = CARTESIAN_POINT ( 'NONE',  ( -56.82202994616205416, -4.156921938165296204, -2.167734102480683039E-13 ) ) ;
#14464 = ORIENTED_EDGE ( 'NONE', *, *, #1139, .F. ) ;
#14465 = DIRECTION ( 'NONE',  ( 0.000000000000000000, 0.000000000000000000, 1.000000000000000000 ) ) ;
#14466 = CIRCLE ( 'NONE', #2332, 2.765000000000001013 ) ;
#14467 = DIRECTION ( 'NONE',  ( 0.9993908270190957621, -0.03489949670250097613, -3.491481338843133355E-15 ) ) ;
#14469 = ADVANCED_FACE ( 'NONE', ( #10305 ), #2875, .T. ) ;
#14468 = CIRCLE ( 'NONE', #807, 3.525000000000025224 ) ;
#14470 = CARTESIAN_POINT ( 'NONE',  ( 30.23587923126626364, 6.713699170112940706, 2.049999999999764011 ) ) ;
#14471 = EDGE_LOOP ( 'NONE', ( #9325, #3381, #8678, #23118, #24949 ) ) ;
#14472 = AXIS2_PLACEMENT_3D ( 'NONE', #19564, #5451, #2458 ) ;
#14473 = VECTOR ( 'NONE', #17151, 1000.000000000000000 ) ;
#14474 = CARTESIAN_POINT ( 'NONE',  ( 47.06312566212015724, 8.366466760780054912, -1.950000000000163380 ) ) ;
#14475 = AXIS2_PLACEMENT_3D ( 'NONE', #29860, #27948, #3263 ) ;
#14476 = ADVANCED_FACE ( 'NONE', ( #19974 ), #29613, .T. ) ;
#14477 = PLANE ( 'NONE',  #3625 ) ;
#14478 = EDGE_LOOP ( 'NONE', ( #30265, #6838, #25789, #15676 ) ) ;
#14479 = FACE_OUTER_BOUND ( 'NONE', #25280, .T. ) ;
#14480 = DIRECTION ( 'NONE',  ( 9.599890688054003756E-15, -0.9507508458638092019, -0.3099561728523110293 ) ) ;
#14481 = AXIS2_PLACEMENT_3D ( 'NONE', #6065, #10650, #22853 ) ;
#14482 = CARTESIAN_POINT ( 'NONE',  ( 58.65263613458528624, -0.8791532451978957274, 1.656197658588203447 ) ) ;
#14483 = ADVANCED_FACE ( 'NONE', ( #26932 ), #7939, .T. ) ;
#14484 = EDGE_CURVE ( 'NONE', #17625, #19844, #3332, .T. ) ;
#14485 = AXIS2_PLACEMENT_3D ( 'NONE', #728, #10561, #29709 ) ;
#14486 = CARTESIAN_POINT ( 'NONE',  ( 51.43355796162960303, 0.9748468443439985975, 1.443681521171340520 ) ) ;
#14487 = CARTESIAN_POINT ( 'NONE',  ( -54.49999999999997868, -4.766731106216463600E-14, -1.834893917355220926E-13 ) ) ;
#14488 = B_SPLINE_CURVE_WITH_KNOTS ( 'NONE', 3,
 ( #22038, #966, #636, #3171 ),
 .UNSPECIFIED., .F., .F.,
 ( 4, 4 ),
 ( 0.000000000000000000, 9.751079247351165789E-06 ),
 .UNSPECIFIED. ) ;
#14490 = CARTESIAN_POINT ( 'NONE',  ( 51.39453088482486010, 4.389042235173731044, 1.549999999999820410 ) ) ;
#14489 = CIRCLE ( 'NONE', #21588, 4.500000000000037303 ) ;
#14491 = EDGE_LOOP ( 'NONE', ( #14910, #20278, #29675, #5367 ) ) ;
#14492 = AXIS2_PLACEMENT_3D ( 'NONE', #10199, #10670, #5927 ) ;
#14493 = VECTOR ( 'NONE', #11349, 1000.000000000000000 ) ;
#14494 = CARTESIAN_POINT ( 'NONE',  ( -59.69999999999998153, 3.161828374300071687, 1.250136525132549581 ) ) ;
#14495 = EDGE_LOOP ( 'NONE', ( #29956, #21311, #26390, #18725, #23174, #21314 ) ) ;
#14496 = CIRCLE ( 'NONE', #9965, 1.000000000000000000 ) ;
#14497 = CARTESIAN_POINT ( 'NONE',  ( 54.16568811108924564, 5.603438171869654205, 2.049999999999811084 ) ) ;
#14498 = CARTESIAN_POINT ( 'NONE',  ( -54.79792740578361077, -2.256877952708263191, 2.542931754211923856 ) ) ;
#14500 = CARTESIAN_POINT ( 'NONE',  ( -36.04581030752770943, 2.525801262579482120, 4.794550356815209469 ) ) ;
#14499 = CARTESIAN_POINT ( 'NONE',  ( 50.87477060347373481, 8.633605004118187765, -1.950000000000176925 ) ) ;
#14501 = EDGE_LOOP ( 'NONE', ( #8387, #25285, #15277, #5438 ) ) ;
#14502 = ORIENTED_EDGE ( 'NONE', *, *, #29487, .T. ) ;
#14503 = DIRECTION ( 'NONE',  ( -1.000000000000000000, -0.000000000000000000, -0.000000000000000000 ) ) ;
#14504 = ORIENTED_EDGE ( 'NONE', *, *, #11318, .F. ) ;
#14505 = DIRECTION ( 'NONE',  ( -1.000000000000000000, -1.047444401652940007E-14, -0.000000000000000000 ) ) ;
#14506 = ORIENTED_EDGE ( 'NONE', *, *, #3219, .F. ) ;
#14507 = CARTESIAN_POINT ( 'NONE',  ( 50.38719906715037666, 1.295960864328800088, 3.889961360030739002 ) ) ;
#14508 = B_SPLINE_CURVE_WITH_KNOTS ( 'NONE', 3,
 ( #24755, #29488, #12558, #10189, #17180, #3065, #27128, #19858, #22543, #2913, #26826, #24299, #22389, #19716, #17801, #2753 ),
 .UNSPECIFIED., .F., .F.,
 ( 4, 3, 3, 3, 3, 4 ),
 ( 0.000000000000000000, 3.304654905548784445E-05, 6.654308848431610937E-05, 0.0001011328993923922879, 0.0001374176636839657517, 0.0001650454644847076165 ),
 .UNSPECIFIED. ) ;
#14509 = CARTESIAN_POINT ( 'NONE',  ( 53.54945434694669615, 7.685534019892441115, 1.865296441523391024 ) ) ;
#14510 = AXIS2_PLACEMENT_3D ( 'NONE', #2857, #7754, #22342 ) ;
#14511 = EDGE_CURVE ( 'NONE', #4409, #23987, #26668, .T. ) ;
#14512 = DIRECTION ( 'NONE',  ( 0.000000000000000000, 1.000000000000000000, 3.491481338843130594E-15 ) ) ;
#14513 = CIRCLE ( 'NONE', #29665, 3.399999999999999911 ) ;
#14514 = EDGE_CURVE ( 'NONE', #1831, #29552, #27146, .T. ) ;
#14515 = AXIS2_PLACEMENT_3D ( 'NONE', #1431, #3187, #8403 ) ;
#14516 = CARTESIAN_POINT ( 'NONE',  ( 57.00000000000001421, 0.7256836306366275524, -1.800271087100996592 ) ) ;
#14517 = EDGE_CURVE ( 'NONE', #11262, #31243, #28302, .T. ) ;
#14518 = CARTESIAN_POINT ( 'NONE',  ( -55.58155989232412963, 3.925981830489463142, -1.832452953121496317E-13 ) ) ;
#14519 = CYLINDRICAL_SURFACE ( 'NONE', #21082, 2.624999999999998668 ) ;
#14520 = CLOSED_SHELL ( 'NONE', ( #8665, #178, #12674, #23991, #10396, #26459, #21268, #17217, #23418, #21035, #11548, #5695, #15327, #3242, #17455, #29316, #11880, #10081, #7106, #15015, #20912, #11907, #28579, #1572, #24540, #23395, #14071, #5245, #28632, #26872, #29496, #22390, #23185, #22585, #21989, #883, #16914, #14857, #9531, #11795, #30666, #13501, #17670, #6516, #12190, #1447, #7652, #17766, #22412, #21817, #17744, #5864, #28415, #7814, #25450, #16898, #2893, #29777, #1592, #8803, #9197, #15256, #15109, #26677, #25842, #1973, #11427, #3393, #6911, #8056, #28341, #4510, #27140, #4078, #10130, #14483, #30746, #6863, #5172, #2283, #19329, #23247, #4895, #17209, #28562, #26209, #22451, #18344, #13079, #7157, #5732, #19104, #13453, #30399, #18315, #9920, #30283, #5145, #8317, #20106, #31096, #24298, #14056, #6088, #22108, #12503, #3618, #11771, #31275, #12821, #14555, #20860, #2487, #28006, #29095, #4870, #24742, #20426, #28856, #14270, #94, #1746, #29571, #29243, #30773, #188, #8037, #30777, #11049, #28757, #17166, #18742, #9769, #20715, #12319, #28194, #8451, #4953, #24147, #117, #18375, #8027, #15712, #15358, #10220, #30313, #22000, #20507, #25478, #13684, #11560, #15351, #1691, #15530, #2003, #4189, #252, #7759, #3179, #31229, #11398, #8242, #22004, #15013, #5, #4205, #27361, #5643, #731, #27472, #9866, #21505, #28387, #27196, #7302, #13189, #11197, #17375, #121, #13277, #21501, #10085, #12153, #27776, #18497, #13843, #11391, #22861, #6708, #22869, #6723, #4936, #13107, #27393, #13705, #7443, #13140, #29256, #18209, #14194, #20752, #4773, #28962, #11534, #13113, #29504, #393, #26642, #19752, #8354, #23639, #23462, #14000, #28466, #25829, #1664, #16784, #13820, #10764, #16730, #2552, #17281 ) ) ;
#14521 = AXIS2_PLACEMENT_3D ( 'NONE', #17763, #22680, #13146 ) ;
#14522 = AXIS2_PLACEMENT_3D ( 'NONE', #17997, #27648, #23223 ) ;
#14524 = AXIS2_PLACEMENT_3D ( 'NONE', #22591, #16941, #2371 ) ;
#14523 = CARTESIAN_POINT ( 'NONE',  ( 56.95000000000001705, 0.000000000000000000, 0.000000000000000000 ) ) ;
#14525 = CARTESIAN_POINT ( 'NONE',  ( 50.40000000000001279, 0.6304760106459517122, -3.950000000000022826 ) ) ;
#14526 = FACE_OUTER_BOUND ( 'NONE', #13238, .T. ) ;
#14527 = ORIENTED_EDGE ( 'NONE', *, *, #26060, .F. ) ;
#14528 = FACE_OUTER_BOUND ( 'NONE', #1364, .T. ) ;
#14529 = ORIENTED_EDGE ( 'NONE', *, *, #5748, .T. ) ;
#14530 = VECTOR ( 'NONE', #3915, 1000.000000000000000 ) ;
#14531 = DIRECTION ( 'NONE',  ( 0.000000000000000000, -1.000000000000000000, 0.000000000000000000 ) ) ;
#14532 = AXIS2_PLACEMENT_3D ( 'NONE', #26703, #26843, #2768 ) ;
#14533 = CARTESIAN_POINT ( 'NONE',  ( -54.46926330052497178, 1.503605180550108944, 3.302415457191590242 ) ) ;
#14534 = CARTESIAN_POINT ( 'NONE',  ( 53.91566580141705600, 6.672244292255798293, 1.816235488581843693 ) ) ;
#14535 = EDGE_LOOP ( 'NONE', ( #17935, #18762, #983, #8571 ) ) ;
#14536 = DIRECTION ( 'NONE',  ( 0.000000000000000000, 0.000000000000000000, 1.000000000000000000 ) ) ;
#14537 = CIRCLE ( 'NONE', #13014, 0.1000000000000007133 ) ;
#14538 = ORIENTED_EDGE ( 'NONE', *, *, #29078, .T. ) ;
#14539 = CARTESIAN_POINT ( 'NONE',  ( 15.48686146417452569, -0.1108756495953492488, -5.200000001675014971 ) ) ;
#14541 = CARTESIAN_POINT ( 'NONE',  ( 50.25000000000000711, 1.106298139389853885, 1.666164585743605375 ) ) ;
#14540 = CARTESIAN_POINT ( 'NONE',  ( 58.73371041428899986, 1.006219588949977650, -1.582294810366573934 ) ) ;
#14542 = EDGE_LOOP ( 'NONE', ( #96, #20320, #2082, #12618 ) ) ;
#14543 = DIRECTION ( 'NONE',  ( 0.000000000000000000, -0.9996898646859343485, -0.02490330187381123786 ) ) ;
#14544 = TOROIDAL_SURFACE ( 'NONE', #8981, 2.549999999999999822, 0.05000000000000000278 ) ;
#14545 = DIRECTION ( 'NONE',  ( -1.000000000000000000, -3.053848253006669023E-16, 2.042510438544995415E-16 ) ) ;
#14546 = CIRCLE ( 'NONE', #8984, 0.01000000000000001929 ) ;
#14548 = CARTESIAN_POINT ( 'NONE',  ( -54.49853245345825314, -1.536420219664552667, -4.055116445457033869 ) ) ;
#14547 = CYLINDRICAL_SURFACE ( 'NONE', #22141, 0.05000000000000143219 ) ;
#14549 = VECTOR ( 'NONE', #8201, 1000.000000000000000 ) ;
#14550 = ORIENTED_EDGE ( 'NONE', *, *, #19188, .F. ) ;
#14551 = CARTESIAN_POINT ( 'NONE',  ( -57.06249999999997158, -3.238593381231840151, -2.874284765127021579 ) ) ;
#14552 = CARTESIAN_POINT ( 'NONE',  ( 59.00000000000002132, 1.401298464324817071E-42, -6.179921969752347932E-13 ) ) ;
#14553 = CARTESIAN_POINT ( 'NONE',  ( 59.00000000000002132, 1.401298464324817071E-42, -6.179921969752347932E-13 ) ) ;
#14554 = CARTESIAN_POINT ( 'NONE',  ( 15.70940947763171636, -3.858136107555796279, -3.790289750283466486 ) ) ;
#14555 = ADVANCED_FACE ( 'NONE', ( #4518 ), #11996, .T. ) ;
#14556 = DIRECTION ( 'NONE',  ( -1.000000000000000000, 0.000000000000000000, 0.000000000000000000 ) ) ;
#14557 = CARTESIAN_POINT ( 'NONE',  ( 52.20711756518984004, -0.4999999999994533817, 1.807104036850122109 ) ) ;
#14558 = DIRECTION ( 'NONE',  ( 1.000000000000000000, 0.000000000000000000, -1.047444401652940007E-14 ) ) ;
#14559 = CIRCLE ( 'NONE', #5975, 0.04999999999999991257 ) ;
#14560 = VERTEX_POINT ( 'NONE', #2135 ) ;
#14561 = VECTOR ( 'NONE', #18614, 1000.000000000000000 ) ;
#14562 = CARTESIAN_POINT ( 'NONE',  ( 58.75000000000000711, 1.469015551796267527, 1.320082690054878549 ) ) ;
#14563 = VECTOR ( 'NONE', #24242, 1000.000000000000000 ) ;
#14564 = CARTESIAN_POINT ( 'NONE',  ( 51.80000000000002558, 4.175664755576631748, 1.929721184273780255 ) ) ;
#14565 = DIRECTION ( 'NONE',  ( -0.9993908270191184107, 0.03489949670185085034, 3.491481338843133355E-15 ) ) ;
#14566 = CARTESIAN_POINT ( 'NONE',  ( -62.05111114591711896, -2.687659336528080534, 0.2567748417330854016 ) ) ;
#14567 = ADVANCED_FACE ( 'NONE', ( #28749 ), #7062, .T. ) ;
#14569 = CARTESIAN_POINT ( 'NONE',  ( 53.35813067190703407, 7.919951180354087406, -1.887104237684443353 ) ) ;
#14568 = DIRECTION ( 'NONE',  ( 1.000000000000000000, 2.586136946169074517E-16, -0.000000000000000000 ) ) ;
#14570 = DIRECTION ( 'NONE',  ( -1.000000000000000000, -3.054025858079668409E-16, 2.042474015755241579E-16 ) ) ;
#14572 = CARTESIAN_POINT ( 'NONE',  ( 22.11060592828335558, 7.457498294695584562, 1.424999999999924105 ) ) ;
#14571 = CARTESIAN_POINT ( 'NONE',  ( 51.18410987668588064, 1.003361152473140505, 1.282358977530924538 ) ) ;
#14573 = ORIENTED_EDGE ( 'NONE', *, *, #8053, .T. ) ;
#14574 = CARTESIAN_POINT ( 'NONE',  ( 58.65000000000000568, 1.022750809562428476, -1.571497941946047083 ) ) ;
#14575 = CARTESIAN_POINT ( 'NONE',  ( 51.45655683570191741, -0.9591657938390838467, -1.611094652690527873 ) ) ;
#14577 = DIRECTION ( 'NONE',  ( 0.000000000000000000, 1.000000000000000000, 0.000000000000000000 ) ) ;
#14576 = CARTESIAN_POINT ( 'NONE',  ( -60.59999999999998010, -2.482306123512481477, -1.062147028039162944 ) ) ;
#14578 = LINE ( 'NONE', #9990, #17111 ) ;
#14579 = ORIENTED_EDGE ( 'NONE', *, *, #27266, .F. ) ;
#14580 = ORIENTED_EDGE ( 'NONE', *, *, #14969, .T. ) ;
#14581 = DIRECTION ( 'NONE',  ( 7.790947421116002101E-15, -0.7438053426818020952, -0.6683962987614510132 ) ) ;
#14582 = AXIS2_PLACEMENT_3D ( 'NONE', #19711, #27282, #12852 ) ;
#14583 = VERTEX_POINT ( 'NONE', #18079 ) ;
#14584 = CARTESIAN_POINT ( 'NONE',  ( -59.92928932188130631, 2.138123341857387114E-15, 5.538933845919563674E-16 ) ) ;
#14585 = DIRECTION ( 'NONE',  ( -1.000000000000000000, -4.678365685400793326E-16, 1.520093157366863638E-16 ) ) ;
#14586 = B_SPLINE_CURVE_WITH_KNOTS ( 'NONE', 3,
 ( #19395, #24294, #24751, #14920, #24586, #12250, #24435, #15247, #19852, #3061, #14627, #10183, #7973, #29037, #3209, #216, #14777, #29198, #17466 ),
 .UNSPECIFIED., .F., .F.,
 ( 4, 3, 3, 3, 3, 3, 4 ),
 ( 7.925977934669585492E-22, 3.356391004153398916E-05, 6.712733219957284561E-05, 0.0001006985180134183105, 0.0001342867383218968741, 0.0001485301915999662963, 0.0001563009630072294926 ),
 .UNSPECIFIED. ) ;
#14587 = EDGE_LOOP ( 'NONE', ( #4238, #21846, #3793, #11177 ) ) ;
#14588 = CARTESIAN_POINT ( 'NONE',  ( -36.25997906085252964, -5.012895491272632675, -1.399447560527455003 ) ) ;
#14589 = ORIENTED_EDGE ( 'NONE', *, *, #13411, .T. ) ;
#14590 = ADVANCED_FACE ( 'NONE', ( #23139 ), #30077, .F. ) ;
#14591 = CARTESIAN_POINT ( 'NONE',  ( -44.49999999999999289, 1.499999999999999556, -4.029888335921975262 ) ) ;
#14592 = ORIENTED_EDGE ( 'NONE', *, *, #4397, .T. ) ;
#14593 = SURFACE_STYLE_USAGE ( .BOTH. , #4933 ) ;
#14594 = EDGE_LOOP ( 'NONE', ( #10328, #22772, #7167, #28257 ) ) ;
#14595 = CARTESIAN_POINT ( 'NONE',  ( -59.38452994616203995, 3.117691453623979481, 1.799999999999801092 ) ) ;
#14596 = CARTESIAN_POINT ( 'NONE',  ( 52.11520194349618862, 3.840337079369375406, -2.050000000000181455 ) ) ;
#14597 = DIRECTION ( 'NONE',  ( 1.000000000000000000, 1.047444401652940007E-14, 0.000000000000000000 ) ) ;
#14598 = CARTESIAN_POINT ( 'NONE',  ( -57.22499999999997300, 2.964020293532818446E-15, 1.549317489258299684E-18 ) ) ;
#14599 = CARTESIAN_POINT ( 'NONE',  ( -58.34585481156723574, -2.489203624310587060, 2.804704140674918911 ) ) ;
#14600 = PRESENTATION_LAYER_ASSIGNMENT (  '', '', ( #11070 ) ) ;
#14601 = AXIS2_PLACEMENT_3D ( 'NONE', #4704, #24199, #14360 ) ;
#14603 = CARTESIAN_POINT ( 'NONE',  ( -36.23324115033522475, 0.2667568399896946829, -5.200000000294884295 ) ) ;
#14602 = CARTESIAN_POINT ( 'NONE',  ( 69.01464466094070360, 4.557543281186736018E-17, -7.228900318216929560E-13 ) ) ;
#14604 = CARTESIAN_POINT ( 'NONE',  ( 52.20711756518983293, 0.6500000000005468070, 1.489337100860647967 ) ) ;
#14605 = CARTESIAN_POINT ( 'NONE',  ( 16.00221665700883733, -2.696520634775326108, 4.691964194339917071 ) ) ;
#14606 = CYLINDRICAL_SURFACE ( 'NONE', #4356, 3.399999999999999911 ) ;
#14607 = ORIENTED_EDGE ( 'NONE', *, *, #6652, .T. ) ;
#14608 = CARTESIAN_POINT ( 'NONE',  ( 58.65000000000003411, -1.253243060177392953, -1.394635017528123910 ) ) ;
#14609 = DIRECTION ( 'NONE',  ( 0.000000000000000000, -1.000000000000000000, -3.491481338843129805E-15 ) ) ;
#14611 = DIRECTION ( 'NONE',  ( -2.614375865348240525E-16, 0.2008964009354147207, -0.9796124928211138450 ) ) ;
#14610 = CARTESIAN_POINT ( 'NONE',  ( 48.42201677308601404, -1.327156576403696553, 3.879406274192464643 ) ) ;
#14612 = EDGE_CURVE ( 'NONE', #16445, #4765, #20598, .T. ) ;
#14613 = ORIENTED_EDGE ( 'NONE', *, *, #6582, .T. ) ;
#14614 = CARTESIAN_POINT ( 'NONE',  ( -54.49999999999997868, 1.734723475976807094E-15, 0.000000000000000000 ) ) ;
#14615 = ORIENTED_EDGE ( 'NONE', *, *, #18655, .F. ) ;
#14616 = DIRECTION ( 'NONE',  ( -1.000000000000000000, -3.054025858079668409E-16, 2.042474015755241579E-16 ) ) ;
#14617 = CARTESIAN_POINT ( 'NONE',  ( -56.75952994616203995, -3.117691453623963938, -1.800000000000212763 ) ) ;
#14618 = ORIENTED_EDGE ( 'NONE', *, *, #22032, .T. ) ;
#14619 = ORIENTED_EDGE ( 'NONE', *, *, #21967, .T. ) ;
#14620 = DIRECTION ( 'NONE',  ( 1.000000000000000000, 1.047444401652940007E-14, 0.000000000000000000 ) ) ;
#14621 = EDGE_LOOP ( 'NONE', ( #31136, #8045, #30770, #6134, #26373, #31284 ) ) ;
#14622 = CARTESIAN_POINT ( 'NONE',  ( 50.80000000000002558, -3.936726248589973221, 1.145507068359715941 ) ) ;
#14623 = AXIS2_PLACEMENT_3D ( 'NONE', #22481, #778, #20128 ) ;
#14624 = EDGE_CURVE ( 'NONE', #24006, #17544, #27646, .T. ) ;
#14625 = CARTESIAN_POINT ( 'NONE',  ( -57.00952994616205416, -4.643455692769903542E-15, 3.599999999999796696 ) ) ;
#14626 = ORIENTED_EDGE ( 'NONE', *, *, #15779, .F. ) ;
#14627 = CARTESIAN_POINT ( 'NONE',  ( 54.49070678691090563, -0.001831363507947880720, 4.318560329337371329 ) ) ;
#14628 = EDGE_CURVE ( 'NONE', #23376, #27880, #11087, .T. ) ;
#14629 = CARTESIAN_POINT ( 'NONE',  ( 51.80000048029754822, 4.021162616303429971, -2.019962949071075542 ) ) ;
#14630 = EDGE_CURVE ( 'NONE', #30797, #20483, #345, .T. ) ;
#14631 = CARTESIAN_POINT ( 'NONE',  ( 34.56702326949726256, 8.213851659285209550, 1.949999999999879385 ) ) ;
#14632 = ORIENTED_EDGE ( 'NONE', *, *, #28082, .F. ) ;
#14633 = CARTESIAN_POINT ( 'NONE',  ( -54.56249999999997158, -1.962990915244707368, -3.400000000000200640 ) ) ;
#14634 = DIRECTION ( 'NONE',  ( 2.581436205204234006E-16, -0.9796124928211140670, -0.2008964009354148872 ) ) ;
#14635 = CARTESIAN_POINT ( 'NONE',  ( 50.55260020142765143, -0.05166409867288173502, -0.7900938592415984729 ) ) ;
#14636 = VECTOR ( 'NONE', #28426, 999.9999999999998863 ) ;
#14637 = CARTESIAN_POINT ( 'NONE',  ( -59.65990137405635352, 2.396397731248872010, -2.649317374334408726 ) ) ;
#14638 = B_SPLINE_CURVE_WITH_KNOTS ( 'NONE', 3,
 ( #13009, #22987, #20317, #27885, #30259, #15707 ),
 .UNSPECIFIED., .F., .F.,
 ( 4, 2, 4 ),
 ( 0.000000000000000000, 0.0001000270069606276543, 0.0002000540139212553085 ),
 .UNSPECIFIED. ) ;
#14639 = CARTESIAN_POINT ( 'NONE',  ( 57.03907689491666844, -0.7490795634100378964, 2.421870079683545285 ) ) ;
#14640 = ADVANCED_FACE ( 'NONE', ( #10769 ), #18059, .T. ) ;
#14641 = AXIS2_PLACEMENT_3D ( 'NONE', #25471, #6316, #25325 ) ;
#14643 = CARTESIAN_POINT ( 'NONE',  ( 50.25000000000000000, 1.996089927834441946, 0.1250000000010043355 ) ) ;
#14642 = FILL_AREA_STYLE_COLOUR ( '', #6379 ) ;
#14644 = PRESENTATION_LAYER_ASSIGNMENT (  '', '', ( #29806 ) ) ;
#14645 = DIRECTION ( 'NONE',  ( 0.000000000000000000, 0.000000000000000000, 1.000000000000000000 ) ) ;
#14646 = CYLINDRICAL_SURFACE ( 'NONE', #19049, 2.700000000000000178 ) ;
#14647 = AXIS2_PLACEMENT_3D ( 'NONE', #6133, #6277, #3597 ) ;
#14648 = AXIS2_PLACEMENT_3D ( 'NONE', #13601, #1425, #28016 ) ;
#14649 = CARTESIAN_POINT ( 'NONE',  ( 61.24794577449344501, -0.9523642485466080609, -1.677218681934459665 ) ) ;
#14650 = ORIENTED_EDGE ( 'NONE', *, *, #23175, .F. ) ;
#14651 = EDGE_CURVE ( 'NONE', #28473, #18214, #6189, .T. ) ;
#14652 = ORIENTED_EDGE ( 'NONE', *, *, #8835, .F. ) ;
#14653 = ORIENTED_EDGE ( 'NONE', *, *, #20025, .F. ) ;
#14654 = DIRECTION ( 'NONE',  ( 0.000000000000000000, -1.000000000000000000, 0.000000000000000000 ) ) ;
#14655 = CARTESIAN_POINT ( 'NONE',  ( -56.67292740578360366, 2.256877952708269408, -2.542931754211925188 ) ) ;
#14657 = DIRECTION ( 'NONE',  ( 0.000000000000000000, 0.000000000000000000, -1.000000000000000000 ) ) ;
#14656 = CARTESIAN_POINT ( 'NONE',  ( -54.49999999999996447, 2.023778652682504319E-14, -3.400000000000193978 ) ) ;
#14658 = ORIENTED_EDGE ( 'NONE', *, *, #25014, .T. ) ;
#14659 = VERTEX_POINT ( 'NONE', #3648 ) ;
#14660 = DIRECTION ( 'NONE',  ( 0.000000000000000000, 1.000000000000000000, 3.491481338843132961E-15 ) ) ;
#14661 = ORIENTED_EDGE ( 'NONE', *, *, #30793, .F. ) ;
#14662 = CARTESIAN_POINT ( 'NONE',  ( 23.93113343277026317, 5.410774079442639994, -1.950000000000083000 ) ) ;
#14663 = EDGE_CURVE ( 'NONE', #17201, #21866, #23027, .T. ) ;
#14664 = ORIENTED_EDGE ( 'NONE', *, *, #4035, .T. ) ;
#14665 = CARTESIAN_POINT ( 'NONE',  ( 31.90749320846404657, 7.645246315295578299, -1.950000000000144063 ) ) ;
#14666 = EDGE_CURVE ( 'NONE', #30371, #11715, #25629, .T. ) ;
#14667 = ORIENTED_EDGE ( 'NONE', *, *, #14824, .F. ) ;
#14668 = CARTESIAN_POINT ( 'NONE',  ( 51.80000000000002558, -4.031600731908413948, 1.173113608511492822 ) ) ;
#14669 = ADVANCED_FACE ( 'NONE', ( #10925 ), #22107, .T. ) ;
#14670 = CARTESIAN_POINT ( 'NONE',  ( 51.80000000000002558, 4.350000000000017408, 1.495827530165114050 ) ) ;
#14671 = AXIS2_PLACEMENT_3D ( 'NONE', #21956, #28912, #7223 ) ;
#14672 = FACE_OUTER_BOUND ( 'NONE', #8425, .T. ) ;
#14673 = VECTOR ( 'NONE', #8763, 1000.000000000000000 ) ;
#14674 = CARTESIAN_POINT ( 'NONE',  ( -55.08155989232411542, -1.962990915244706924, -3.400000000000202416 ) ) ;
#14675 = CARTESIAN_POINT ( 'NONE',  ( 53.49139514279641361, 5.155866831720374854, -1.635615235160539749 ) ) ;
#14676 = AXIS2_PLACEMENT_3D ( 'NONE', #11155, #22894, #27791 ) ;
#14677 = FACE_OUTER_BOUND ( 'NONE', #18102, .T. ) ;
#14678 = CARTESIAN_POINT ( 'NONE',  ( -36.04518387042615757, -3.779372851356037621, -3.883777284340919067 ) ) ;
#14679 = CARTESIAN_POINT ( 'NONE',  ( 49.00000000000002132, 1.401298464324817071E-42, -5.132477568099407673E-13 ) ) ;
#14680 = ORIENTED_EDGE ( 'NONE', *, *, #27040, .T. ) ;
#14681 = EDGE_CURVE ( 'NONE', #16115, #19668, #28393, .T. ) ;
#14682 = CARTESIAN_POINT ( 'NONE',  ( 57.00000000000001421, -0.7263660278559024297, -2.436986164851962844 ) ) ;
#14684 = CARTESIAN_POINT ( 'NONE',  ( -59.69977646026288909, -2.446662296333478537, -1.238409548734900278 ) ) ;
#14683 = CARTESIAN_POINT ( 'NONE',  ( 64.25000000000001421, 1.163569835200988601E-28, -2.243276760206714411E-13 ) ) ;
#14685 = CARTESIAN_POINT ( 'NONE',  ( 53.91582462592152325, 6.672259099522126036, -1.774223561664970861 ) ) ;
#14686 = ORIENTED_EDGE ( 'NONE', *, *, #9991, .F. ) ;
#14687 = CARTESIAN_POINT ( 'NONE',  ( 58.65000000000001279, 0.8495817349404606311, -1.671477153794393766 ) ) ;
#14688 = VERTEX_POINT ( 'NONE', #27873 ) ;
#14689 = ADVANCED_FACE ( 'NONE', ( #12993 ), #13440, .F. ) ;
#14690 = CARTESIAN_POINT ( 'NONE',  ( 15.81621483022863117, 0.7811288459611720469, -5.350925378100957808 ) ) ;
#14691 = CARTESIAN_POINT ( 'NONE',  ( -36.80043232705877898, -4.951626736499100900, 2.174059107776701971 ) ) ;
#14693 = CARTESIAN_POINT ( 'NONE',  ( -67.98046642889043767, 0.6631150920522007608, -3.233486639521205852 ) ) ;
#14692 = DIRECTION ( 'NONE',  ( 0.000000000000000000, 0.000000000000000000, -1.000000000000000000 ) ) ;
#14694 = EDGE_LOOP ( 'NONE', ( #25908, #7378 ) ) ;
#14695 = CARTESIAN_POINT ( 'NONE',  ( 57.05000000000001847, 0.8000000000000000444, -1.778341924377873751 ) ) ;
#14696 = CIRCLE ( 'NONE', #3580, 0.1000000000000002554 ) ;
#14697 = DIRECTION ( 'NONE',  ( 0.000000000000000000, 1.000000000000000000, 4.336808689942015369E-15 ) ) ;
#14699 = DIRECTION ( 'NONE',  ( 0.000000000000000000, 0.000000000000000000, 1.000000000000000000 ) ) ;
#14698 = FACE_OUTER_BOUND ( 'NONE', #20428, .T. ) ;
#14700 = ORIENTED_EDGE ( 'NONE', *, *, #24711, .T. ) ;
#14701 = CARTESIAN_POINT ( 'NONE',  ( -60.87499999999996447, -3.673546848079174865, -0.7533615035078055078 ) ) ;
#14702 = CARTESIAN_POINT ( 'NONE',  ( 61.24312156765933679, 0.9166010152745406314, 1.712896921566334774 ) ) ;
#14703 = CYLINDRICAL_SURFACE ( 'NONE', #17074, 2.374999999999998668 ) ;
#14704 = EDGE_CURVE ( 'NONE', #1571, #2659, #3402, .T. ) ;
#14705 = CARTESIAN_POINT ( 'NONE',  ( 15.18459684427939926, -4.018128179617528772, -3.618665901676669350 ) ) ;
#14706 = CONTEXT_DEPENDENT_SHAPE_REPRESENTATION ( #3120, #30547 ) ;
#14707 = CARTESIAN_POINT ( 'NONE',  ( -54.49999999999997868, -0.2226148165844518412, -3.434203345966388543 ) ) ;
#14708 = DIRECTION ( 'NONE',  ( 0.000000000000000000, 0.000000000000000000, -1.000000000000000000 ) ) ;
#14709 = DIRECTION ( 'NONE',  ( -1.000000000000000000, 0.000000000000000000, -0.000000000000000000 ) ) ;
#14710 = VERTEX_POINT ( 'NONE', #16158 ) ;
#14711 = FACE_OUTER_BOUND ( 'NONE', #26191, .T. ) ;
#14712 = AXIS2_PLACEMENT_3D ( 'NONE', #25001, #10760, #8542 ) ;
#14713 = DIRECTION ( 'NONE',  ( 0.000000000000000000, -0.9996898646859343485, -0.02490330187381124133 ) ) ;
#14714 = DIRECTION ( 'NONE',  ( 0.000000000000000000, 0.6683962987616030027, 0.7438053426816655378 ) ) ;
#14715 = CARTESIAN_POINT ( 'NONE',  ( 50.25000000000000000, 1.800471618824351694, 1.039502773797588597 ) ) ;
#14716 = EDGE_CURVE ( 'NONE', #30753, #4710, #4907, .T. ) ;
#14717 = CARTESIAN_POINT ( 'NONE',  ( 58.45000000000001705, -0.8000000000000000444, -2.421260002560650104 ) ) ;
#14719 = CARTESIAN_POINT ( 'NONE',  ( 58.75000000000002132, 6.153735859711025284E-13, 3.111507638930570854E-58 ) ) ;
#14718 = DIRECTION ( 'NONE',  ( 0.000000000000000000, 0.000000000000000000, -1.000000000000000000 ) ) ;
#14720 = ADVANCED_FACE ( 'NONE', ( #14243 ), #21544, .F. ) ;
#14721 = ORIENTED_EDGE ( 'NONE', *, *, #15635, .F. ) ;
#14722 = CARTESIAN_POINT ( 'NONE',  ( 58.50000000000001421, 0.8000000000000000444, 1.745709025009609228 ) ) ;
#14723 = ORIENTED_EDGE ( 'NONE', *, *, #17724, .T. ) ;
#14724 = EDGE_CURVE ( 'NONE', #30697, #1709, #21398, .T. ) ;
#14725 = CARTESIAN_POINT ( 'NONE',  ( 69.25000000000004263, -0.6441176470588234615, 1.707553061179923448 ) ) ;
#14727 = DIRECTION ( 'NONE',  ( -1.000000000000000000, 1.219044193948983948E-29, -3.491481338843133355E-15 ) ) ;
#14726 = CARTESIAN_POINT ( 'NONE',  ( 15.98305126557417566, -2.728070298465786525, -4.669343935538291746 ) ) ;
#14728 = DIRECTION ( 'NONE',  ( 1.000000000000000000, 1.047444401652940007E-14, 0.000000000000000000 ) ) ;
#14729 = ORIENTED_EDGE ( 'NONE', *, *, #7003, .T. ) ;
#14730 = ORIENTED_EDGE ( 'NONE', *, *, #3509, .T. ) ;
#14731 = DIRECTION ( 'NONE',  ( 0.000000000000000000, 0.000000000000000000, -1.000000000000000000 ) ) ;
#14732 = VERTEX_POINT ( 'NONE', #4115 ) ;
#14733 = CARTESIAN_POINT ( 'NONE',  ( -59.19999999999996732, 4.156921938165317520, -0.9498634748674451567 ) ) ;
#14734 = CARTESIAN_POINT ( 'NONE',  ( -54.98542740578361077, 2.936324665650207333, 2.606018187048498191 ) ) ;
#14735 = ORIENTED_EDGE ( 'NONE', *, *, #1080, .T. ) ;
#14736 = CARTESIAN_POINT ( 'NONE',  ( -36.21152527658242093, -5.035245099686886050, -1.330662535294857340 ) ) ;
#14737 = ORIENTED_EDGE ( 'NONE', *, *, #7674, .F. ) ;
#14738 = EDGE_CURVE ( 'NONE', #2659, #30697, #13396, .T. ) ;
#14739 = CARTESIAN_POINT ( 'NONE',  ( -59.29999999999994742, -3.524955859648372769, 0.4973042051317699275 ) ) ;
#14740 = EDGE_LOOP ( 'NONE', ( #14661, #5024, #7832, #28092 ) ) ;
#14741 = EDGE_LOOP ( 'NONE', ( #11134, #2854, #1679, #7575 ) ) ;
#14742 = AXIS2_PLACEMENT_3D ( 'NONE', #6077, #24900, #12560 ) ;
#14743 = CARTESIAN_POINT ( 'NONE',  ( -56.75952994616203995, -3.117691453623963938, -1.800000000000212763 ) ) ;
#14744 = CARTESIAN_POINT ( 'NONE',  ( 53.71501932699289483, 7.815554144461332342, -2.050000000000187228 ) ) ;
#14745 = PRODUCT_DEFINITION ( 'UNKNOWN', '', #13100, #3156 ) ;
#14746 = CARTESIAN_POINT ( 'NONE',  ( -54.49646078629579193, -1.531523113441621176, 3.320331042554033552 ) ) ;
#14747 = CARTESIAN_POINT ( 'NONE',  ( 51.70000000000000995, -4.276948333784437395, -0.9210526315789474561 ) ) ;
#14748 = CARTESIAN_POINT ( 'NONE',  ( -58.83155989232410832, -1.962990915244687828, -3.400000000000225953 ) ) ;
#14749 = TOROIDAL_SURFACE ( 'NONE', #30942, 4.500000000000037303, 0.1000000000000000056 ) ;
#14751 = CARTESIAN_POINT ( 'NONE',  ( -36.21152527658242093, -0.2904410314644593760, -5.200000000384610743 ) ) ;
#14750 = DIRECTION ( 'NONE',  ( 3.491481338843133355E-15, 0.000000000000000000, 1.000000000000000000 ) ) ;
#14752 = DIRECTION ( 'NONE',  ( 0.000000000000000000, 0.000000000000000000, 1.000000000000000000 ) ) ;
#14753 = CARTESIAN_POINT ( 'NONE',  ( -44.49999999999999289, -1.600000000000004530, 3.363870538531272381 ) ) ;
#14755 = LINE ( 'NONE', #2725, #22076 ) ;
#14754 = CARTESIAN_POINT ( 'NONE',  ( 15.56401610563844962, 4.735424960531769756, -2.618558234549730024 ) ) ;
#14756 = EDGE_CURVE ( 'NONE', #6272, #20516, #8433, .T. ) ;
#14757 = B_SPLINE_CURVE_WITH_KNOTS ( 'NONE', 3,
 ( #1311, #10816, #5929, #23189, #17957, #15736, #30436, #3228, #22555, #17812 ),
 .UNSPECIFIED., .F., .F.,
 ( 4, 3, 3, 4 ),
 ( 0.000000000000000000, 1.446898074592995643E-05, 3.359950008203892456E-05, 3.648946756727797501E-05 ),
 .UNSPECIFIED. ) ;
#14758 = ORIENTED_EDGE ( 'NONE', *, *, #17185, .F. ) ;
#14759 = FACE_OUTER_BOUND ( 'NONE', #23851, .T. ) ;
#14760 =( BOUNDED_CURVE ( )  B_SPLINE_CURVE ( 2, ( #14889, #15059, #17761, #3177, #12817, #642, #7935, #13142, #22502 ),
 .UNSPECIFIED., .F., .T. ) 
 B_SPLINE_CURVE_WITH_KNOTS ( ( 3, 2, 2, 2, 3 ),
 ( 0.3055555555555555802, 0.3148148148148148251, 0.3333333333333333148, 0.3518518518518518601, 0.3611111111111111605 ),
 .UNSPECIFIED. ) 
 CURVE ( )  GEOMETRIC_REPRESENTATION_ITEM ( )  RATIONAL_B_SPLINE_CURVE ( ( 0.9330127018922194093, 0.9330127018922195203, 1.000000000000000000, 0.8660254037844387076, 1.000000000000000000, 0.8660254037844387076, 1.000000000000000000, 0.9330127018922189652, 0.9330127018922194093 ) ) 
 REPRESENTATION_ITEM ( '' )  );
#14761 = DIRECTION ( 'NONE',  ( 1.000000000000000000, 3.054025858079668409E-16, -2.042474015755241579E-16 ) ) ;
#14763 = CARTESIAN_POINT ( 'NONE',  ( 51.87803684735047227, 3.845118170584751915, -1.423186137768011505 ) ) ;
#14762 = DIRECTION ( 'NONE',  ( 0.000000000000000000, 0.000000000000000000, 1.000000000000000000 ) ) ;
#14764 = CARTESIAN_POINT ( 'NONE',  ( -58.31249999999995737, -1.962990915244701151, -3.400000000000217515 ) ) ;
#14765 = ORIENTED_EDGE ( 'NONE', *, *, #21414, .F. ) ;
#14766 = FACE_OUTER_BOUND ( 'NONE', #6903, .T. ) ;
#14767 = ORIENTED_EDGE ( 'NONE', *, *, #9236, .T. ) ;
#14768 = CARTESIAN_POINT ( 'NONE',  ( 51.27864614607251070, 1.002608958138268447, -1.395204572094401740 ) ) ;
#14769 = EDGE_LOOP ( 'NONE', ( #12244, #29237 ) ) ;
#14770 = ORIENTED_EDGE ( 'NONE', *, *, #3145, .F. ) ;
#14771 = DIRECTION ( 'NONE',  ( 0.000000000000000000, 0.9996898646859344595, 0.02490330187381119623 ) ) ;
#14772 = ORIENTED_EDGE ( 'NONE', *, *, #6897, .F. ) ;
#14773 = LINE ( 'NONE', #16860, #4553 ) ;
#14774 = ADVANCED_FACE ( 'NONE', ( #9348 ), #19015, .F. ) ;
#14775 = CARTESIAN_POINT ( 'NONE',  ( -54.63452994616206126, -3.117691453623976816, 1.799999999999793765 ) ) ;
#14776 = ORIENTED_EDGE ( 'NONE', *, *, #28854, .F. ) ;
#14777 = CARTESIAN_POINT ( 'NONE',  ( 54.49989931805382071, -0.003076767801038497469, 4.280178505497699071 ) ) ;
#14778 = CARTESIAN_POINT ( 'NONE',  ( -44.49999999999999289, 2.818925648462311528E-15, 9.856100559121352825E-17 ) ) ;
#14779 = CARTESIAN_POINT ( 'NONE',  ( 30.23587923389744958, 6.713699166094349025, 1.949999999999828315 ) ) ;
#14780 = ORIENTED_EDGE ( 'NONE', *, *, #10356, .T. ) ;
#14781 = CARTESIAN_POINT ( 'NONE',  ( -59.19999999999997442, -3.222669219888746550, 1.250136525132528931 ) ) ;
#14782 = CARTESIAN_POINT ( 'NONE',  ( -54.49999999999997868, -1.549999999999999600, 4.064480286580312907 ) ) ;
#14783 = CARTESIAN_POINT ( 'NONE',  ( 58.65838214097836811, -0.9664062014975295378, -1.606847897768189259 ) ) ;
#14784 = CARTESIAN_POINT ( 'NONE',  ( -56.72499999999997300, 3.116721586436802063E-15, -1.005743832985040150E-16 ) ) ;
#14785 = B_SPLINE_CURVE_WITH_KNOTS ( 'NONE', 3,
 ( #27321, #14963, #714, #29521, #15130, #8477, #20525, #12593 ),
 .UNSPECIFIED., .F., .F.,
 ( 4, 2, 2, 4 ),
 ( 0.000000000000000000, 0.0007042195513453405453, 0.001056329327018010709, 0.001408439102690681091 ),
 .UNSPECIFIED. ) ;
#14786 = ADVANCED_FACE ( 'NONE', ( #26126 ), #25652, .T. ) ;
#14787 = DIRECTION ( 'NONE',  ( -2.081668171172170028E-13, -0.4295302013422817033, -0.9030524935654953289 ) ) ;
#14789 = CARTESIAN_POINT ( 'NONE',  ( 58.75000000000002132, -0.6121634413826994026, 1.877732920581024922 ) ) ;
#14788 = FACE_OUTER_BOUND ( 'NONE', #9581, .T. ) ;
#14790 = CARTESIAN_POINT ( 'NONE',  ( 51.13585994975460380, 0.9262448312174480503, 1.518514878530177414 ) ) ;
#14791 = PLANE ( 'NONE',  #30635 ) ;
#14792 = EDGE_CURVE ( 'NONE', #3421, #9593, #13481, .T. ) ;
#14793 = CARTESIAN_POINT ( 'NONE',  ( 52.98236138753793512, 8.264679131573696935, 1.919164453910085610 ) ) ;
#14794 = ORIENTED_EDGE ( 'NONE', *, *, #4429, .T. ) ;
#14795 = ORIENTED_EDGE ( 'NONE', *, *, #9494, .T. ) ;
#14796 = ORIENTED_EDGE ( 'NONE', *, *, #11867, .T. ) ;
#14797 = AXIS2_PLACEMENT_3D ( 'NONE', #4018, #4167, #15885 ) ;
#14798 = CARTESIAN_POINT ( 'NONE',  ( -56.11042740578360366, -2.936324665650200672, -2.606018187048498191 ) ) ;
#14800 = CARTESIAN_POINT ( 'NONE',  ( -35.85663232820592583, 2.686240680702101979, 4.475885388010746979 ) ) ;
#14799 = CARTESIAN_POINT ( 'NONE',  ( 50.55258015808398397, 5.295040916136730406E-13, 1.177580158083963546 ) ) ;
#14801 = ORIENTED_EDGE ( 'NONE', *, *, #20532, .F. ) ;
#14802 = CARTESIAN_POINT ( 'NONE',  ( 54.02713021818536987, 5.727804820055879098, -2.034063242164690255 ) ) ;
#14803 = ORIENTED_EDGE ( 'NONE', *, *, #969, .F. ) ;
#14804 = DIRECTION ( 'NONE',  ( 3.002035892788117459E-16, -0.9996898646859344595, -0.02490330187381123786 ) ) ;
#14805 = EDGE_CURVE ( 'NONE', #13278, #14388, #29398, .T. ) ;
#14806 = ORIENTED_EDGE ( 'NONE', *, *, #15293, .T. ) ;
#14807 = CARTESIAN_POINT ( 'NONE',  ( 31.77414890175468898, 7.582826005769556232, -2.049999999999980282 ) ) ;
#14808 = VERTEX_POINT ( 'NONE', #4592 ) ;
#14809 = CARTESIAN_POINT ( 'NONE',  ( 51.21021026411729338, -1.041641720704776786, 1.248302399389048079 ) ) ;
#14810 = CARTESIAN_POINT ( 'NONE',  ( 64.99999999999997158, -1.025519176787267142E-28, -4.100000000000680878 ) ) ;
#14811 = CARTESIAN_POINT ( 'NONE',  ( 15.81621483022852281, -4.847650360853460683, -2.396424556483019774 ) ) ;
#14812 = CARTESIAN_POINT ( 'NONE',  ( -54.83155989232412963, 3.925981830489463142, -1.806266843080172912E-13 ) ) ;
#14813 = EDGE_CURVE ( 'NONE', #28557, #26264, #18824, .T. ) ;
#14814 = CARTESIAN_POINT ( 'NONE',  ( 53.49139514279633545, 5.155866831720416599, -2.050000000000122835 ) ) ;
#14815 = DIRECTION ( 'NONE',  ( -1.000000000000000000, 0.000000000000000000, -0.000000000000000000 ) ) ;
#14816 = CARTESIAN_POINT ( 'NONE',  ( -36.38012252111054323, -3.953287617511738627, -3.694739123711016759 ) ) ;
#14817 = TOROIDAL_SURFACE ( 'NONE', #20413, 2.424999999999998934, 0.05000000000000000278 ) ;
#14818 = AXIS2_PLACEMENT_3D ( 'NONE', #20161, #29790, #8105 ) ;
#14819 = CARTESIAN_POINT ( 'NONE',  ( 16.00221665700883733, -5.295593823078813323, -1.114646847977642130 ) ) ;
#14820 = EDGE_CURVE ( 'NONE', #16720, #17544, #12472, .T. ) ;
#14821 = DIRECTION ( 'NONE',  ( -2.964772755551650383E-16, -0.9875000000000001554, -0.1576190026614809614 ) ) ;
#14822 = EDGE_CURVE ( 'NONE', #30937, #13475, #2874, .T. ) ;
#14823 = ORIENTED_EDGE ( 'NONE', *, *, #25376, .T. ) ;
#14824 = EDGE_CURVE ( 'NONE', #1900, #3598, #28823, .T. ) ;
#14825 = DIRECTION ( 'NONE',  ( -1.047444401652940007E-14, 0.000000000000000000, -1.000000000000000000 ) ) ;
#14826 = CARTESIAN_POINT ( 'NONE',  ( -36.76447480099788123, -3.646691605040335737, -3.993181011920743373 ) ) ;
#14827 = CARTESIAN_POINT ( 'NONE',  ( 53.94302949754625587, 6.378738024272571749, 1.816235488581843693 ) ) ;
#14828 = VERTEX_POINT ( 'NONE', #29284 ) ;
#14829 = DIRECTION ( 'NONE',  ( 1.000000000000000000, 1.047444401652940007E-14, 0.000000000000000000 ) ) ;
#14830 = ORIENTED_EDGE ( 'NONE', *, *, #12146, .T. ) ;
#14831 = CARTESIAN_POINT ( 'NONE',  ( 15.86395258069112124, 0.7247683022689473953, -5.358970532132275366 ) ) ;
#14832 = CARTESIAN_POINT ( 'NONE',  ( 48.30260100412290569, 0.9326869175216770946, 3.995127421239667687 ) ) ;
#14834 = CARTESIAN_POINT ( 'NONE',  ( -61.84501029485813461, -2.660356430927216298, -0.4698869684439438976 ) ) ;
#14833 = CARTESIAN_POINT ( 'NONE',  ( 48.43326094847141405, -1.398826622412639775, -3.854114288381606190 ) ) ;
#14835 = ORIENTED_EDGE ( 'NONE', *, *, #3852, .T. ) ;
#14836 = CARTESIAN_POINT ( 'NONE',  ( 51.59739104186227365, 1.010292945603182169, 1.272765950230260401 ) ) ;
#14837 = CARTESIAN_POINT ( 'NONE',  ( -44.59999999999997300, -6.102218906431391608E-14, -1.870876429524648473E-13 ) ) ;
#14839 = CARTESIAN_POINT ( 'NONE',  ( -54.48779575765000516, -1.517266520141196118, -4.041867453639657271 ) ) ;
#14838 = CARTESIAN_POINT ( 'NONE',  ( 52.64068875113407131, 4.063124538860861001, 2.046235746538459743 ) ) ;
#14840 = DIRECTION ( 'NONE',  ( 0.000000000000000000, 0.000000000000000000, 1.000000000000000000 ) ) ;
#14841 = CARTESIAN_POINT ( 'NONE',  ( -60.49999999999997158, 3.673546848079180194, 0.7533615035078067290 ) ) ;
#14842 = AXIS2_PLACEMENT_3D ( 'NONE', #10711, #1662, #27959 ) ;
#14843 = LINE ( 'NONE', #12628, #14549 ) ;
#14844 = CIRCLE ( 'NONE', #21391, 2.000000000000000000 ) ;
#14845 = CARTESIAN_POINT ( 'NONE',  ( 15.59140265158956495, -2.334862116274967647, -4.877703086529571408 ) ) ;
#14846 = CARTESIAN_POINT ( 'NONE',  ( -44.59999999999998721, 1.599999999999998090, 3.363870538531281706 ) ) ;
#14847 = FACE_OUTER_BOUND ( 'NONE', #31259, .T. ) ;
#14848 = CARTESIAN_POINT ( 'NONE',  ( -67.99999999999997158, 2.708628542650380666, 0.5554785485864246475 ) ) ;
#14849 = EDGE_CURVE ( 'NONE', #1083, #23733, #15007, .T. ) ;
#14850 = EDGE_LOOP ( 'NONE', ( #376, #12208, #30015, #1759 ) ) ;
#14851 = EDGE_CURVE ( 'NONE', #24741, #31043, #26894, .T. ) ;
#14852 = CARTESIAN_POINT ( 'NONE',  ( 15.03925126672123014, -4.018128179617556306, 3.618665901676639596 ) ) ;
#14853 = DIRECTION ( 'NONE',  ( 0.000000000000000000, -4.336808689942006692E-15, 1.000000000000000000 ) ) ;
#14854 = DIRECTION ( 'NONE',  ( 1.000000000000000000, -0.000000000000000000, -0.000000000000000000 ) ) ;
#14855 = CARTESIAN_POINT ( 'NONE',  ( 58.65000000000003411, -1.077297519403678017, 1.655311165517035166 ) ) ;
#14856 = CIRCLE ( 'NONE', #9322, 2.000000000000000000 ) ;
#14857 = ADVANCED_FACE ( 'NONE', ( #5207 ), #19789, .F. ) ;
#14858 = CARTESIAN_POINT ( 'NONE',  ( 61.23913277633471353, -0.8963220027428320247, 1.755758457447560428 ) ) ;
#14860 = DIRECTION ( 'NONE',  ( -1.583552166641333955E-32, 1.224646799147353207E-16, 1.000000000000000000 ) ) ;
#14859 = CARTESIAN_POINT ( 'NONE',  ( 58.66122389686762517, 0.5174758696803309910, 1.802487374212454307 ) ) ;
#14861 = ORIENTED_EDGE ( 'NONE', *, *, #19438, .T. ) ;
#14862 = CARTESIAN_POINT ( 'NONE',  ( 47.00000000000002132, -3.826179070414207573, -1.100000000000000089 ) ) ;
#14863 = ORIENTED_EDGE ( 'NONE', *, *, #23141, .T. ) ;
#14864 = DIRECTION ( 'NONE',  ( -8.860386339788720432E-15, 0.8459051693633012903, -0.5333333333333336590 ) ) ;
#14865 = AXIS2_PLACEMENT_3D ( 'NONE', #8206, #8517, #30359 ) ;
#14867 = DIRECTION ( 'NONE',  ( 0.000000000000000000, 0.9783524716136585697, 0.2069455031824692648 ) ) ;
#14866 = CARTESIAN_POINT ( 'NONE',  ( 57.00319509709754584, 0.7184317838911207232, -2.441240553461111684 ) ) ;
#14868 = CARTESIAN_POINT ( 'NONE',  ( 57.00000000000001421, -0.7500000000000000000, -1.778341924377873751 ) ) ;
#14869 = ORIENTED_EDGE ( 'NONE', *, *, #13599, .F. ) ;
#14870 = AXIS2_PLACEMENT_3D ( 'NONE', #7564, #2656, #22140 ) ;
#14871 = EDGE_LOOP ( 'NONE', ( #16344, #14464, #29542 ) ) ;
#14872 = DIRECTION ( 'NONE',  ( -3.002035892788116966E-16, 0.9996898646859343485, 0.02490330187381124133 ) ) ;
#14873 = CARTESIAN_POINT ( 'NONE',  ( 47.49384476122470033, -3.992023072242622206, 1.294577227648573192 ) ) ;
#14874 =( BOUNDED_CURVE ( )  B_SPLINE_CURVE ( 2, ( #20005, #2746, #7797, #5124, #19554, #9878, #527, #26673, #22241 ),
 .UNSPECIFIED., .F., .T. ) 
 B_SPLINE_CURVE_WITH_KNOTS ( ( 3, 2, 2, 2, 3 ),
 ( 0.2500000000000000000, 0.2592592592592592449, 0.2777777777777777901, 0.2962962962962962798, 0.3055555555555555802 ),
 .UNSPECIFIED. ) 
 CURVE ( )  GEOMETRIC_REPRESENTATION_ITEM ( )  RATIONAL_B_SPLINE_CURVE ( ( 0.9330127018922192983, 0.9330127018922194093, 1.000000000000000000, 0.8660254037844387076, 1.000000000000000000, 0.8660254037844387076, 1.000000000000000000, 0.9330127018922191873, 0.9330127018922194093 ) ) 
 REPRESENTATION_ITEM ( '' )  );
#14875 = ORIENTED_EDGE ( 'NONE', *, *, #7097, .T. ) ;
#14876 = CARTESIAN_POINT ( 'NONE',  ( 51.79029922165371858, -4.153760649298012808, 1.055564289358534413 ) ) ;
#14877 = CARTESIAN_POINT ( 'NONE',  ( -55.42292740578360366, -3.330682475591783209, -0.6830477631804113825 ) ) ;
#14878 = CARTESIAN_POINT ( 'NONE',  ( -77.28999999999996362, 0.2499224661714801732, 0.006225825468458142005 ) ) ;
#14879 = ORIENTED_EDGE ( 'NONE', *, *, #28240, .F. ) ;
#14880 = DIRECTION ( 'NONE',  ( 1.000000000000000000, 0.000000000000000000, 0.000000000000000000 ) ) ;
#14881 = DIRECTION ( 'NONE',  ( 0.000000000000000000, -0.3333333333333282633, 0.9428090415820651327 ) ) ;
#14882 = AXIS2_PLACEMENT_3D ( 'NONE', #21814, #5003, #103 ) ;
#14883 = EDGE_CURVE ( 'NONE', #15123, #15285, #4838, .T. ) ;
#14884 = ORIENTED_EDGE ( 'NONE', *, *, #27419, .F. ) ;
#14885 = EDGE_CURVE ( 'NONE', #22540, #21420, #16990, .T. ) ;
#14886 = CARTESIAN_POINT ( 'NONE',  ( -57.75952994616205416, -4.643455692769894075E-15, 3.599999999999794031 ) ) ;
#14887 = ADVANCED_FACE ( 'NONE', ( #12043 ), #27594, .T. ) ;
#14888 = CARTESIAN_POINT ( 'NONE',  ( 51.74548155811469741, 3.822334312940638412, -2.050000000000177902 ) ) ;
#14889 = CARTESIAN_POINT ( 'NONE',  ( -56.33155989232412963, 3.400000000000008349, -1.856946929144785632E-13 ) ) ;
#14890 = CARTESIAN_POINT ( 'NONE',  ( 58.45000000000001705, 0.8000000000000000444, 3.499999999999999556 ) ) ;
#14891 = CARTESIAN_POINT ( 'NONE',  ( -71.44999999999998863, -1.380331489585512972E-15, 2.906968604901091669E-15 ) ) ;
#14892 = DIRECTION ( 'NONE',  ( 1.000000000000000000, 1.047444401652940007E-14, 0.000000000000000000 ) ) ;
#14894 = CARTESIAN_POINT ( 'NONE',  ( -36.58361892165972762, -0.1071614981651333592, -5.407381887150175537 ) ) ;
#14893 = DIRECTION ( 'NONE',  ( 0.000000000000000000, -0.3589743589743574215, -0.9333474217026310749 ) ) ;
#14895 = CIRCLE ( 'NONE', #15916, 0.1500000000000001887 ) ;
#14896 = CARTESIAN_POINT ( 'NONE',  ( -54.44999999999997442, -1.499999999999998668, 4.029888335921975262 ) ) ;
#14897 = CARTESIAN_POINT ( 'NONE',  ( 51.85262340636811729, 0.6891204047495619323, -1.750401715244590539 ) ) ;
#14899 = DIRECTION ( 'NONE',  ( -1.000000000000000000, -0.000000000000000000, 3.491481338843133355E-15 ) ) ;
#14898 = CARTESIAN_POINT ( 'NONE',  ( 54.49754940158101846, -0.002530889200248514093, -4.297001851131137862 ) ) ;
#14900 = ADVANCED_FACE ( 'NONE', ( #19644 ), #10270, .T. ) ;
#14901 = ORIENTED_EDGE ( 'NONE', *, *, #30579, .T. ) ;
#14902 = CARTESIAN_POINT ( 'NONE',  ( 58.65000000000003411, -1.371849028670161896, -1.278599783848962668 ) ) ;
#14903 = AXIS2_PLACEMENT_3D ( 'NONE', #26953, #15241, #24887 ) ;
#14904 = CARTESIAN_POINT ( 'NONE',  ( 47.10000000000003695, 2.428612866367529932E-14, 4.099999999999827338 ) ) ;
#14906 = DIRECTION ( 'NONE',  ( -1.000000000000000000, 1.219044193948983948E-29, -3.491481338843133355E-15 ) ) ;
#14905 = CARTESIAN_POINT ( 'NONE',  ( -44.49999999999999289, -1.500000000000000000, 3.300094695611020867 ) ) ;
#14907 = CARTESIAN_POINT ( 'NONE',  ( 54.15675781068899397, 5.684314874070254042, -2.050000000000189004 ) ) ;
#14908 = EDGE_LOOP ( 'NONE', ( #2727, #30017, #18475, #30754 ) ) ;
#14909 = CARTESIAN_POINT ( 'NONE',  ( -61.35733863216196227, -2.634673853764536222, 0.4689153067231007777 ) ) ;
#14910 = ORIENTED_EDGE ( 'NONE', *, *, #22387, .F. ) ;
#14911 = AXIS2_PLACEMENT_3D ( 'NONE', #13464, #1446, #4136 ) ;
#14912 = FACE_OUTER_BOUND ( 'NONE', #16977, .T. ) ;
#14913 = EDGE_LOOP ( 'NONE', ( #11387, #11257, #14177, #23811 ) ) ;
#14914 = ORIENTED_EDGE ( 'NONE', *, *, #6756, .T. ) ;
#14915 = CARTESIAN_POINT ( 'NONE',  ( 57.05000000000001847, -0.7500000000000000000, -1.745709025009609228 ) ) ;
#14916 = VERTEX_POINT ( 'NONE', #15020 ) ;
#14917 = DIRECTION ( 'NONE',  ( -1.000000000000000000, -3.053848253006669023E-16, 2.042510438544995415E-16 ) ) ;
#14918 = CARTESIAN_POINT ( 'NONE',  ( -55.33155989232414385, -1.962990915244731571, 3.399999999999794742 ) ) ;
#14919 = ORIENTED_EDGE ( 'NONE', *, *, #21365, .T. ) ;
#14920 = CARTESIAN_POINT ( 'NONE',  ( 54.43308742068420969, -0.0001827659103420331901, 4.369367483123359541 ) ) ;
#14921 = VECTOR ( 'NONE', #19058, 1000.000000000000000 ) ;
#14922 = CARTESIAN_POINT ( 'NONE',  ( 22.79271333219191931, 6.591595603791505553, 2.049999999999919442 ) ) ;
#14923 = ORIENTED_EDGE ( 'NONE', *, *, #22966, .F. ) ;
#14924 = EDGE_CURVE ( 'NONE', #10954, #13383, #30509, .T. ) ;
#14925 = CIRCLE ( 'NONE', #26577, 2.525000000000001688 ) ;
#14926 = B_SPLINE_CURVE_WITH_KNOTS ( 'NONE', 3,
 ( #24284, #16701, #2438, #21616, #19074, #2595, #9405, #4796, #205, #18912, #16534, #26189, #23971, #4492, #14454 ),
 .UNSPECIFIED., .F., .F.,
 ( 4, 1, 1, 1, 1, 1, 1, 1, 1, 1, 1, 1, 4 ),
 ( 0.03200690811994862106, 0.06212998257909596589, 0.1242599651581919179, 0.2485199303163838636, 0.3727798954745757953, 0.4970398606327676716, 0.6212998257909596589, 0.6834298083700556248, 0.7455597909491514796, 0.8076897735282474455, 0.8387547648177954285, 0.8698197561073434114, 0.8953196948241715081 ),
 .UNSPECIFIED. ) ;
#14927 = CARTESIAN_POINT ( 'NONE',  ( 51.78364358464229156, 0.9002346248706185605, -1.360127766454892084 ) ) ;
#14928 = DIRECTION ( 'NONE',  ( 1.000000000000000000, 3.054025858079668409E-16, -2.042474015755241579E-16 ) ) ;
#14929 = CARTESIAN_POINT ( 'NONE',  ( 58.74999999999980815, -1.022750809560559526, -1.571497941946463861 ) ) ;
#14930 = CARTESIAN_POINT ( 'NONE',  ( 57.05000000000001847, 0.8156862745098041323, -2.468735688885368873 ) ) ;
#14931 = CARTESIAN_POINT ( 'NONE',  ( 57.00103033359725657, 0.7116617362530316404, 2.445288145576760552 ) ) ;
#14932 = TOROIDAL_SURFACE ( 'NONE', #11388, 4.600000000000000533, 0.4999999999999996669 ) ;
#14933 = CIRCLE ( 'NONE', #25533, 1.000000000000000000 ) ;
#14935 = DIRECTION ( 'NONE',  ( 0.000000000000000000, 0.000000000000000000, -1.000000000000000000 ) ) ;
#14934 = CARTESIAN_POINT ( 'NONE',  ( -35.85663232820601820, -4.018128179617563411, 3.618665901676646257 ) ) ;
#14936 =( BOUNDED_SURFACE ( )  B_SPLINE_SURFACE ( 3, 2, ( 
 ( #1118, #22830, #5236 ),
 ( #27546, #5872, #27247 ),
 ( #10767, #7626, #25187 ),
 ( #17285, #12522, #15533 ),
 ( #29452, #26928, #24551 ),
 ( #2871, #15361, #494 ),
 ( #25011, #12670, #22205 ),
 ( #22676, #5564, #29931 ),
 ( #3339, #8240, #10153 ),
 ( #15213, #19820, #24714 ) ),
 .UNSPECIFIED., .F., .F., .F. ) 
 B_SPLINE_SURFACE_WITH_KNOTS ( ( 4, 2, 2, 2, 4 ),
 ( 3, 3 ),
 ( 0.0004005301535625022482, 0.0008279283193725973976, 0.001041627402277645054, 0.001148476943730168936, 0.001255326485182692601 ),
 ( 0.000000000000000000, 1.000000000000000000 ),
 .UNSPECIFIED. ) 
 GEOMETRIC_REPRESENTATION_ITEM ( )  RATIONAL_B_SPLINE_SURFACE ( (
 ( 1.000000000000000000, 0.7071067811865260344, 1.000000000000000000),
 ( 1.000000000000000000, 0.7463463187144947497, 1.000000000000000000),
 ( 1.000000000000000000, 0.7946150999565809725, 1.000000000000000000),
 ( 1.000000000000000000, 0.8720431506958414847, 1.000000000000000000),
 ( 1.000000000000000000, 0.8987780092778684393, 1.000000000000000000),
 ( 1.000000000000000000, 0.9375340664365204857, 1.000000000000000000),
 ( 1.000000000000000000, 0.9504270566176279411, 1.000000000000000000),
 ( 1.000000000000000000, 0.9732249474031190450, 1.000000000000000000),
 ( 1.000000000000000000, 0.9839441327696822892, 1.000000000000000000),
 ( 1.000000000000000000, 0.9842509842514762797, 1.000000000000000000) ) ) 
 REPRESENTATION_ITEM ( '' )  SURFACE ( )  );
#14937 = DIRECTION ( 'NONE',  ( -1.000000000000000000, -0.000000000000000000, -0.000000000000000000 ) ) ;
#14938 = DIRECTION ( 'NONE',  ( 3.696862594069201137E-15, -0.9356455129756980904, 0.3529411764705883137 ) ) ;
#14939 = ADVANCED_FACE ( 'NONE', ( #21870 ), #14952, .T. ) ;
#14940 = CARTESIAN_POINT ( 'NONE',  ( -54.49646078629579193, 1.531523113441620731, -3.320331042554034440 ) ) ;
#14941 = CARTESIAN_POINT ( 'NONE',  ( 53.74478519188840409, 7.379842749953129832, 1.837855077339518362 ) ) ;
#14942 = ORIENTED_EDGE ( 'NONE', *, *, #7735, .F. ) ;
#14943 = CIRCLE ( 'NONE', #13413, 0.2499999999999987788 ) ;
#14944 = CIRCLE ( 'NONE', #1298, 2.000000000000000000 ) ;
#14945 = ORIENTED_EDGE ( 'NONE', *, *, #21423, .T. ) ;
#14946 = ORIENTED_EDGE ( 'NONE', *, *, #29123, .F. ) ;
#14947 = LINE ( 'NONE', #699, #11351 ) ;
#14948 = CARTESIAN_POINT ( 'NONE',  ( -60.42292740578359656, 2.256877952708268520, -2.542931754211924300 ) ) ;
#14950 = CARTESIAN_POINT ( 'NONE',  ( 50.50000000000002132, -0.6462379109120514054, -4.048750000000023164 ) ) ;
#14949 = DIRECTION ( 'NONE',  ( -9.754918421198722508E-16, -0.9601771338024398528, -0.2793919678926571337 ) ) ;
#14951 = ORIENTED_EDGE ( 'NONE', *, *, #30046, .F. ) ;
#14952 = TOROIDAL_SURFACE ( 'NONE', #31147, 4.800000000000000711, 0.05000000000000000278 ) ;
#14953 = EDGE_LOOP ( 'NONE', ( #19269, #29505, #10799, #29270 ) ) ;
#14954 = CARTESIAN_POINT ( 'NONE',  ( 50.93148713995405785, -4.319730106380442081, -1.256953381515634849 ) ) ;
#14955 = ORIENTED_EDGE ( 'NONE', *, *, #26257, .T. ) ;
#14956 = AXIS2_PLACEMENT_3D ( 'NONE', #17324, #24758, #10342 ) ;
#14957 = DIRECTION ( 'NONE',  ( 0.000000000000000000, -1.000000000000000000, 0.000000000000000000 ) ) ;
#14958 = ORIENTED_EDGE ( 'NONE', *, *, #15259, .F. ) ;
#14959 = CARTESIAN_POINT ( 'NONE',  ( 27.54696499482717442, 5.363421040582472266, -1.950000000000027711 ) ) ;
#14960 = AXIS2_PLACEMENT_3D ( 'NONE', #27505, #3751, #6145 ) ;
#14961 = ORIENTED_EDGE ( 'NONE', *, *, #23787, .F. ) ;
#14962 = CARTESIAN_POINT ( 'NONE',  ( -57.45655989232412253, -3.399999999999991029, -2.148039047887444390E-13 ) ) ;
#14963 = CARTESIAN_POINT ( 'NONE',  ( 47.76370854686960854, -3.908336260473453727, 1.238913909465753971 ) ) ;
#14964 = EDGE_CURVE ( 'NONE', #22807, #1093, #13927, .T. ) ;
#14965 = B_SPLINE_CURVE_WITH_KNOTS ( 'NONE', 3,
 ( #26427, #14705, #9664, #19320, #14554, #7266, #14380, #2986, #28955, #7430, #17103, #16932, #14845, #17387, #10113, #24365 ),
 .UNSPECIFIED., .F., .F.,
 ( 4, 2, 2, 2, 2, 2, 2, 4 ),
 ( 1.734723475976807094E-18, 0.0004351083927046438368, 0.0008702167854092859390, 0.001740433570818577733, 0.002175541963523223467, 0.002610650356227869635, 0.003045758748932515369, 0.003480867141637161537 ),
 .UNSPECIFIED. ) ;
#14966 = AXIS2_PLACEMENT_3D ( 'NONE', #16494, #18879, #25983 ) ;
#14967 = FACE_OUTER_BOUND ( 'NONE', #21782, .T. ) ;
#14968 = CARTESIAN_POINT ( 'NONE',  ( -61.00952994616203284, 3.117691453623994580, -1.800000000000202993 ) ) ;
#14969 = EDGE_CURVE ( 'NONE', #3863, #21049, #2206, .T. ) ;
#14970 = CARTESIAN_POINT ( 'NONE',  ( 53.78456803694546551, 5.661108390837235937, -2.050000000000250289 ) ) ;
#14971 = AXIS2_PLACEMENT_3D ( 'NONE', #17361, #5021, #29391 ) ;
#14972 = CYLINDRICAL_SURFACE ( 'NONE', #23732, 0.2500000000000002220 ) ;
#14973 = CIRCLE ( 'NONE', #22564, 1.000000000000000000 ) ;
#14974 = DIRECTION ( 'NONE',  ( 0.000000000000000000, 0.000000000000000000, -1.000000000000000000 ) ) ;
#14975 = CARTESIAN_POINT ( 'NONE',  ( 50.33290990662629838, 1.365599538210783281, -3.854893000251051749 ) ) ;
#14976 = AXIS2_PLACEMENT_3D ( 'NONE', #4668, #11961, #26515 ) ;
#14977 = AXIS2_PLACEMENT_3D ( 'NONE', #15139, #20066, #5968 ) ;
#14978 = FACE_OUTER_BOUND ( 'NONE', #11773, .T. ) ;
#14979 = AXIS2_PLACEMENT_3D ( 'NONE', #3035, #22509, #19831 ) ;
#14980 = CIRCLE ( 'NONE', #3355, 0.2500000000000000000 ) ;
#14981 = CARTESIAN_POINT ( 'NONE',  ( 49.04999999999999716, 3.459627207591271682E-16, -2.825000000000512657 ) ) ;
#14982 = ORIENTED_EDGE ( 'NONE', *, *, #14228, .T. ) ;
#14983 = CARTESIAN_POINT ( 'NONE',  ( 58.75000000000003553, -1.470078920827206925, -1.470078920827526892 ) ) ;
#14984 = CARTESIAN_POINT ( 'NONE',  ( -36.68866260399369850, -2.562020839648592396, -4.763023844701044673 ) ) ;
#14985 = CARTESIAN_POINT ( 'NONE',  ( 54.21130113843405951, 6.699806482265510787, 2.049999999999811529 ) ) ;
#14986 = VERTEX_POINT ( 'NONE', #18037 ) ;
#14987 = CARTESIAN_POINT ( 'NONE',  ( 50.33710128586459120, 1.426739617975221863, -3.843750000000023981 ) ) ;
#14988 = ORIENTED_EDGE ( 'NONE', *, *, #15227, .F. ) ;
#14989 = VECTOR ( 'NONE', #17968, 1000.000000000000000 ) ;
#14990 = CARTESIAN_POINT ( 'NONE',  ( 15.66436536804551416, 0.4008586329627058520, -5.396496690166812549 ) ) ;
#14991 = DIRECTION ( 'NONE',  ( 3.491481338843133355E-15, -0.000000000000000000, 1.000000000000000000 ) ) ;
#14993 = CARTESIAN_POINT ( 'NONE',  ( 47.12350347295471664, -3.663955391962992802, -1.843087722223818004 ) ) ;
#14992 = DIRECTION ( 'NONE',  ( 0.000000000000000000, -1.000000000000000000, -0.000000000000000000 ) ) ;
#14994 = ADVANCED_FACE ( 'NONE', ( #6155 ), #10887, .F. ) ;
#14995 = ORIENTED_EDGE ( 'NONE', *, *, #18671, .F. ) ;
#14996 = CIRCLE ( 'NONE', #9950, 1.875000000000001776 ) ;
#14997 = LINE ( 'NONE', #7868, #14392 ) ;
#14998 = CIRCLE ( 'NONE', #17038, 1.875000000000001776 ) ;
#14999 = DIRECTION ( 'NONE',  ( -0.000000000000000000, -0.9875000000000001554, 0.1576190026614806561 ) ) ;
#15000 = AXIS2_PLACEMENT_3D ( 'NONE', #26294, #8703, #25658 ) ;
#15001 = ORIENTED_EDGE ( 'NONE', *, *, #10583, .F. ) ;
#15002 = ORIENTED_EDGE ( 'NONE', *, *, #13411, .F. ) ;
#15003 = CARTESIAN_POINT ( 'NONE',  ( -60.12499999999996447, -3.673546848079174421, -0.7533615035078056188 ) ) ;
#15004 = DIRECTION ( 'NONE',  ( -1.000000000000000000, -3.053848253006669023E-16, 2.042510438544995415E-16 ) ) ;
#15005 = AXIS2_PLACEMENT_3D ( 'NONE', #9389, #19059, #7024 ) ;
#15006 = CARTESIAN_POINT ( 'NONE',  ( -58.03335481156722864, 0.7533615035077975142, -3.673546848079180638 ) ) ;
#15007 = CIRCLE ( 'NONE', #1356, 0.1000000000000000194 ) ;
#15008 = EDGE_CURVE ( 'NONE', #25398, #66, #27215, .T. ) ;
#15009 = CARTESIAN_POINT ( 'NONE',  ( -54.49999999999998579, -3.534339970052580160, -1.064353278733559893 ) ) ;
#15010 = CARTESIAN_POINT ( 'NONE',  ( -59.69999999999996021, 1.397030005794335672, -3.099726949734703751 ) ) ;
#15011 = CIRCLE ( 'NONE', #25607, 4.199999999999993072 ) ;
#15012 = AXIS2_PLACEMENT_3D ( 'NONE', #29046, #4666, #19404 ) ;
#15013 = ADVANCED_FACE ( 'NONE', ( #15659 ), #25151, .F. ) ;
#15014 = DIRECTION ( 'NONE',  ( 0.000000000000000000, 4.440892098500626951E-15, 1.000000000000000000 ) ) ;
#15015 = ADVANCED_FACE ( 'NONE', ( #20269 ), #30212, .T. ) ;
#15016 = CARTESIAN_POINT ( 'NONE',  ( 15.90468948301723628, -0.6818242347930719705, 5.365311767243448493 ) ) ;
#15017 = ORIENTED_EDGE ( 'NONE', *, *, #14292, .F. ) ;
#15018 = CARTESIAN_POINT ( 'NONE',  ( 15.44259799936806488, 2.880023619481773434, 4.335093843541880432 ) ) ;
#15019 = AXIS2_PLACEMENT_3D ( 'NONE', #25433, #3735, #8646 ) ;
#15020 = CARTESIAN_POINT ( 'NONE',  ( -61.34999999999997300, -2.399215024517336925, -0.7870147813924887048 ) ) ;
#15021 = EDGE_CURVE ( 'NONE', #473, #3555, #24080, .T. ) ;
#15022 = VECTOR ( 'NONE', #14054, 1000.000000000000000 ) ;
#15023 = CYLINDRICAL_SURFACE ( 'NONE', #30606, 0.1500000000000001887 ) ;
#15024 = CARTESIAN_POINT ( 'NONE',  ( -57.63452994616205416, -3.117691453623982589, 1.799999999999773337 ) ) ;
#15025 = CARTESIAN_POINT ( 'NONE',  ( -56.90400635094608361, 1.737685414808523454, -3.471684241605564658 ) ) ;
#15027 = CARTESIAN_POINT ( 'NONE',  ( 27.56628230087643416, 5.372092466067856620, 1.424999999999904565 ) ) ;
#15026 = FACE_OUTER_BOUND ( 'NONE', #3605, .T. ) ;
#15028 = ORIENTED_EDGE ( 'NONE', *, *, #3756, .T. ) ;
#15029 = AXIS2_PLACEMENT_3D ( 'NONE', #19923, #17239, #19628 ) ;
#15030 = DIRECTION ( 'NONE',  ( 1.000000000000000000, 1.047444401652940007E-14, -0.000000000000000000 ) ) ;
#15031 = AXIS2_PLACEMENT_3D ( 'NONE', #20701, #6267, #8323 ) ;
#15032 = ORIENTED_EDGE ( 'NONE', *, *, #27741, .T. ) ;
#15033 = CIRCLE ( 'NONE', #17580, 2.800000000000000266 ) ;
#15034 = CARTESIAN_POINT ( 'NONE',  ( -35.85663232820584057, 3.426725943139506292, 3.937891353488775170 ) ) ;
#15036 = CARTESIAN_POINT ( 'NONE',  ( 58.71354657862850246, -0.4999999999993852695, -1.821913688936154241 ) ) ;
#15035 = DIRECTION ( 'NONE',  ( 1.000000000000000000, 0.000000000000000000, -1.047444401652940007E-14 ) ) ;
#15037 = CARTESIAN_POINT ( 'NONE',  ( 57.00000000000001421, 0.7500000000000000000, -2.421260002560649216 ) ) ;
#15038 = EDGE_CURVE ( 'NONE', #5081, #19802, #25152, .T. ) ;
#15039 = ORIENTED_EDGE ( 'NONE', *, *, #25043, .T. ) ;
#15040 = ORIENTED_EDGE ( 'NONE', *, *, #10433, .T. ) ;
#15041 = PLANE ( 'NONE',  #28528 ) ;
#15042 = LINE ( 'NONE', #27063, #11613 ) ;
#15043 = ORIENTED_EDGE ( 'NONE', *, *, #12922, .T. ) ;
#15044 = ADVANCED_FACE ( 'NONE', ( #11353 ), #17076, .T. ) ;
#15045 = CARTESIAN_POINT ( 'NONE',  ( -59.19312575602410931, 2.408440864227364919, 1.250136525132548693 ) ) ;
#15046 = DIRECTION ( 'NONE',  ( 0.000000000000000000, 0.000000000000000000, 1.000000000000000000 ) ) ;
#15047 = CIRCLE ( 'NONE', #15548, 2.625000000000000444 ) ;
#15048 = CARTESIAN_POINT ( 'NONE',  ( -36.39645873810205501, -5.286410563980360244, -1.167394352644205213 ) ) ;
#15049 = CARTESIAN_POINT ( 'NONE',  ( 0.000000000000000000, 0.000000000000000000, 0.000000000000000000 ) ) ;
#15050 = TOROIDAL_SURFACE ( 'NONE', #21666, 4.800000000000000711, 0.05000000000000000278 ) ;
#15051 = CARTESIAN_POINT ( 'NONE',  ( -54.39999999999999147, -1.400000000000006795, 3.959797974644449603 ) ) ;
#15052 = AXIS2_PLACEMENT_3D ( 'NONE', #23560, #16757, #14204 ) ;
#15053 = ADVANCED_FACE ( 'NONE', ( #14526 ), #7883, .T. ) ;
#15054 = ADVANCED_FACE ( 'NONE', ( #5169 ), #2790, .T. ) ;
#15055 = ORIENTED_EDGE ( 'NONE', *, *, #6148, .F. ) ;
#15056 = VECTOR ( 'NONE', #14505, 1000.000000000000000 ) ;
#15057 = CARTESIAN_POINT ( 'NONE',  ( -57.57202994616204705, -4.156921938165296204, -2.193920212522006445E-13 ) ) ;
#15058 = CARTESIAN_POINT ( 'NONE',  ( 50.50000000000002132, 0.6462379109120995890, 4.048750000000023164 ) ) ;
#15059 = CARTESIAN_POINT ( 'NONE',  ( -56.36505354137801049, 3.400000000000011902, -0.9110272542659988426 ) ) ;
#15060 = CARTESIAN_POINT ( 'NONE',  ( 68.00000000000004263, -0.7500000000000000000, 1.988246715072644166 ) ) ;
#15061 = CARTESIAN_POINT ( 'NONE',  ( 59.34999999999999432, 4.286263797015737088E-16, -3.500000000000622169 ) ) ;
#15062 = CARTESIAN_POINT ( 'NONE',  ( 58.75000000000002132, 6.153735859711025284E-13, 3.111507638930570854E-58 ) ) ;
#15064 = CARTESIAN_POINT ( 'NONE',  ( -36.80043232705879319, -0.5375162698823703344, -5.381098085087390182 ) ) ;
#15063 = CARTESIAN_POINT ( 'NONE',  ( -59.54784193156670113, -3.076428338433373710, 1.450963157958014449 ) ) ;
#15065 = AXIS2_PLACEMENT_3D ( 'NONE', #28413, #28258, #23500 ) ;
#15066 = LINE ( 'NONE', #7633, #23117 ) ;
#15067 = CARTESIAN_POINT ( 'NONE',  ( 16.08093158123429234, -3.408535483610572570, 4.200031884472242183 ) ) ;
#15069 = CARTESIAN_POINT ( 'NONE',  ( -54.49999999999996447, -1.399999999999981259, -3.300094695611242468 ) ) ;
#15068 = CARTESIAN_POINT ( 'NONE',  ( 54.49508724208691746, -0.002176679993726876768, -4.307918145378301311 ) ) ;
#15070 = ORIENTED_EDGE ( 'NONE', *, *, #28524, .T. ) ;
#15071 =( BOUNDED_CURVE ( )  B_SPLINE_CURVE ( 2, ( #29101, #6954, #2032, #14215, #19308, #16920, #4711, #7251, #25937 ),
 .UNSPECIFIED., .F., .T. ) 
 B_SPLINE_CURVE_WITH_KNOTS ( ( 3, 2, 2, 2, 3 ),
 ( 0.4166666666666666852, 0.4259259259259259300, 0.4444444444444444198, 0.4629629629629629650, 0.4722222222222222654 ),
 .UNSPECIFIED. ) 
 CURVE ( )  GEOMETRIC_REPRESENTATION_ITEM ( )  RATIONAL_B_SPLINE_CURVE ( ( 0.9330127018922194093, 0.9330127018922195203, 1.000000000000000000, 0.8660254037844387076, 1.000000000000000000, 0.8660254037844387076, 1.000000000000000000, 0.9330127018922189652, 0.9330127018922194093 ) ) 
 REPRESENTATION_ITEM ( '' )  );
#15072 = DIRECTION ( 'NONE',  ( 1.000000000000000000, 0.000000000000000000, -0.000000000000000000 ) ) ;
#15073 = CARTESIAN_POINT ( 'NONE',  ( -36.81959771849334828, -4.939398376933301194, -2.210903708596504202 ) ) ;
#15075 = CARTESIAN_POINT ( 'NONE',  ( 52.37358958628623640, 3.908449573900731444, 1.241066825229008685 ) ) ;
#15074 = CARTESIAN_POINT ( 'NONE',  ( 51.32028027175453389, -1.012964966966786617, -1.577985093213079448 ) ) ;
#15076 = FACE_OUTER_BOUND ( 'NONE', #14337, .T. ) ;
#15077 = ADVANCED_FACE ( 'NONE', ( #26549 ), #9775, .F. ) ;
#15078 = ORIENTED_EDGE ( 'NONE', *, *, #6783, .T. ) ;
#15079 = CARTESIAN_POINT ( 'NONE',  ( 58.75000000000004263, -2.008165151418633165, 0.5380862305909606125 ) ) ;
#15080 = CARTESIAN_POINT ( 'NONE',  ( 51.86029176559893017, 0.1231600413635689645, -4.365376941996956361 ) ) ;
#15081 = EDGE_CURVE ( 'NONE', #18214, #9901, #14268, .T. ) ;
#15082 = ORIENTED_EDGE ( 'NONE', *, *, #228, .T. ) ;
#15083 = EDGE_CURVE ( 'NONE', #21866, #30858, #11189, .T. ) ;
#15084 = DIRECTION ( 'NONE',  ( 0.000000000000000000, -0.9996898646859343485, -0.02490330187381116153 ) ) ;
#15085 = ORIENTED_EDGE ( 'NONE', *, *, #6697, .F. ) ;
#15086 = ORIENTED_EDGE ( 'NONE', *, *, #8014, .T. ) ;
#15087 = CARTESIAN_POINT ( 'NONE',  ( 15.30042582489632608, 5.377732434016984975, 0.5657657146872882015 ) ) ;
#15088 = VERTEX_POINT ( 'NONE', #2648 ) ;
#15089 = DIRECTION ( 'NONE',  ( 0.000000000000000000, 0.000000000000000000, 1.000000000000000000 ) ) ;
#15090 = CARTESIAN_POINT ( 'NONE',  ( -54.51905989232412963, -2.944486372867088697, 1.699999999999795008 ) ) ;
#15091 = ORIENTED_EDGE ( 'NONE', *, *, #14438, .F. ) ;
#15092 = CARTESIAN_POINT ( 'NONE',  ( 61.16864364483389238, -0.7080009476652142641, -1.871974308544436250 ) ) ;
#15093 = DIRECTION ( 'NONE',  ( -2.095850865446309212E-30, -1.000000000000000000, -2.891205793294679411E-15 ) ) ;
#15094 = AXIS2_PLACEMENT_3D ( 'NONE', #31207, #19195, #1736 ) ;
#15095 = CARTESIAN_POINT ( 'NONE',  ( 22.00282357524792687, 7.757228885921422012, 2.050000000000460787 ) ) ;
#15096 = ORIENTED_EDGE ( 'NONE', *, *, #17352, .T. ) ;
#15097 = CARTESIAN_POINT ( 'NONE',  ( 51.50435016707358216, 0.9265794315412900772, -1.339215852266870233 ) ) ;
#15098 = DIRECTION ( 'NONE',  ( -1.000000000000000000, 0.000000000000000000, -3.491481338843153471E-15 ) ) ;
#15099 = CARTESIAN_POINT ( 'NONE',  ( 60.94140446608462014, 0.5380862305989584371, -1.858165151370887669 ) ) ;
#15100 = B_SPLINE_CURVE_WITH_KNOTS ( 'NONE', 3,
 ( #6385, #580, #19909, #14445 ),
 .UNSPECIFIED., .F., .F.,
 ( 4, 4 ),
 ( 0.000000000000000000, 9.751079247352095831E-06 ),
 .UNSPECIFIED. ) ;
#15101 = CARTESIAN_POINT ( 'NONE',  ( 51.14630318392405428, 0.9364487020640391846, 1.503522130792586342 ) ) ;
#15103 = DIRECTION ( 'NONE',  ( 9.754918421198724481E-16, 0.9601771338024399638, 0.2793919678926571892 ) ) ;
#15102 = CARTESIAN_POINT ( 'NONE',  ( -36.58361892165971341, -3.091683853622008371, 4.437651790014588649 ) ) ;
#15104 = CARTESIAN_POINT ( 'NONE',  ( 50.33625478868709990, -1.419210040599374612, -3.846553521706499001 ) ) ;
#15105 = CARTESIAN_POINT ( 'NONE',  ( 58.75000000000003553, -1.666164585742487159, -1.106298139390194724 ) ) ;
#15106 = CARTESIAN_POINT ( 'NONE',  ( -54.44999999999997442, 1.549999999999999600, 4.029888335921975262 ) ) ;
#15107 = CARTESIAN_POINT ( 'NONE',  ( -61.34999999999997300, -2.528827883897363904, -0.7921676171260561006 ) ) ;
#15108 = ORIENTED_EDGE ( 'NONE', *, *, #29371, .T. ) ;
#15109 = ADVANCED_FACE ( 'NONE', ( #14978 ), #29249, .F. ) ;
#15110 =( GEOMETRIC_REPRESENTATION_CONTEXT ( 3 ) GLOBAL_UNCERTAINTY_ASSIGNED_CONTEXT ( ( #8219 ) ) GLOBAL_UNIT_ASSIGNED_CONTEXT ( ( #19508, #22964, #25182 ) ) REPRESENTATION_CONTEXT ( 'NONE', 'WORKASPACE' ) );
#15111 = EDGE_CURVE ( 'NONE', #15962, #2126, #28112, .T. ) ;
#15112 = ORIENTED_EDGE ( 'NONE', *, *, #23377, .F. ) ;
#15113 = VECTOR ( 'NONE', #22729, 1000.000000000000000 ) ;
#15114 = VERTEX_POINT ( 'NONE', #29086 ) ;
#15115 = EDGE_CURVE ( 'NONE', #17127, #7637, #7398, .T. ) ;
#15116 = CYLINDRICAL_SURFACE ( 'NONE', #243, 0.1500000000000001887 ) ;
#15117 = CARTESIAN_POINT ( 'NONE',  ( -57.98542740578359656, 2.936324665650206889, 2.606018187048499080 ) ) ;
#15119 = CARTESIAN_POINT ( 'NONE',  ( -59.32290219554960942, 2.336760081911408271, 1.249820915005386279 ) ) ;
#15118 = DIRECTION ( 'NONE',  ( -0.9993908270191184107, 0.03489949670185085034, 3.491481338843133355E-15 ) ) ;
#15120 = VERTEX_POINT ( 'NONE', #21975 ) ;
#15121 = ORIENTED_EDGE ( 'NONE', *, *, #25059, .F. ) ;
#15122 = DIRECTION ( 'NONE',  ( 0.000000000000000000, 0.9996898646859343485, 0.02490330187381123786 ) ) ;
#15123 = VERTEX_POINT ( 'NONE', #26403 ) ;
#15124 = DIRECTION ( 'NONE',  ( 1.000000000000000000, -0.000000000000000000, -1.047444401652940007E-14 ) ) ;
#15125 = ORIENTED_EDGE ( 'NONE', *, *, #15478, .F. ) ;
#15126 = CARTESIAN_POINT ( 'NONE',  ( 28.70703846152805028, 5.747922418238541553, -1.950000000000162936 ) ) ;
#15127 = MANIFOLD_SOLID_BREP ( 'Stock-MAS-683-1', #22632 ) ;
#15128 = CARTESIAN_POINT ( 'NONE',  ( 46.90000000000001279, 1.734723475976807094E-15, 0.000000000000000000 ) ) ;
#15129 = CIRCLE ( 'NONE', #18181, 160.6997717543497686 ) ;
#15130 = CARTESIAN_POINT ( 'NONE',  ( 47.21343356430319460, -3.755435527867144962, 1.648753881545072630 ) ) ;
#15131 = VERTEX_POINT ( 'NONE', #8024 ) ;
#15132 = ADVANCED_FACE ( 'NONE', ( #5799 ), #19146, .T. ) ;
#15133 = CARTESIAN_POINT ( 'NONE',  ( 15.86395258069124559, -4.872718122832710996, -2.345308583460518292 ) ) ;
#15134 = CARTESIAN_POINT ( 'NONE',  ( -59.45655989232410832, 1.962990915244748891, -3.400000000000202416 ) ) ;
#15135 = CARTESIAN_POINT ( 'NONE',  ( 52.54946733419072302, 4.465216787881787219, -2.050000000000182787 ) ) ;
#15136 = CARTESIAN_POINT ( 'NONE',  ( 48.00000000000001421, -4.031600731908414836, -1.173113608511841877 ) ) ;
#15137 = AXIS2_PLACEMENT_3D ( 'NONE', #18359, #23116, #1554 ) ;
#15138 = CARTESIAN_POINT ( 'NONE',  ( 48.48125827213483774, 1.426739617975217866, -3.843750000000022649 ) ) ;
#15139 = CARTESIAN_POINT ( 'NONE',  ( 60.75000000000003553, -0.9999999999993638422, -1.996089927833914146 ) ) ;
#15140 = FACE_OUTER_BOUND ( 'NONE', #16829, .T. ) ;
#15141 = PRODUCT_DEFINITION ( 'UNKNOWN', '', #3504, #12334 ) ;
#15142 = CARTESIAN_POINT ( 'NONE',  ( -59.14664939113121278, -2.420129821023009331, 1.219334536740721564 ) ) ;
#15143 = CARTESIAN_POINT ( 'NONE',  ( -59.14665968485343228, 2.559517124687116230, -0.9190674295589398302 ) ) ;
#15144 = CARTESIAN_POINT ( 'NONE',  ( 51.13585994975462512, -0.9262448312163767961, 1.518514878530177192 ) ) ;
#15145 = ORIENTED_EDGE ( 'NONE', *, *, #14039, .F. ) ;
#15146 = DIRECTION ( 'NONE',  ( 1.000000000000000000, 1.047444401652940007E-14, 0.000000000000000000 ) ) ;
#15147 = CARTESIAN_POINT ( 'NONE',  ( 51.34893360928146677, -1.002183861492330630, -1.396106892655424980 ) ) ;
#15148 = CARTESIAN_POINT ( 'NONE',  ( 54.44703553260186624, 6.360744355421148022, -0.9750000000001826095 ) ) ;
#15149 = ORIENTED_EDGE ( 'NONE', *, *, #131, .T. ) ;
#15150 = EDGE_CURVE ( 'NONE', #12762, #29802, #18505, .T. ) ;
#15151 = DIRECTION ( 'NONE',  ( 1.000000000000000000, -0.000000000000000000, -1.047444401652940007E-14 ) ) ;
#15152 = ORIENTED_EDGE ( 'NONE', *, *, #10648, .T. ) ;
#15153 = EDGE_CURVE ( 'NONE', #22848, #31290, #3265, .T. ) ;
#15154 = CARTESIAN_POINT ( 'NONE',  ( 53.89553379148907908, 6.017104844469305824, 1.708828125785182728 ) ) ;
#15155 = CARTESIAN_POINT ( 'NONE',  ( -59.19376570361661294, -3.399999999999992362, 0.1704271383727704869 ) ) ;
#15157 = DIRECTION ( 'NONE',  ( 0.000000000000000000, 1.000000000000000000, 0.000000000000000000 ) ) ;
#15156 = CARTESIAN_POINT ( 'NONE',  ( 58.65000000000000568, 0.9941784314380587295, 1.590093208333443142 ) ) ;
#15158 = ORIENTED_EDGE ( 'NONE', *, *, #24286, .F. ) ;
#15159 = CARTESIAN_POINT ( 'NONE',  ( 58.75000000000003553, -1.972190280207336555, 0.1053114364790900953 ) ) ;
#15160 = PRODUCT_DEFINITION_FORMATION_WITH_SPECIFIED_SOURCE ( 'ANY', '', #8054, .NOT_KNOWN. ) ;
#15161 = CIRCLE ( 'NONE', #23768, 0.1499999999999998557 ) ;
#15162 = DIRECTION ( 'NONE',  ( 0.000000000000000000, -0.9996898646859344595, -0.02490330187381139398 ) ) ;
#15163 = AXIS2_PLACEMENT_3D ( 'NONE', #7314, #26323, #24263 ) ;
#15164 = ORIENTED_EDGE ( 'NONE', *, *, #2248, .T. ) ;
#15166 = CARTESIAN_POINT ( 'NONE',  ( -60.59999999999998010, -2.408745774756101188, -1.060314564156378037 ) ) ;
#15165 = DIRECTION ( 'NONE',  ( 1.000000000000000000, 1.786976680021908743E-16, -2.459562394685749209E-16 ) ) ;
#15167 = CARTESIAN_POINT ( 'NONE',  ( 48.00000000000001421, -4.003661535119149129, -1.269131321892086106 ) ) ;
#15168 = CARTESIAN_POINT ( 'NONE',  ( -57.43749999999997868, 3.238593381231845481, 2.874284765127021579 ) ) ;
#15169 = DIRECTION ( 'NONE',  ( 3.002035892788117459E-16, -0.9996898646859343485, -0.02490330187381124480 ) ) ;
#15170 = CARTESIAN_POINT ( 'NONE',  ( -54.39999999999996305, 1.400000000000021450, -3.363870538531680499 ) ) ;
#15171 = CIRCLE ( 'NONE', #22262, 1.000000000000000000 ) ;
#15172 = EDGE_CURVE ( 'NONE', #4801, #28026, #5348, .T. ) ;
#15173 = CARTESIAN_POINT ( 'NONE',  ( -61.39999999999998437, -2.624491116890564690, -0.6340712715164679159 ) ) ;
#15174 = CARTESIAN_POINT ( 'NONE',  ( 51.25000000000002842, -1.099999999999459410, -1.001327244211406953 ) ) ;
#15175 = CARTESIAN_POINT ( 'NONE',  ( -54.50952994616204705, -3.117691453623963938, -1.800000000000204770 ) ) ;
#15176 = DIRECTION ( 'NONE',  ( 1.000000000000000000, 0.000000000000000000, -1.047444401652940007E-14 ) ) ;
#15177 = ORIENTED_EDGE ( 'NONE', *, *, #9051, .T. ) ;
#15178 = CIRCLE ( 'NONE', #3040, 4.275000000000000355 ) ;
#15179 = CARTESIAN_POINT ( 'NONE',  ( 15.67083574136752944, 3.495540671458142068, 4.131527132740846042 ) ) ;
#15180 = B_SPLINE_CURVE_WITH_KNOTS ( 'NONE', 3,
 ( #5959, #19893, #5634, #10546, #8310, #10223 ),
 .UNSPECIFIED., .F., .F.,
 ( 4, 2, 4 ),
 ( 0.000000000000000000, 0.5000000000000000000, 1.000000000000000000 ),
 .UNSPECIFIED. ) ;
#15181 = DIRECTION ( 'NONE',  ( 0.000000000000000000, -5.942513678379226626E-16, -1.000000000000000000 ) ) ;
#15182 = FACE_OUTER_BOUND ( 'NONE', #3588, .T. ) ;
#15183 = CARTESIAN_POINT ( 'NONE',  ( -56.69702994616203284, -2.078460969082626342, -3.600000000000210587 ) ) ;
#15185 = AXIS2_PLACEMENT_3D ( 'NONE', #29238, #17063, #19597 ) ;
#15184 = CARTESIAN_POINT ( 'NONE',  ( 58.74154451056425330, -1.872697749442759463, -0.09314201707011884879 ) ) ;
#15186 = CARTESIAN_POINT ( 'NONE',  ( 48.50000000000178346, 1.391941090720882235, -3.849999999997240074 ) ) ;
#15187 = ORIENTED_EDGE ( 'NONE', *, *, #29061, .T. ) ;
#15188 = ADVANCED_FACE ( 'NONE', ( #902 ), #22547, .T. ) ;
#15189 = VERTEX_POINT ( 'NONE', #12755 ) ;
#15190 = UNCERTAINTY_MEASURE_WITH_UNIT (LENGTH_MEASURE( 1.000000000000000082E-05 ), #22823, 'distance_accuracy_value', 'NONE');
#15191 = EDGE_CURVE ( 'NONE', #20706, #333, #7375, .T. ) ;
#15192 = CARTESIAN_POINT ( 'NONE',  ( 50.45683212279338647, -1.211455355144520185, 3.917539841352834173 ) ) ;
#15194 = FACE_OUTER_BOUND ( 'NONE', #6531, .T. ) ;
#15193 = CARTESIAN_POINT ( 'NONE',  ( 15.95705409078465209, -3.646557212684145899, -3.995389720703518055 ) ) ;
#15195 = EDGE_CURVE ( 'NONE', #11984, #16075, #789, .T. ) ;
#15196 = ORIENTED_EDGE ( 'NONE', *, *, #22395, .T. ) ;
#15197 = ORIENTED_EDGE ( 'NONE', *, *, #8062, .T. ) ;
#15198 = CARTESIAN_POINT ( 'NONE',  ( -59.26905989232412253, 2.944486372867082480, 1.699999999999818101 ) ) ;
#15199 = CARTESIAN_POINT ( 'NONE',  ( 51.59739104186226655, 1.010292945603183723, 1.272765950230259513 ) ) ;
#15200 = ORIENTED_EDGE ( 'NONE', *, *, #16045, .F. ) ;
#15202 = CARTESIAN_POINT ( 'NONE',  ( 51.80000000000001847, -4.131056160354152240, 1.099999999999999867 ) ) ;
#15201 = CARTESIAN_POINT ( 'NONE',  ( -56.13452994616205416, -3.117691453623976816, 1.799999999999788436 ) ) ;
#15203 = CARTESIAN_POINT ( 'NONE',  ( 50.36033030378882103, 1.282137971188145320, 3.869545987293864897 ) ) ;
#15204 = LINE ( 'NONE', #10458, #14248 ) ;
#15205 = DIRECTION ( 'NONE',  ( 1.000000000000000000, 0.000000000000000000, 0.000000000000000000 ) ) ;
#15206 = ADVANCED_FACE ( 'NONE', ( #17527 ), #25270, .T. ) ;
#15207 = CARTESIAN_POINT ( 'NONE',  ( -59.29999999999996874, -3.436256089820699522, -1.251858815887733289 ) ) ;
#15208 =( LENGTH_UNIT ( ) NAMED_UNIT ( * ) SI_UNIT ( .MILLI., .METRE. ) );
#15209 = ORIENTED_EDGE ( 'NONE', *, *, #10653, .F. ) ;
#15210 = AXIS2_PLACEMENT_3D ( 'NONE', #28176, #27582, #30533 ) ;
#15211 = CARTESIAN_POINT ( 'NONE',  ( -56.19702994616206837, -2.078460969082657872, 3.599999999999791811 ) ) ;
#15212 = CARTESIAN_POINT ( 'NONE',  ( 51.46757676178951613, 4.376162276235350035, -1.550000000000179012 ) ) ;
#15213 = CARTESIAN_POINT ( 'NONE',  ( 48.50000000000002132, -1.391941090707492057, -3.850000000000022293 ) ) ;
#15214 = CARTESIAN_POINT ( 'NONE',  ( 15.30042582489634384, 1.123735543663135550, 5.289358694936654004 ) ) ;
#15215 = EDGE_CURVE ( 'NONE', #29380, #2983, #9420, .T. ) ;
#15216 = CARTESIAN_POINT ( 'NONE',  ( 51.72661555197463912, -4.179189466084497262, -0.9999999999999991118 ) ) ;
#15217 = DIRECTION ( 'NONE',  ( -2.117927888850090838E-16, 0.02490330187381123786, -0.9996898646859343485 ) ) ;
#15219 = DIRECTION ( 'NONE',  ( 1.000000000000000000, 1.047444401652940007E-14, 0.000000000000000000 ) ) ;
#15218 = CARTESIAN_POINT ( 'NONE',  ( -56.90400635094607651, -3.399999999999988809, -0.9110272542660338146 ) ) ;
#15220 =( BOUNDED_SURFACE ( )  B_SPLINE_SURFACE ( 3, 2, ( 
 ( #30650, #6916, #18482 ),
 ( #26226, #9290, #21343 ),
 ( #4369, #16105, #7075 ),
 ( #18953, #23236, #25586 ),
 ( #25754, #23709, #1999 ),
 ( #28599, #4060, #16581 ),
 ( #4532, #21489, #23536 ),
 ( #23385, #11509, #14183 ),
 ( #31122, #9454, #3904 ),
 ( #1668, #1524, #23858 ),
 ( #11185, #2151, #8963 ),
 ( #11327, #21013, #18642 ),
 ( #16257, #25904, #4209 ),
 ( #1836, #5150, #21661 ),
 ( #19740, #14500, #17054 ),
 ( #2628, #9618, #14800 ) ),
 .UNSPECIFIED., .F., .F., .F. ) 
 B_SPLINE_SURFACE_WITH_KNOTS ( ( 4, 2, 2, 2, 2, 2, 2, 4 ),
 ( 3, 3 ),
 ( 0.001780502285214235472, 0.002558945925323760293, 0.002753556835351141444, 0.002948167745378522595, 0.003337389565433285330, 0.003726611385488048066, 0.004115833205542810368, 0.004894276845652334972 ),
 ( 0.000000000000000000, 1.000000000000000000 ),
 .UNSPECIFIED. ) 
 GEOMETRIC_REPRESENTATION_ITEM ( )  RATIONAL_B_SPLINE_SURFACE ( (
 ( 1.000000000000000000, 0.9418517008537247159, 1.000000000000000000),
 ( 1.000000000000000000, 0.9417987965884988544, 1.000000000000000000),
 ( 1.000000000000000000, 0.9418198861734239369, 1.000000000000000000),
 ( 1.000000000000000000, 0.9434060303845547280, 1.000000000000000000),
 ( 1.000000000000000000, 0.9437939819948095721, 1.000000000000000000),
 ( 1.000000000000000000, 0.9445989566712877927, 1.000000000000000000),
 ( 1.000000000000000000, 0.9450169930049913125, 1.000000000000000000),
 ( 1.000000000000000000, 0.9461610507673479109, 1.000000000000000000),
 ( 1.000000000000000000, 0.9467217966425561793, 1.000000000000000000),
 ( 1.000000000000000000, 0.9467345476126033388, 1.000000000000000000),
 ( 1.000000000000000000, 0.9461964028053023723, 1.000000000000000000),
 ( 1.000000000000000000, 0.9446801822473783750, 1.000000000000000000),
 ( 1.000000000000000000, 0.9437582546536112948, 1.000000000000000000),
 ( 1.000000000000000000, 0.9418129560296572000, 1.000000000000000000),
 ( 1.000000000000000000, 0.9418016889776811285, 1.000000000000000000),
 ( 1.000000000000000000, 0.9418517008537240498, 1.000000000000000000) ) ) 
 REPRESENTATION_ITEM ( '' )  SURFACE ( )  );
#15221 = CIRCLE ( 'NONE', #19297, 1.949999999999999956 ) ;
#15222 = CARTESIAN_POINT ( 'NONE',  ( 51.21562071718019382, 0.9844478935114779894, -1.555267182539685100 ) ) ;
#15223 = CARTESIAN_POINT ( 'NONE',  ( 48.41298237836545582, 1.088467210617599656, -3.899823238510140122 ) ) ;
#15225 = LINE ( 'NONE', #17153, #27609 ) ;
#15224 = CARTESIAN_POINT ( 'NONE',  ( 17.21035195517768557, -2.471857751707525626E-15, 0.000000000000000000 ) ) ;
#15226 = ORIENTED_EDGE ( 'NONE', *, *, #31299, .F. ) ;
#15227 = EDGE_CURVE ( 'NONE', #9733, #10205, #6374, .T. ) ;
#15228 = CARTESIAN_POINT ( 'NONE',  ( 50.29999999999825633, -1.391941090720833607, -3.849999999997240074 ) ) ;
#15229 = EDGE_CURVE ( 'NONE', #560, #4498, #24646, .T. ) ;
#15230 = DIRECTION ( 'NONE',  ( 1.000000000000000000, 3.054025858079668409E-16, -2.042474015755241579E-16 ) ) ;
#15231 = CARTESIAN_POINT ( 'NONE',  ( 15.39414421509792419, 3.291455042465473824, -4.036171416105450049 ) ) ;
#15233 = ADVANCED_FACE ( 'NONE', ( #27178 ), #22941, .T. ) ;
#15232 = CARTESIAN_POINT ( 'NONE',  ( -58.09599364905385244, 3.400000000000014122, -0.9110272542660006190 ) ) ;
#15234 = VERTEX_POINT ( 'NONE', #18787 ) ;
#15235 = CARTESIAN_POINT ( 'NONE',  ( 51.80000000000002558, 0.2793919678926817807, 0.9601771338022603297 ) ) ;
#15236 = CARTESIAN_POINT ( 'NONE',  ( -60.63087243001902493, -2.460428303538280570, -1.102619274812461025 ) ) ;
#15237 = ORIENTED_EDGE ( 'NONE', *, *, #10891, .T. ) ;
#15238 = FACE_OUTER_BOUND ( 'NONE', #2703, .T. ) ;
#15239 = ORIENTED_EDGE ( 'NONE', *, *, #501, .F. ) ;
#15240 = ORIENTED_EDGE ( 'NONE', *, *, #27445, .F. ) ;
#15241 = DIRECTION ( 'NONE',  ( 0.9993908270190957621, -0.03489949670250097613, -3.491481338843133355E-15 ) ) ;
#15242 = EDGE_LOOP ( 'NONE', ( #21147, #15853, #372, #13414 ) ) ;
#15243 =( NAMED_UNIT ( * ) PLANE_ANGLE_UNIT ( ) SI_UNIT ( $, .RADIAN. ) );
#15244 = CARTESIAN_POINT ( 'NONE',  ( 60.75000000000002842, -0.6499999999993638644, 1.489337100860647967 ) ) ;
#15245 = CARTESIAN_POINT ( 'NONE',  ( -59.57202994616203995, 2.078460969082674747, -3.600000000000202593 ) ) ;
#15246 = EDGE_LOOP ( 'NONE', ( #2899, #23391, #16407, #1625 ) ) ;
#15247 = CARTESIAN_POINT ( 'NONE',  ( 54.47118315602192951, -0.0009370910484917797413, 4.346120462634435633 ) ) ;
#15248 = ORIENTED_EDGE ( 'NONE', *, *, #7228, .T. ) ;
#15249 = LINE ( 'NONE', #5125, #26339 ) ;
#15250 = CARTESIAN_POINT ( 'NONE',  ( 22.09542497196702371, 7.445411295444298361, 1.949999999999922240 ) ) ;
#15251 = EDGE_LOOP ( 'NONE', ( #20034, #25356, #24057, #31212 ) ) ;
#15252 = CIRCLE ( 'NONE', #2093, 0.8749999999999990008 ) ;
#15253 = DIRECTION ( 'NONE',  ( -2.581436205204234499E-16, 0.9796124928211140670, 0.2008964009354147762 ) ) ;
#15254 = DIRECTION ( 'NONE',  ( -1.000000000000000000, -3.053848253006669023E-16, 2.042510438544995415E-16 ) ) ;
#15255 = CARTESIAN_POINT ( 'NONE',  ( 50.25000000000003553, -1.323060376181184772, -1.499837071478052453 ) ) ;
#15256 = ADVANCED_FACE ( 'NONE', ( #15771 ), #23697, .F. ) ;
#15257 = CARTESIAN_POINT ( 'NONE',  ( -54.39999999999997016, -1.514093959731525274, -3.183260039818592624 ) ) ;
#15258 =( BOUNDED_CURVE ( )  B_SPLINE_CURVE ( 2, ( #2808, #22305, #17546, #3128, #12461, #5816, #20088, #29726, #5332 ),
 .UNSPECIFIED., .F., .T. ) 
 B_SPLINE_CURVE_WITH_KNOTS ( ( 3, 2, 2, 2, 3 ),
 ( 0.4722222222222222654, 0.4814814814814814548, 0.5000000000000000000, 0.5185185185185184897, 0.5277777777777777901 ),
 .UNSPECIFIED. ) 
 CURVE ( )  GEOMETRIC_REPRESENTATION_ITEM ( )  RATIONAL_B_SPLINE_CURVE ( ( 0.9330127018922194093, 0.9330127018922197424, 1.000000000000000000, 0.8660254037844387076, 1.000000000000000000, 0.8660254037844387076, 1.000000000000000000, 0.9330127018922194093, 0.9330127018922194093 ) ) 
 REPRESENTATION_ITEM ( '' )  );
#15259 = EDGE_CURVE ( 'NONE', #6022, #17883, #21040, .T. ) ;
#15261 = DIRECTION ( 'NONE',  ( 0.000000000000000000, 0.000000000000000000, 1.000000000000000000 ) ) ;
#15260 = DIRECTION ( 'NONE',  ( 0.000000000000000000, 0.000000000000000000, -1.000000000000000000 ) ) ;
#15262 = DIRECTION ( 'NONE',  ( 0.000000000000000000, -1.000000000000000000, -3.491481338843134933E-15 ) ) ;
#15263 = DIRECTION ( 'NONE',  ( -3.002035892788117459E-16, 0.9996898646859344595, 0.02490330187381124133 ) ) ;
#15264 = CARTESIAN_POINT ( 'NONE',  ( 58.66122797211878748, 1.337438849765252069, -1.314214529126763509 ) ) ;
#15265 = CARTESIAN_POINT ( 'NONE',  ( 53.46805841003781978, 8.044896776089471402, -2.050000000000185452 ) ) ;
#15266 = ORIENTED_EDGE ( 'NONE', *, *, #5760, .T. ) ;
#15267 = CARTESIAN_POINT ( 'NONE',  ( 53.38897031725308295, 5.061772353509735645, 1.621051207520878723 ) ) ;
#15268 = AXIS2_PLACEMENT_3D ( 'NONE', #9336, #4104, #4253 ) ;
#15269 = EDGE_LOOP ( 'NONE', ( #13879, #17315, #3737, #14192 ) ) ;
#15270 = AXIS2_PLACEMENT_3D ( 'NONE', #28013, #799, #29773 ) ;
#15271 = VERTEX_POINT ( 'NONE', #30328 ) ;
#15272 = CARTESIAN_POINT ( 'NONE',  ( 50.25000000000003553, -1.470078920827295965, -1.470078920827526892 ) ) ;
#15273 = CARTESIAN_POINT ( 'NONE',  ( -58.86042740578360366, 3.725040285533370632, -1.239922660687675648 ) ) ;
#15275 = CARTESIAN_POINT ( 'NONE',  ( -61.35738992240673184, -2.589110738181390037, 0.6770092922617376718 ) ) ;
#15274 = FACE_OUTER_BOUND ( 'NONE', #30967, .T. ) ;
#15276 = VERTEX_POINT ( 'NONE', #4353 ) ;
#15277 = ORIENTED_EDGE ( 'NONE', *, *, #10566, .T. ) ;
#15278 = CARTESIAN_POINT ( 'NONE',  ( 53.94314916079858335, 6.379172879799750007, -1.774223561664970861 ) ) ;
#15279 = EDGE_LOOP ( 'NONE', ( #28983, #17778, #25879, #10277 ) ) ;
#15280 = CARTESIAN_POINT ( 'NONE',  ( 51.40674769956036272, 0.9873535814804794697, -1.422142864483640912 ) ) ;
#15281 = VERTEX_POINT ( 'NONE', #21331 ) ;
#15282 = CARTESIAN_POINT ( 'NONE',  ( 29.99460041311474612, 6.535150002936296332, -2.049999999999972733 ) ) ;
#15283 = CARTESIAN_POINT ( 'NONE',  ( -44.49999999999999289, -1.499999999999999556, -3.300094695611020867 ) ) ;
#15284 = CARTESIAN_POINT ( 'NONE',  ( -58.84599364905385954, 3.400000000000015010, -0.9110272542660019512 ) ) ;
#15285 = VERTEX_POINT ( 'NONE', #25892 ) ;
#15286 = CARTESIAN_POINT ( 'NONE',  ( 15.56274145962692401, -4.735538777079653983, -2.618062770413819518 ) ) ;
#15287 = CARTESIAN_POINT ( 'NONE',  ( -60.83155989232411542, 3.925981830489463142, -2.015755723410760408E-13 ) ) ;
#15288 = CARTESIAN_POINT ( 'NONE',  ( 52.72145679358933279, 4.007061708474140893, -2.050000000000183675 ) ) ;
#15289 = EDGE_CURVE ( 'NONE', #22328, #8527, #23222, .T. ) ;
#15290 = CARTESIAN_POINT ( 'NONE',  ( 47.12910489933606328, -3.772469189071208095, -1.610667359469886595 ) ) ;
#15291 = EDGE_CURVE ( 'NONE', #11104, #11593, #19522, .T. ) ;
#15292 = CARTESIAN_POINT ( 'NONE',  ( -59.09999999999997300, 8.366749974758448157E-15, -2.099585467500611340E-13 ) ) ;
#15293 = EDGE_CURVE ( 'NONE', #29801, #8009, #1819, .T. ) ;
#15294 = DIRECTION ( 'NONE',  ( -1.000000000000000000, 0.000000000000000000, 1.047444401652940007E-14 ) ) ;
#15295 = CARTESIAN_POINT ( 'NONE',  ( 58.65000000000004121, -1.760622601995821990, 0.8948927608039443093 ) ) ;
#15296 = DIRECTION ( 'NONE',  ( -2.095850865446309212E-30, -1.000000000000000000, -2.891205793294679411E-15 ) ) ;
#15297 = CARTESIAN_POINT ( 'NONE',  ( -62.07183734345855441, -2.637794457623054534, 0.1946209358647623400 ) ) ;
#15298 = CARTESIAN_POINT ( 'NONE',  ( 50.31971926781693583, 8.252744006147214151, -2.050000000000174794 ) ) ;
#15299 = AXIS2_PLACEMENT_3D ( 'NONE', #18256, #31012, #22999 ) ;
#15300 = VERTEX_POINT ( 'NONE', #11654 ) ;
#15301 = CARTESIAN_POINT ( 'NONE',  ( -59.29999999999998295, -1.825148624098436478, 2.913569361162840377 ) ) ;
#15302 = CARTESIAN_POINT ( 'NONE',  ( -36.11780688638066295, -2.199885882963843908, -4.939696253589922925 ) ) ;
#15303 = CARTESIAN_POINT ( 'NONE',  ( 54.29334943003577507, 6.002962681774890008, 2.049999999999807532 ) ) ;
#15304 = EDGE_LOOP ( 'NONE', ( #22660, #15800, #6881, #17672 ) ) ;
#15305 = EDGE_CURVE ( 'NONE', #15675, #1692, #6400, .T. ) ;
#15306 = FACE_OUTER_BOUND ( 'NONE', #25401, .T. ) ;
#15307 = VERTEX_POINT ( 'NONE', #8778 ) ;
#15308 = CARTESIAN_POINT ( 'NONE',  ( 60.75000000000001421, 0.7500000000006363798, 1.718465885608440269 ) ) ;
#15309 = CARTESIAN_POINT ( 'NONE',  ( -36.04581030752631676, -5.340403874104872273, 0.9205822090003401570 ) ) ;
#15311 = CARTESIAN_POINT ( 'NONE',  ( 51.67650754010888647, -3.859221392886597712, -1.645001822843487949 ) ) ;
#15310 = CARTESIAN_POINT ( 'NONE',  ( 51.70000000000003126, -4.020776289669855785, 2.234582293948397691 ) ) ;
#15312 = ORIENTED_EDGE ( 'NONE', *, *, #6539, .F. ) ;
#15313 = DIRECTION ( 'NONE',  ( 0.7542528389311653481, 0.5142632992712595774, -0.4082106245394850341 ) ) ;
#15314 = LINE ( 'NONE', #24959, #6960 ) ;
#15315 = ORIENTED_EDGE ( 'NONE', *, *, #19827, .T. ) ;
#15317 = CARTESIAN_POINT ( 'NONE',  ( 41.48619405471883681, -151.3359592902622239, -2.050000000000163691 ) ) ;
#15316 = CARTESIAN_POINT ( 'NONE',  ( 52.54185214673768911, 4.030541857796934302, 2.045987466503689234 ) ) ;
#15318 = ORIENTED_EDGE ( 'NONE', *, *, #15801, .T. ) ;
#15319 = ORIENTED_EDGE ( 'NONE', *, *, #6941, .F. ) ;
#15320 = CARTESIAN_POINT ( 'NONE',  ( 53.94245690748179811, 6.674762429336770886, -1.915449902665558701 ) ) ;
#15321 = CARTESIAN_POINT ( 'NONE',  ( 56.96065904101961763, -0.7273651001630837554, 1.755300599839360265 ) ) ;
#15322 = DIRECTION ( 'NONE',  ( 0.000000000000000000, 0.9996898646859343485, 0.02490330187381123786 ) ) ;
#15323 = CARTESIAN_POINT ( 'NONE',  ( -54.49999999999997158, -3.743960284996337151, -0.06497723394329793511 ) ) ;
#15324 = DIRECTION ( 'NONE',  ( -2.964772755551650383E-16, -0.9875000000000001554, 0.1576190026614809614 ) ) ;
#15325 = CARTESIAN_POINT ( 'NONE',  ( 48.50000000000002132, -4.899999999999999467, 3.950000000000022826 ) ) ;
#15326 = ORIENTED_EDGE ( 'NONE', *, *, #20270, .T. ) ;
#15327 = ADVANCED_FACE ( 'NONE', ( #9121 ), #10931, .T. ) ;
#15328 = ADVANCED_FACE ( 'NONE', ( #3890 ), #20069, .F. ) ;
#15329 = CARTESIAN_POINT ( 'NONE',  ( 15.57907767661756004, 2.743848709681572018, 4.666930520580628183 ) ) ;
#15330 = CARTESIAN_POINT ( 'NONE',  ( -55.36042740578360366, -2.936324665650197563, -2.606018187048502632 ) ) ;
#15331 = LINE ( 'NONE', #30507, #4828 ) ;
#15332 = CARTESIAN_POINT ( 'NONE',  ( -59.00952994616203284, -3.117691453623959053, -1.800000000000228750 ) ) ;
#15333 = DIRECTION ( 'NONE',  ( -0.7542528389311761172, 0.5142632992712440343, 0.4082106245394852007 ) ) ;
#15334 = CARTESIAN_POINT ( 'NONE',  ( 48.42155979508061137, 1.181909706220234613, -3.885998080850100234 ) ) ;
#15335 = ORIENTED_EDGE ( 'NONE', *, *, #5679, .T. ) ;
#15336 = ADVANCED_FACE ( 'NONE', ( #30805 ), #24106, .T. ) ;
#15337 = DIRECTION ( 'NONE',  ( 0.000000000000000000, 1.000000000000000000, 0.000000000000000000 ) ) ;
#15338 = VERTEX_POINT ( 'NONE', #26045 ) ;
#15339 = CARTESIAN_POINT ( 'NONE',  ( 50.36673905152862574, -1.398826622412641996, 3.854114288381605302 ) ) ;
#15340 = VECTOR ( 'NONE', #29133, 1000.000000000000000 ) ;
#15342 = CARTESIAN_POINT ( 'NONE',  ( 58.75000000000003553, -1.320164791810108484, 1.457351493770938200 ) ) ;
#15341 = DIRECTION ( 'NONE',  ( 0.000000000000000000, 0.000000000000000000, -1.000000000000000000 ) ) ;
#15343 = CIRCLE ( 'NONE', #16879, 0.2499999999999997780 ) ;
#15344 = ORIENTED_EDGE ( 'NONE', *, *, #16203, .F. ) ;
#15345 = ORIENTED_EDGE ( 'NONE', *, *, #22754, .F. ) ;
#15346 = CARTESIAN_POINT ( 'NONE',  ( -61.34999999999997300, -2.617575446388284099, 0.6620413751912884726 ) ) ;
#15347 = CARTESIAN_POINT ( 'NONE',  ( 24.57460841532290630, 5.893272594507614315, -1.425000000000085754 ) ) ;
#15348 = ORIENTED_EDGE ( 'NONE', *, *, #7930, .T. ) ;
#15350 = CARTESIAN_POINT ( 'NONE',  ( 51.73054293450984886, -4.177413309949346676, 1.004109922956872625 ) ) ;
#15349 = CARTESIAN_POINT ( 'NONE',  ( -58.75952994616203284, 3.117691453623994580, -1.800000000000195000 ) ) ;
#15351 = ADVANCED_FACE ( 'NONE', ( #18942 ), #28585, .T. ) ;
#15352 = DIRECTION ( 'NONE',  ( 0.000000000000000000, 0.000000000000000000, 1.000000000000000000 ) ) ;
#15353 = SHAPE_DEFINITION_REPRESENTATION ( #25788, #7047 ) ;
#15354 = CARTESIAN_POINT ( 'NONE',  ( -59.29999999999996163, -3.297590540183683139, 1.214612339250627171 ) ) ;
#15355 =( LENGTH_UNIT ( ) NAMED_UNIT ( * ) SI_UNIT ( .MILLI., .METRE. ) );
#15356 = ADVANCED_BREP_SHAPE_REPRESENTATION ( '', ( #25800, #9018 ), #12557 ) ;
#15357 = VERTEX_POINT ( 'NONE', #23058 ) ;
#15358 = ADVANCED_FACE ( 'NONE', ( #11025 ), #1474, .T. ) ;
#15359 = FACE_OUTER_BOUND ( 'NONE', #29362, .T. ) ;
#15360 = CARTESIAN_POINT ( 'NONE',  ( 53.90340377275677497, 6.895264694548083995, -1.787725782035514355 ) ) ;
#15361 = CARTESIAN_POINT ( 'NONE',  ( 48.41306782696076993, -1.296871156637267486, -3.889656364559859192 ) ) ;
#15362 = AXIS2_PLACEMENT_3D ( 'NONE', #23379, #13698, #8332 ) ;
#15363 = CARTESIAN_POINT ( 'NONE',  ( 15.76675455518219593, 0.1030603059132040172, 5.407440145940146436 ) ) ;
#15364 = DIRECTION ( 'NONE',  ( 1.000000000000000000, 2.586136946169074517E-16, -0.000000000000000000 ) ) ;
#15366 = CARTESIAN_POINT ( 'NONE',  ( 58.72427158855730056, -1.822388627306549047, -0.4415141953928994889 ) ) ;
#15365 = CARTESIAN_POINT ( 'NONE',  ( 30.89639353666900945, 7.705332861838119385, -1.425000000000107292 ) ) ;
#15367 = PRODUCT ( 'Eraser', 'Eraser', '', ( #28337 ) ) ;
#15368 = AXIS2_PLACEMENT_3D ( 'NONE', #22294, #1315, #30292 ) ;
#15369 = FACE_OUTER_BOUND ( 'NONE', #21926, .T. ) ;
#15370 = CARTESIAN_POINT ( 'NONE',  ( 52.28357475172138891, 3.966531851984107959, -2.045538984187684317 ) ) ;
#15372 = CARTESIAN_POINT ( 'NONE',  ( 51.76665129121496989, 4.175715153428437354, -1.929612129901383977 ) ) ;
#15371 = CARTESIAN_POINT ( 'NONE',  ( 58.66133336607634163, 1.802692578419500258, -0.5167488000321581731 ) ) ;
#15373 = ORIENTED_EDGE ( 'NONE', *, *, #31267, .T. ) ;
#15374 = EDGE_CURVE ( 'NONE', #6165, #17785, #4341, .T. ) ;
#15375 = DIRECTION ( 'NONE',  ( -1.000000000000000000, -0.000000000000000000, -0.000000000000000000 ) ) ;
#15376 = CARTESIAN_POINT ( 'NONE',  ( 58.64999999999992752, -1.760622601995799119, -0.8948927608040211368 ) ) ;
#15378 = CARTESIAN_POINT ( 'NONE',  ( 51.70000000000002416, 3.851905453475163110, 1.404572667215161053 ) ) ;
#15377 = CARTESIAN_POINT ( 'NONE',  ( 47.10000000000002274, 6.982261990806648555E-14, -1.632474749424821370E-13 ) ) ;
#15379 = CARTESIAN_POINT ( 'NONE',  ( 51.70000000000000995, 2.478823385132571090E-14, -4.100000000000172840 ) ) ;
#15380 = ORIENTED_EDGE ( 'NONE', *, *, #2618, .F. ) ;
#15381 = CARTESIAN_POINT ( 'NONE',  ( 60.75000000000002842, -0.4999999999993638977, 1.718465885608440047 ) ) ;
#15382 = CARTESIAN_POINT ( 'NONE',  ( 30.31473038485998828, 6.776227631128587170, -1.550000000000105294 ) ) ;
#15383 = AXIS2_PLACEMENT_3D ( 'NONE', #15170, #22631, #931 ) ;
#15384 = ORIENTED_EDGE ( 'NONE', *, *, #30008, .T. ) ;
#15385 = FACE_OUTER_BOUND ( 'NONE', #16292, .T. ) ;
#15386 = ORIENTED_EDGE ( 'NONE', *, *, #6553, .F. ) ;
#15387 = ADVANCED_FACE ( 'NONE', ( #12262 ), #30143, .F. ) ;
#15388 = ORIENTED_EDGE ( 'NONE', *, *, #3145, .T. ) ;
#15389 = LINE ( 'NONE', #14915, #26033 ) ;
#15390 = CARTESIAN_POINT ( 'NONE',  ( 46.90000000000001279, 1.734723475976807094E-15, 0.000000000000000000 ) ) ;
#15391 = ORIENTED_EDGE ( 'NONE', *, *, #25772, .F. ) ;
#15392 = CARTESIAN_POINT ( 'NONE',  ( 51.34430644926990084, 1.002608958138277773, -1.395204572094386641 ) ) ;
#15393 = CARTESIAN_POINT ( 'NONE',  ( -59.32202994616204705, 2.078460969082646770, 3.599999999999797140 ) ) ;
#15394 = ORIENTED_EDGE ( 'NONE', *, *, #602, .T. ) ;
#15395 = FACE_OUTER_BOUND ( 'NONE', #21693, .T. ) ;
#15396 = VECTOR ( 'NONE', #679, 1000.000000000000000 ) ;
#15397 = CARTESIAN_POINT ( 'NONE',  ( 57.00000000000001421, 0.7500000000000000000, -1.778341924377873751 ) ) ;
#15398 = CARTESIAN_POINT ( 'NONE',  ( 22.40865038670895260, 7.071719536792469896, 2.049999999999921663 ) ) ;
#15399 = ORIENTED_EDGE ( 'NONE', *, *, #5976, .F. ) ;
#15400 = ADVANCED_FACE ( 'NONE', ( #87 ), #29140, .F. ) ;
#15401 = CARTESIAN_POINT ( 'NONE',  ( -57.06249999999997868, -1.962990915244731793, 3.399999999999788969 ) ) ;
#15402 = ADVANCED_FACE ( 'NONE', ( #7529 ), #19728, .T. ) ;
#15403 =( BOUNDED_CURVE ( )  B_SPLINE_CURVE ( 2, ( #17511, #12591, #26997, #8012, #29849, #22420, #5303, #22583, #14962 ),
 .UNSPECIFIED., .F., .T. ) 
 B_SPLINE_CURVE_WITH_KNOTS ( ( 3, 2, 2, 2, 3 ),
 ( 0.4166666666666666852, 0.4259259259259259300, 0.4444444444444444198, 0.4629629629629629650, 0.4722222222222222654 ),
 .UNSPECIFIED. ) 
 CURVE ( )  GEOMETRIC_REPRESENTATION_ITEM ( )  RATIONAL_B_SPLINE_CURVE ( ( 0.9330127018922194093, 0.9330127018922195203, 1.000000000000000000, 0.8660254037844387076, 1.000000000000000000, 0.8660254037844387076, 1.000000000000000000, 0.9330127018922189652, 0.9330127018922194093 ) ) 
 REPRESENTATION_ITEM ( '' )  );
#15404 = CYLINDRICAL_SURFACE ( 'NONE', #23602, 0.04999999999999991257 ) ;
#15405 = CARTESIAN_POINT ( 'NONE',  ( 69.20000000000005969, -0.4500000000000000111, 1.988246715072633508 ) ) ;
#15407 = ADVANCED_FACE ( 'NONE', ( #29214 ), #25979, .T. ) ;
#15406 = DIRECTION ( 'NONE',  ( 0.000000000000000000, 0.000000000000000000, -1.000000000000000000 ) ) ;
#15408 = VECTOR ( 'NONE', #18285, 1000.000000000000000 ) ;
#15409 = AXIS2_PLACEMENT_3D ( 'NONE', #30005, #27949, #30326 ) ;
#15410 = CARTESIAN_POINT ( 'NONE',  ( -59.19999999999997442, 8.366749974758448157E-15, -2.103076948839454410E-13 ) ) ;
#15412 = DIRECTION ( 'NONE',  ( 0.000000000000000000, 0.2008964009354144709, -0.9796124928211140670 ) ) ;
#15411 = CARTESIAN_POINT ( 'NONE',  ( 51.80000000000002558, 6.475000000000062705, 2.049999999999819522 ) ) ;
#15413 = AXIS2_PLACEMENT_3D ( 'NONE', #20249, #15313, #10251 ) ;
#15414 = FACE_OUTER_BOUND ( 'NONE', #11106, .T. ) ;
#15415 = CARTESIAN_POINT ( 'NONE',  ( -59.29999999999997584, 2.330309927981285032E-15, 4.253626757584724400E-16 ) ) ;
#15416 = DIRECTION ( 'NONE',  ( 0.000000000000000000, 0.000000000000000000, 1.000000000000000000 ) ) ;
#15417 = DIRECTION ( 'NONE',  ( -3.489354422748178582E-15, 1.218509414717996338E-16, -1.000000000000000000 ) ) ;
#15418 = EDGE_CURVE ( 'NONE', #10721, #1900, #28627, .T. ) ;
#15419 = CARTESIAN_POINT ( 'NONE',  ( 53.81457038914302871, 5.799118248596165870, 1.689328270749656191 ) ) ;
#15420 = ORIENTED_EDGE ( 'NONE', *, *, #23358, .F. ) ;
#15421 = DIRECTION ( 'NONE',  ( 0.000000000000000000, 0.000000000000000000, 1.000000000000000000 ) ) ;
#15422 = VERTEX_POINT ( 'NONE', #29974 ) ;
#15423 = DIRECTION ( 'NONE',  ( 1.000000000000000000, -0.000000000000000000, -3.491481338843133355E-15 ) ) ;
#15424 = CARTESIAN_POINT ( 'NONE',  ( -58.54792740578360366, -2.256877952708263635, 2.542931754211924744 ) ) ;
#15426 = CARTESIAN_POINT ( 'NONE',  ( -61.39999999999998437, -2.604492677689918878, 0.7117709546332967596 ) ) ;
#15425 = CARTESIAN_POINT ( 'NONE',  ( -56.49999999999997868, 2.944486372867092250, 1.699999999999810774 ) ) ;
#15427 = ORIENTED_EDGE ( 'NONE', *, *, #8144, .F. ) ;
#15428 = EDGE_CURVE ( 'NONE', #12125, #28052, #8597, .T. ) ;
#15429 = ORIENTED_EDGE ( 'NONE', *, *, #20376, .F. ) ;
#15430 = CIRCLE ( 'NONE', #30082, 1.899999999999999911 ) ;
#15431 = CARTESIAN_POINT ( 'NONE',  ( 54.26434950415730896, 6.004763229855418771, -2.050000000000188560 ) ) ;
#15432 = ORIENTED_EDGE ( 'NONE', *, *, #4292, .F. ) ;
#15433 = CARTESIAN_POINT ( 'NONE',  ( 51.25000000000001421, 0.9938153758931693726, -1.589954715908409755 ) ) ;
#15434 = ORIENTED_EDGE ( 'NONE', *, *, #12487, .T. ) ;
#15435 = CARTESIAN_POINT ( 'NONE',  ( 23.33428888190753980, 6.022557145544042534, -1.950000000000082112 ) ) ;
#15436 = EDGE_CURVE ( 'NONE', #16145, #2467, #20572, .T. ) ;
#15437 = ORIENTED_EDGE ( 'NONE', *, *, #23209, .F. ) ;
#15438 = CARTESIAN_POINT ( 'NONE',  ( 68.00000000000002842, 1.401298464324817071E-42, -7.122621931239993559E-13 ) ) ;
#15439 = CARTESIAN_POINT ( 'NONE',  ( -61.34999999999997300, -2.551764585593653489, 0.6636807913650824009 ) ) ;
#15440 = AXIS2_PLACEMENT_3D ( 'NONE', #18300, #13528, #5347 ) ;
#15441 =( BOUNDED_SURFACE ( )  B_SPLINE_SURFACE ( 3, 2, ( 
 ( #8904, #13962, #4159 ),
 ( #23662, #9242, #26179 ),
 ( #13500, #1475, #20808 ),
 ( #30439, #16358, #18429 ) ),
 .UNSPECIFIED., .F., .F., .F. ) 
 B_SPLINE_SURFACE_WITH_KNOTS ( ( 4, 4 ),
 ( 3, 3 ),
 ( 6.470519842244164266E-05, 0.0002246728259156070709 ),
 ( 0.000000000000000000, 1.000000000000000000 ),
 .UNSPECIFIED. ) 
 GEOMETRIC_REPRESENTATION_ITEM ( )  RATIONAL_B_SPLINE_SURFACE ( (
 ( 1.000000000000000000, 0.5857791861290068125, 1.000000000000000000),
 ( 1.000000000000000000, 0.5849685391560944803, 1.000000000000000000),
 ( 1.000000000000000000, 0.6585504321673580908, 1.000000000000000000),
 ( 1.000000000000000000, 0.7071067811864985009, 1.000000000000000000) ) ) 
 REPRESENTATION_ITEM ( '' )  SURFACE ( )  );
#15442 = CARTESIAN_POINT ( 'NONE',  ( 15.74652664997072549, -5.205077242910900459, -1.471673150993815682 ) ) ;
#15443 = AXIS2_PLACEMENT_3D ( 'NONE', #4175, #20826, #13671 ) ;
#15444 = EDGE_CURVE ( 'NONE', #16322, #12204, #1420, .T. ) ;
#15445 = CARTESIAN_POINT ( 'NONE',  ( -58.64405989232411542, 2.944486372867106461, -1.700000000000195577 ) ) ;
#15447 = EDGE_CURVE ( 'NONE', #3458, #10689, #18031, .T. ) ;
#15446 = CARTESIAN_POINT ( 'NONE',  ( 47.27741771404776472, -3.791878011401586868, 1.561538262852513625 ) ) ;
#15448 = CARTESIAN_POINT ( 'NONE',  ( 69.20000000000005969, 3.798169760107705143E-16, 2.729289321880613794 ) ) ;
#15449 = DIRECTION ( 'NONE',  ( 0.000000000000000000, 0.000000000000000000, 1.000000000000000000 ) ) ;
#15451 = CARTESIAN_POINT ( 'NONE',  ( 51.25569095016093257, -4.350592967663767574, 1.494824413850131428 ) ) ;
#15450 = DIRECTION ( 'NONE',  ( 0.000000000000000000, 0.2008964009354144709, -0.9796124928211140670 ) ) ;
#15452 = CIRCLE ( 'NONE', #8856, 2.824999999999998845 ) ;
#15453 = CARTESIAN_POINT ( 'NONE',  ( -58.53335481156722864, 3.238593381231847257, 2.874284765127023356 ) ) ;
#15454 = VECTOR ( 'NONE', #20463, 1000.000000000000000 ) ;
#15455 = DIRECTION ( 'NONE',  ( 0.000000000000000000, 1.000000000000000000, 0.000000000000000000 ) ) ;
#15456 = CARTESIAN_POINT ( 'NONE',  ( -36.52757395963740095, 0.8926979523208172784, 5.334280177567949366 ) ) ;
#15457 = VERTEX_POINT ( 'NONE', #5458 ) ;
#15458 = DIRECTION ( 'NONE',  ( 1.000000000000000000, -0.000000000000000000, -0.000000000000000000 ) ) ;
#15459 = CARTESIAN_POINT ( 'NONE',  ( 54.28498591791677796, 6.002444397903692774, 2.049999999999814637 ) ) ;
#15460 = AXIS2_PLACEMENT_3D ( 'NONE', #11269, #23800, #28708 ) ;
#15461 = ORIENTED_EDGE ( 'NONE', *, *, #16851, .F. ) ;
#15462 = DIRECTION ( 'NONE',  ( 0.000000000000000000, 0.000000000000000000, 1.000000000000000000 ) ) ;
#15463 = ORIENTED_EDGE ( 'NONE', *, *, #10739, .F. ) ;
#15464 = AXIS2_PLACEMENT_3D ( 'NONE', #30034, #6000, #6291 ) ;
#15465 = CARTESIAN_POINT ( 'NONE',  ( 51.71858290632728483, 4.174878015463704628, 1.931423039627790494 ) ) ;
#15466 = CARTESIAN_POINT ( 'NONE',  ( -35.85663232820597557, -5.340403872473347135, 0.9205822173395924457 ) ) ;
#15468 = CARTESIAN_POINT ( 'NONE',  ( 51.70000000000000995, -3.550773357292059007, -2.049880134336001802 ) ) ;
#15467 = CARTESIAN_POINT ( 'NONE',  ( 51.80000000000001137, 6.475000000000062705, -2.050000000000180123 ) ) ;
#15469 = EDGE_LOOP ( 'NONE', ( #23380, #24428, #30571 ) ) ;
#15470 = EDGE_CURVE ( 'NONE', #18483, #24201, #19052, .T. ) ;
#15471 = CARTESIAN_POINT ( 'NONE',  ( 58.75000000000002842, -1.077297519403677128, 1.655311165517035166 ) ) ;
#15472 = EDGE_CURVE ( 'NONE', #23673, #26730, #15489, .T. ) ;
#15473 = DIRECTION ( 'NONE',  ( 1.000000000000000000, 3.053848253006669023E-16, -2.042510438544995415E-16 ) ) ;
#15474 = AXIS2_PLACEMENT_3D ( 'NONE', #19207, #23459, #14271 ) ;
#15475 = ORIENTED_EDGE ( 'NONE', *, *, #11583, .T. ) ;
#15477 = CARTESIAN_POINT ( 'NONE',  ( -35.85663232820584057, 3.275050215668586784, -2.949461045527574932 ) ) ;
#15476 = FACE_OUTER_BOUND ( 'NONE', #18057, .T. ) ;
#15478 = EDGE_CURVE ( 'NONE', #29552, #18413, #28211, .T. ) ;
#15479 = CARTESIAN_POINT ( 'NONE',  ( 48.30000000000001847, 2.428612866367529932E-14, 0.000000000000000000 ) ) ;
#15480 = ORIENTED_EDGE ( 'NONE', *, *, #3003, .F. ) ;
#15481 = CARTESIAN_POINT ( 'NONE',  ( 50.30000000000001847, 1.391941090707534023, 3.850000000000022737 ) ) ;
#15482 = CARTESIAN_POINT ( 'NONE',  ( 34.55000000000001847, 0.000000000000000000, 0.000000000000000000 ) ) ;
#15483 = CIRCLE ( 'NONE', #18023, 2.625000000000000444 ) ;
#15484 = CARTESIAN_POINT ( 'NONE',  ( 58.65266784251163301, 1.656109637136700785, -0.8793208749727724483 ) ) ;
#15485 = AXIS2_PLACEMENT_3D ( 'NONE', #9195, #11570, #8850 ) ;
#15486 =( NAMED_UNIT ( * ) SI_UNIT ( $, .STERADIAN. ) SOLID_ANGLE_UNIT ( ) );
#15487 = CARTESIAN_POINT ( 'NONE',  ( -61.82615520548803545, -2.612112197326142304, -0.4148502322964471856 ) ) ;
#15488 = CARTESIAN_POINT ( 'NONE',  ( 52.10126625705173353, -0.5195911883732942105, 1.546252172343134834 ) ) ;
#15489 = CIRCLE ( 'NONE', #16509, 3.499999999999999556 ) ;
#15490 = ORIENTED_EDGE ( 'NONE', *, *, #18636, .T. ) ;
#15491 = TOROIDAL_SURFACE ( 'NONE', #5863, 1.239999999999999991, 0.01000000000000000021 ) ;
#15492 = CIRCLE ( 'NONE', #1334, 4.100000000000022737 ) ;
#15493 = VECTOR ( 'NONE', #10848, 1000.000000000000000 ) ;
#15494 = CARTESIAN_POINT ( 'NONE',  ( 15.30042582489635095, -2.199885882962415717, 4.939696253590554420 ) ) ;
#15495 = DIRECTION ( 'NONE',  ( 2.614375865348240525E-16, -0.2008964009354147762, 0.9796124928211140670 ) ) ;
#15496 = CARTESIAN_POINT ( 'NONE',  ( 53.91574522233626965, 6.672251602764244893, -1.774295313897662485 ) ) ;
#15497 = AXIS2_PLACEMENT_3D ( 'NONE', #22716, #1011, #10663 ) ;
#15498 = VECTOR ( 'NONE', #14251, 1000.000000000000000 ) ;
#15499 = CARTESIAN_POINT ( 'NONE',  ( -56.32202994616206126, 2.078460969082643217, 3.599999999999808686 ) ) ;
#15500 = CIRCLE ( 'NONE', #1850, 0.2600000000000000644 ) ;
#15501 = DIRECTION ( 'NONE',  ( -0.5633368246414944824, -0.8262273428075580517, 0.000000000000000000 ) ) ;
#15502 = CARTESIAN_POINT ( 'NONE',  ( 23.13157261764652972, 6.282290353147255146, 2.049999999999918110 ) ) ;
#15503 = ORIENTED_EDGE ( 'NONE', *, *, #2074, .F. ) ;
#15504 = CARTESIAN_POINT ( 'NONE',  ( -59.19999999999997442, 2.449420067797480893, 1.250136525132548693 ) ) ;
#15505 = CIRCLE ( 'NONE', #14515, 1.875000000000001776 ) ;
#15506 = EDGE_LOOP ( 'NONE', ( #5620, #3087, #21615 ) ) ;
#15507 = PRODUCT_DEFINITION_CONTEXT ( 'detailed design', #486, 'design' ) ;
#15508 = CARTESIAN_POINT ( 'NONE',  ( -59.10126175456193209, 2.465973215726302570, -0.9703132803711642662 ) ) ;
#15510 = CARTESIAN_POINT ( 'NONE',  ( -58.06249999999996447, -0.7533615035078129463, 3.673546848079175309 ) ) ;
#15509 = CARTESIAN_POINT ( 'NONE',  ( 15.76675455518197388, -3.261791109367189634, -4.314133646218568430 ) ) ;
#15511 = AXIS2_PLACEMENT_3D ( 'NONE', #21046, #23569, #8997 ) ;
#15512 = ORIENTED_EDGE ( 'NONE', *, *, #21273, .F. ) ;
#15513 = ORIENTED_EDGE ( 'NONE', *, *, #3707, .F. ) ;
#15514 = CARTESIAN_POINT ( 'NONE',  ( 64.25000000000001421, 1.163569835200988601E-28, -2.243276760206714411E-13 ) ) ;
#15515 = CIRCLE ( 'NONE', #5405, 160.1997717543138720 ) ;
#15516 = EDGE_CURVE ( 'NONE', #13230, #11849, #1329, .T. ) ;
#15517 = DIRECTION ( 'NONE',  ( 1.000000000000000000, 3.053848253006669023E-16, -2.042510438544995415E-16 ) ) ;
#15518 = ORIENTED_EDGE ( 'NONE', *, *, #14041, .F. ) ;
#15519 = AXIS2_PLACEMENT_3D ( 'NONE', #5609, #6080, #3225 ) ;
#15521 = CARTESIAN_POINT ( 'NONE',  ( -60.54999999999995453, -0.7328781032566554776, 3.573665542649864246 ) ) ;
#15520 = CARTESIAN_POINT ( 'NONE',  ( -56.38452994616205416, 3.117691453623979481, 1.799999999999811751 ) ) ;
#15522 = CARTESIAN_POINT ( 'NONE',  ( -59.23542740578359656, -3.725040285533365747, 1.239922660687675871 ) ) ;
#15523 = DIRECTION ( 'NONE',  ( 0.000000000000000000, 0.000000000000000000, -1.000000000000000000 ) ) ;
#15524 = DIRECTION ( 'NONE',  ( 1.000000000000000000, 0.000000000000000000, 0.000000000000000000 ) ) ;
#15525 = DIRECTION ( 'NONE',  ( 0.000000000000000000, 0.000000000000000000, 1.000000000000000000 ) ) ;
#15526 =( NAMED_UNIT ( * ) PLANE_ANGLE_UNIT ( ) SI_UNIT ( $, .RADIAN. ) );
#15527 = VECTOR ( 'NONE', #12344, 1000.000000000000000 ) ;
#15528 = ORIENTED_EDGE ( 'NONE', *, *, #31217, .F. ) ;
#15529 = CIRCLE ( 'NONE', #5926, 0.1500000000000001887 ) ;
#15530 = ADVANCED_FACE ( 'NONE', ( #15414 ), #18528, .T. ) ;
#15531 = AXIS2_PLACEMENT_3D ( 'NONE', #5728, #29949, #13158 ) ;
#15532 = CARTESIAN_POINT ( 'NONE',  ( 54.16075265905997327, 5.605215124043997577, -2.050000000000188560 ) ) ;
#15533 = CARTESIAN_POINT ( 'NONE',  ( 48.33046193264123502, -1.143620537822785721, -3.937943076466140724 ) ) ;
#15534 = CYLINDRICAL_SURFACE ( 'NONE', #12413, 1.250000000000000222 ) ;
#15535 = DIRECTION ( 'NONE',  ( -3.489354422748178582E-15, 1.218509414717996338E-16, -1.000000000000000000 ) ) ;
#15536 = CIRCLE ( 'NONE', #1885, 0.04999999999999988481 ) ;
#15537 = CIRCLE ( 'NONE', #3923, 0.1000000000000001027 ) ;
#15539 = DIRECTION ( 'NONE',  ( 1.000000000000000000, 1.047444401652940007E-14, 0.000000000000000000 ) ) ;
#15538 = DIRECTION ( 'NONE',  ( 0.000000000000000000, 0.000000000000000000, -1.000000000000000000 ) ) ;
#15540 = CIRCLE ( 'NONE', #28193, 0.09999999999999983902 ) ;
#15541 = CARTESIAN_POINT ( 'NONE',  ( -62.08600056051449201, -2.518032341469984559, 0.1874854198766372493 ) ) ;
#15542 = DIRECTION ( 'NONE',  ( 1.000000000000000000, 1.047444401652940007E-14, 0.000000000000000000 ) ) ;
#15544 = CARTESIAN_POINT ( 'NONE',  ( -62.09999999999997300, -2.706459356064251587, -0.3286898414610474606 ) ) ;
#15543 = CARTESIAN_POINT ( 'NONE',  ( -35.85663232820584057, 4.804073783693418420, 2.042134687550397398 ) ) ;
#15545 = ORIENTED_EDGE ( 'NONE', *, *, #2975, .F. ) ;
#15546 = CARTESIAN_POINT ( 'NONE',  ( 50.33305158408655444, -1.365427245289796199, -3.854926352964885172 ) ) ;
#15547 = CARTESIAN_POINT ( 'NONE',  ( -36.14490256869205353, 3.997744010329720599, -3.641645661657078037 ) ) ;
#15548 = AXIS2_PLACEMENT_3D ( 'NONE', #4216, #9146, #16413 ) ;
#15550 = CARTESIAN_POINT ( 'NONE',  ( 48.00000000000001421, -4.031600731908413948, -1.173113608511841877 ) ) ;
#15549 = CARTESIAN_POINT ( 'NONE',  ( 51.45655683570191741, -0.9591657938390838467, -1.611094652690527873 ) ) ;
#15551 = CARTESIAN_POINT ( 'NONE',  ( 51.70000000000002416, 6.982261990806648555E-14, -1.793082891011605378E-13 ) ) ;
#15552 = VERTEX_POINT ( 'NONE', #24606 ) ;
#15553 = CARTESIAN_POINT ( 'NONE',  ( 53.82754651211528341, 4.897847608402548403, 2.049999999999811973 ) ) ;
#15554 = CARTESIAN_POINT ( 'NONE',  ( 34.56702326949724835, 8.213851659285209550, -1.550000000000119948 ) ) ;
#15555 = CIRCLE ( 'NONE', #29209, 0.04999999999999969746 ) ;
#15556 = EDGE_CURVE ( 'NONE', #7731, #21976, #3864, .T. ) ;
#15557 = CIRCLE ( 'NONE', #6469, 0.04999999999999969746 ) ;
#15558 = VERTEX_POINT ( 'NONE', #3227 ) ;
#15560 = B_SPLINE_CURVE_WITH_KNOTS ( 'NONE', 3,
 ( #15869, #1463, #16346, #23648, #18582, #28227, #28532, #13786, #11604, #25691, #16196, #11435, #23323, #6371, #25378, #23179, #8590, #3835, #18889, #30913, #23010, #30581, #8731, #21126, #21285, #18269, #28380, #13642 ),
 .UNSPECIFIED., .F., .F.,
 ( 4, 2, 2, 2, 2, 2, 2, 2, 2, 2, 2, 2, 2, 4 ),
 ( 0.003059686050519344613, 0.004393787003443038949, 0.005060837479904890454, 0.005727887956366741959, 0.007061988909290444101, 0.007729039385752295606, 0.008396089862214146243, 0.009063140338675997748, 0.009730190815137849253, 0.01106429176806155226, 0.01239839272098525527, 0.01306544319744710331, 0.01339896843567802559, 0.01373249367390894961 ),
 .UNSPECIFIED. ) ;
#15559 = FACE_OUTER_BOUND ( 'NONE', #24995, .T. ) ;
#15561 = ORIENTED_EDGE ( 'NONE', *, *, #7794, .F. ) ;
#15562 = DIRECTION ( 'NONE',  ( 0.000000000000000000, 0.2008964009354147762, -0.9796124928211140670 ) ) ;
#15563 = CARTESIAN_POINT ( 'NONE',  ( 47.54039588126945404, -4.349885043120369055, -1.496908008647668709 ) ) ;
#15564 = ORIENTED_EDGE ( 'NONE', *, *, #3960, .T. ) ;
#15565 = SURFACE_STYLE_USAGE ( .BOTH. , #22236 ) ;
#15566 = CARTESIAN_POINT ( 'NONE',  ( -68.01382336603234080, 0.6601810586021495952, -3.219179684251513685 ) ) ;
#15567 = CIRCLE ( 'NONE', #20645, 0.1000000000000000056 ) ;
#15568 = CARTESIAN_POINT ( 'NONE',  ( -59.50952994616202574, 3.117691453623994580, -1.800000000000197664 ) ) ;
#15569 = ORIENTED_EDGE ( 'NONE', *, *, #14484, .T. ) ;
#15570 = DIRECTION ( 'NONE',  ( 0.000000000000000000, -0.3137254901960767617, 0.9495137264943732669 ) ) ;
#15571 = ORIENTED_EDGE ( 'NONE', *, *, #9432, .F. ) ;
#15572 = FACE_OUTER_BOUND ( 'NONE', #5775, .T. ) ;
#15573 = ORIENTED_EDGE ( 'NONE', *, *, #23952, .T. ) ;
#15574 = EDGE_CURVE ( 'NONE', #14364, #5594, #27601, .T. ) ;
#15575 = CARTESIAN_POINT ( 'NONE',  ( -56.37499999999998579, -3.920666489018338045E-15, 3.399999999999799183 ) ) ;
#15576 = DIRECTION ( 'NONE',  ( -9.654113257610060303E-15, 0.000000000000000000, -1.000000000000000000 ) ) ;
#15577 = CARTESIAN_POINT ( 'NONE',  ( -59.29999999999997584, 2.330309927981285032E-15, 4.253626757584724400E-16 ) ) ;
#15578 = TOROIDAL_SURFACE ( 'NONE', #12953, 1.975000000000001865, 0.1000000000000000056 ) ;
#15579 = CARTESIAN_POINT ( 'NONE',  ( 34.56702326949724835, 8.213851659285209550, -1.950000000000119860 ) ) ;
#15580 = LINE ( 'NONE', #3545, #29704 ) ;
#15581 = VECTOR ( 'NONE', #6877, 1000.000000000000000 ) ;
#15582 = AXIS2_PLACEMENT_3D ( 'NONE', #4127, #25971, #3809 ) ;
#15584 = CARTESIAN_POINT ( 'NONE',  ( -54.49999999999997868, 3.673546848079182858, 0.7533615035078058408 ) ) ;
#15583 = DIRECTION ( 'NONE',  ( -1.000000000000000000, -1.047444401652940007E-14, -0.000000000000000000 ) ) ;
#15585 = CARTESIAN_POINT ( 'NONE',  ( -60.59999999999997300, -2.342723651847746336, 0.9419505778294103848 ) ) ;
#15586 = FACE_OUTER_BOUND ( 'NONE', #26800, .T. ) ;
#15587 = DIRECTION ( 'NONE',  ( 0.000000000000000000, -1.000000000000000000, 8.673617379884030739E-15 ) ) ;
#15588 = CARTESIAN_POINT ( 'NONE',  ( 58.65266784251157617, 1.372094080477309186, -1.277991457600056391 ) ) ;
#15589 = CARTESIAN_POINT ( 'NONE',  ( 54.02638549814044211, 7.248122547115673164, -2.050000000000188560 ) ) ;
#15590 = ORIENTED_EDGE ( 'NONE', *, *, #3581, .T. ) ;
#15591 = CARTESIAN_POINT ( 'NONE',  ( 50.49738912176885464, -0.9335627837657783923, 3.994936164801344614 ) ) ;
#15592 = DIRECTION ( 'NONE',  ( 1.000000000000000000, 1.047444401652940007E-14, 0.000000000000000000 ) ) ;
#15593 = VERTEX_POINT ( 'NONE', #29497 ) ;
#15594 = EDGE_CURVE ( 'NONE', #24984, #11667, #23095, .T. ) ;
#15595 = EDGE_LOOP ( 'NONE', ( #25780, #17205, #4837, #16174 ) ) ;
#15596 = CARTESIAN_POINT ( 'NONE',  ( 51.80000000000001137, -4.319730106884873244, -1.256953381662418101 ) ) ;
#15597 = CARTESIAN_POINT ( 'NONE',  ( -58.79792740578360366, 3.330682475591789427, 0.6830477631804110494 ) ) ;
#15599 = FACE_OUTER_BOUND ( 'NONE', #2480, .T. ) ;
#15598 = CARTESIAN_POINT ( 'NONE',  ( -57.56249999999995737, -1.962990915244707368, -3.400000000000210854 ) ) ;
#15600 = EDGE_CURVE ( 'NONE', #29622, #24431, #5880, .T. ) ;
#15601 = ORIENTED_EDGE ( 'NONE', *, *, #304, .F. ) ;
#15602 = VERTEX_POINT ( 'NONE', #15875 ) ;
#15603 = VECTOR ( 'NONE', #12648, 1000.000000000000000 ) ;
#15604 = DIRECTION ( 'NONE',  ( 0.000000000000000000, 0.000000000000000000, 1.000000000000000000 ) ) ;
#15605 = ORIENTED_EDGE ( 'NONE', *, *, #20222, .T. ) ;
#15606 = CARTESIAN_POINT ( 'NONE',  ( 49.05000000000005400, 1.401298464324817071E-42, 2.624999999999484857 ) ) ;
#15607 = ORIENTED_EDGE ( 'NONE', *, *, #16608, .T. ) ;
#15608 = CARTESIAN_POINT ( 'NONE',  ( 60.75000000000001421, 0.5000000000006363798, 1.863080903344386030 ) ) ;
#15609 = MANIFOLD_SOLID_BREP ( 'Stock-MAS-683-1', #16029 ) ;
#15610 =( BOUNDED_SURFACE ( )  B_SPLINE_SURFACE ( 3, 2, ( 
 ( #6256, #8934, #20690 ),
 ( #22896, #8624, #25728 ),
 ( #18622, #28263, #6573 ),
 ( #17982, #20526, #27631 ),
 ( #1044, #1643, #27796 ),
 ( #23047, #30316, #27940 ) ),
 .UNSPECIFIED., .F., .F., .T. ) 
 B_SPLINE_SURFACE_WITH_KNOTS ( ( 4, 2, 4 ),
 ( 3, 3 ),
 ( 0.0001437848949530157389, 0.0003024153973479691408, 0.0004610458997429225697 ),
 ( 0.000000000000000000, 1.000000000000000000 ),
 .UNSPECIFIED. ) 
 GEOMETRIC_REPRESENTATION_ITEM ( )  RATIONAL_B_SPLINE_SURFACE ( (
 ( 1.000000000000000000, 0.7071067811865479058, 1.000000000000000000),
 ( 1.000000000000000000, 0.7306243023313020446, 1.000000000000000000),
 ( 1.000000000000000000, 0.7490085278695750581, 1.000000000000000000),
 ( 1.000000000000000000, 0.7725095633944483176, 1.000000000000000000),
 ( 1.000000000000000000, 0.7779630306549427665, 1.000000000000000000),
 ( 1.000000000000000000, 0.7779866052154988942, 1.000000000000000000) ) ) 
 REPRESENTATION_ITEM ( '' )  SURFACE ( )  );
#15611 = EDGE_LOOP ( 'NONE', ( #25830, #25839, #6270, #27586 ) ) ;
#15612 = CARTESIAN_POINT ( 'NONE',  ( -73.84999999999996589, 1.301636140808604125, 0.03242509391110787870 ) ) ;
#15613 = PLANE ( 'NONE',  #27 ) ;
#15614 = ADVANCED_FACE ( 'NONE', ( #1769 ), #6227, .T. ) ;
#15615 = CARTESIAN_POINT ( 'NONE',  ( -44.49999999999997868, 6.542789527549899840E-15, -1.397091617737396343E-15 ) ) ;
#15616 = APPLICATION_CONTEXT ( 'automotive_design' ) ;
#15617 = CARTESIAN_POINT ( 'NONE',  ( -57.89405989232411542, 2.944486372867106461, -1.700000000000192912 ) ) ;
#15618 = CARTESIAN_POINT ( 'NONE',  ( 47.00299618517622946, -3.613796805337473383, 1.940711795750564628 ) ) ;
#15619 = CARTESIAN_POINT ( 'NONE',  ( 58.75000018803716983, 1.333992738916855325, 1.403930843797372541 ) ) ;
#15620 = CARTESIAN_POINT ( 'NONE',  ( 48.41300975153458097, 1.088846059295805135, 3.899771020632008423 ) ) ;
#15621 = CARTESIAN_POINT ( 'NONE',  ( 58.72200959573710577, -0.5298027519206366387, 1.799185603788605148 ) ) ;
#15623 = CARTESIAN_POINT ( 'NONE',  ( 58.75000000000002132, 6.153735859711025284E-13, 3.111507638930570854E-58 ) ) ;
#15622 = CARTESIAN_POINT ( 'NONE',  ( -59.18789508915042319, 2.395752775956333291, 1.250136525132548915 ) ) ;
#15624 = EDGE_CURVE ( 'NONE', #18734, #1692, #8900, .T. ) ;
#15625 =( GEOMETRIC_REPRESENTATION_CONTEXT ( 3 ) GLOBAL_UNCERTAINTY_ASSIGNED_CONTEXT ( ( #17408 ) ) GLOBAL_UNIT_ASSIGNED_CONTEXT ( ( #5905, #25041, #7792 ) ) REPRESENTATION_CONTEXT ( 'NONE', 'WORKASPACE' ) );
#15626 = DIRECTION ( 'NONE',  ( 0.000000000000000000, -0.2008964009354147484, 0.9796124928211138450 ) ) ;
#15627 = CARTESIAN_POINT ( 'NONE',  ( 51.25000000000002842, -1.099999999999462963, -1.996089927833914146 ) ) ;
#15628 = AXIS2_PLACEMENT_3D ( 'NONE', #11362, #18981, #30512 ) ;
#15629 = DIRECTION ( 'NONE',  ( 0.000000000000000000, -1.000000000000000000, 0.000000000000000000 ) ) ;
#15630 = ORIENTED_EDGE ( 'NONE', *, *, #21367, .F. ) ;
#15631 = CARTESIAN_POINT ( 'NONE',  ( 54.40536568400169415, 5.987876372949615167, 1.624999999999809930 ) ) ;
#15632 = ORIENTED_EDGE ( 'NONE', *, *, #25197, .T. ) ;
#15633 = CARTESIAN_POINT ( 'NONE',  ( -59.39405989232410832, 2.944486372867118451, -1.700000000000178035 ) ) ;
#15634 = ORIENTED_EDGE ( 'NONE', *, *, #6103, .T. ) ;
#15635 = EDGE_CURVE ( 'NONE', #11459, #15281, #14468, .T. ) ;
#15636 = CARTESIAN_POINT ( 'NONE',  ( 59.35000000000007248, 4.898587196589447341E-16, 3.999999999999378275 ) ) ;
#15637 = CARTESIAN_POINT ( 'NONE',  ( -54.84585481156724285, 3.673546848079182858, 0.7533615035078058408 ) ) ;
#15639 = CARTESIAN_POINT ( 'NONE',  ( 61.25000000000000711, 1.470078920828170821, -1.470078920826818125 ) ) ;
#15638 = CARTESIAN_POINT ( 'NONE',  ( -54.49999999999999289, 1.499999999999998002, 3.363870538531246623 ) ) ;
#15640 = ADVANCED_FACE ( 'NONE', ( #11273 ), #8447, .T. ) ;
#15641 = EDGE_LOOP ( 'NONE', ( #19803, #30303, #13888, #5603, #23165, #15475, #2109, #14162, #15237 ) ) ;
#15642 = CARTESIAN_POINT ( 'NONE',  ( 61.16289782575152145, -0.6851579758920108842, -1.477831714898571347 ) ) ;
#15643 = DIRECTION ( 'NONE',  ( 0.000000000000000000, 1.000000000000000000, 0.000000000000000000 ) ) ;
#15644 = ORIENTED_EDGE ( 'NONE', *, *, #3282, .T. ) ;
#15646 = DIRECTION ( 'NONE',  ( 1.000000000000000000, 0.000000000000000000, 0.000000000000000000 ) ) ;
#15645 = DIRECTION ( 'NONE',  ( -0.9993908270190956511, 0.03489949670250096919, 3.491481338843132961E-15 ) ) ;
#15647 = DIRECTION ( 'NONE',  ( -3.489354422748178188E-15, 1.218509414717996091E-16, -1.000000000000000000 ) ) ;
#15648 = EDGE_LOOP ( 'NONE', ( #6602, #10041, #23360, #20720 ) ) ;
#15649 = DIRECTION ( 'NONE',  ( 3.002035892788117459E-16, -0.9996898646859343485, -0.02490330187381124133 ) ) ;
#15650 = CARTESIAN_POINT ( 'NONE',  ( -54.58155989232413674, -1.962990915244731571, 3.399999999999796962 ) ) ;
#15651 = MECHANICAL_DESIGN_GEOMETRIC_PRESENTATION_REPRESENTATION (  '', ( #24744 ), #21226 ) ;
#15652 = TOROIDAL_SURFACE ( 'NONE', #1482, 159.7997717543496776, 0.1000000000000000056 ) ;
#15653 = FACE_OUTER_BOUND ( 'NONE', #4597, .T. ) ;
#15654 = DIRECTION ( 'NONE',  ( -1.000000000000000000, -0.000000000000000000, 1.047444401652940007E-14 ) ) ;
#15655 = CYLINDRICAL_SURFACE ( 'NONE', #4771, 0.09999999999999982514 ) ;
#15656 = VERTEX_POINT ( 'NONE', #25528 ) ;
#15657 = FACE_OUTER_BOUND ( 'NONE', #30331, .T. ) ;
#15658 = EDGE_CURVE ( 'NONE', #9993, #9597, #1469, .T. ) ;
#15659 = FACE_OUTER_BOUND ( 'NONE', #20891, .T. ) ;
#15660 = AXIS2_PLACEMENT_3D ( 'NONE', #9502, #23747, #1560 ) ;
#15662 = ADVANCED_FACE ( 'NONE', ( #25384 ), #16204, .T. ) ;
#15661 = FACE_BOUND ( 'NONE', #1444, .T. ) ;
#15663 = CARTESIAN_POINT ( 'NONE',  ( -58.82202994616202574, 2.078460969082688514, -3.600000000000191935 ) ) ;
#15664 = VERTEX_POINT ( 'NONE', #13173 ) ;
#15665 = CARTESIAN_POINT ( 'NONE',  ( 58.74999999305998699, -1.929066554547878454, 0.02566444196692819688 ) ) ;
#15666 = CARTESIAN_POINT ( 'NONE',  ( 48.50000000000263611, 1.409901620923733390, -3.849999999997240518 ) ) ;
#15667 = ORIENTED_EDGE ( 'NONE', *, *, #6290, .F. ) ;
#15668 = VECTOR ( 'NONE', #27660, 1000.000000000000000 ) ;
#15669 = AXIS2_PLACEMENT_3D ( 'NONE', #27399, #6187, #30391 ) ;
#15670 = CYLINDRICAL_SURFACE ( 'NONE', #10281, 0.1000000000000002554 ) ;
#15671 = VERTEX_POINT ( 'NONE', #4307 ) ;
#15672 = CARTESIAN_POINT ( 'NONE',  ( -54.39999999999999147, -1.514093959731547701, 3.183260039818139653 ) ) ;
#15674 = DIRECTION ( 'NONE',  ( 0.000000000000000000, -1.000000000000000000, -3.491481338843137694E-15 ) ) ;
#15673 = CARTESIAN_POINT ( 'NONE',  ( 48.40000000000002700, 0.7711297561636268894, 3.938774833552663335 ) ) ;
#15675 = VERTEX_POINT ( 'NONE', #13958 ) ;
#15676 = ORIENTED_EDGE ( 'NONE', *, *, #24341, .F. ) ;
#15677 = DIRECTION ( 'NONE',  ( 0.3420201433256666590, 0.02340144900402443481, -0.9394011889198365939 ) ) ;
#15678 = CARTESIAN_POINT ( 'NONE',  ( 27.62808879389201522, 5.849836810644521989, -1.425000000000096412 ) ) ;
#15679 = ORIENTED_EDGE ( 'NONE', *, *, #27923, .T. ) ;
#15681 = DIRECTION ( 'NONE',  ( 1.000000000000000000, 3.053848253006669023E-16, -2.042510438544995415E-16 ) ) ;
#15680 = DIRECTION ( 'NONE',  ( 2.614375865348240525E-16, -0.2008964009354147762, 0.9796124928211140670 ) ) ;
#15682 = CARTESIAN_POINT ( 'NONE',  ( -59.11042740578359656, -2.936324665650201560, -2.606018187048497747 ) ) ;
#15683 = CARTESIAN_POINT ( 'NONE',  ( -35.85663232820596846, -4.861582140531631069, -2.394243978978344956 ) ) ;
#15684 = APPLICATION_PROTOCOL_DEFINITION ( 'draft international standard', 'automotive_design', 1998, #10736 ) ;
#15685 = CARTESIAN_POINT ( 'NONE',  ( 68.05000000000002558, 1.401298464324817071E-42, -7.127859153248258291E-13 ) ) ;
#15686 = SHAPE_REPRESENTATION_RELATIONSHIP ( 'NONE' , 'NONE' ,  #549, #2132 ) ;
#15687 = ORIENTED_EDGE ( 'NONE', *, *, #7552, .T. ) ;
#15688 = DIRECTION ( 'NONE',  ( 1.344447539785323523E-44, -1.000000000000000000, -3.491481338843137300E-15 ) ) ;
#15689 = CARTESIAN_POINT ( 'NONE',  ( 53.16217804548203674, 8.131925109091699966, -2.050000000000185008 ) ) ;
#15690 = CARTESIAN_POINT ( 'NONE',  ( 51.13996726386383784, 0.9386186536674969716, -1.439073407537156069 ) ) ;
#15691 = CARTESIAN_POINT ( 'NONE',  ( 15.49676243306307732, -0.05686983728431626445, 5.199999998843000348 ) ) ;
#15692 = EDGE_CURVE ( 'NONE', #28800, #24288, #23187, .T. ) ;
#15693 = EDGE_CURVE ( 'NONE', #4483, #23272, #17022, .T. ) ;
#15694 = B_SPLINE_CURVE_WITH_KNOTS ( 'NONE', 3,
 ( #27817, #20707, #30335, #31117, #28437, #4674, #7070, #14178, #19114, #2302, #11504, #31283, #16733, #21806, #18795, #9447 ),
 .UNSPECIFIED., .F., .F.,
 ( 4, 3, 3, 3, 3, 4 ),
 ( 0.000000000000000000, 3.448798496382319379E-05, 6.876885415380709437E-05, 0.0001064608974028143388, 0.0001221728072927708356, 0.0001243510251068951895 ),
 .UNSPECIFIED. ) ;
#15695 = CARTESIAN_POINT ( 'NONE',  ( -59.29999999999997584, 2.330309927981285032E-15, 4.253626757584724400E-16 ) ) ;
#15697 = LINE ( 'NONE', #11091, #28079 ) ;
#15696 = CYLINDRICAL_SURFACE ( 'NONE', #19109, 0.2500000000000000000 ) ;
#15698 = CARTESIAN_POINT ( 'NONE',  ( 51.25000000000001421, 1.100000000000534994, -1.001327244211404732 ) ) ;
#15699 = DIRECTION ( 'NONE',  ( 0.000000000000000000, 0.000000000000000000, 1.000000000000000000 ) ) ;
#15701 = CARTESIAN_POINT ( 'NONE',  ( -62.34999999999997300, 2.799131621120618085, 0.06972924524667374613 ) ) ;
#15700 = CARTESIAN_POINT ( 'NONE',  ( -59.50499785763158656, 3.022972365879558421, 1.564058272419715179 ) ) ;
#15702 = ORIENTED_EDGE ( 'NONE', *, *, #19683, .T. ) ;
#15703 = DIRECTION ( 'NONE',  ( 0.000000000000000000, 0.000000000000000000, 1.000000000000000000 ) ) ;
#15704 = MANIFOLD_SOLID_BREP ( 'Stock-MAS-683-1', #26666 ) ;
#15705 = DIRECTION ( 'NONE',  ( -1.000000000000000000, 1.219044193948983948E-29, -3.491481338843133355E-15 ) ) ;
#15707 = CARTESIAN_POINT ( 'NONE',  ( 58.65000000000003411, -1.022750809560713181, -1.571497941946363497 ) ) ;
#15706 = CARTESIAN_POINT ( 'NONE',  ( 58.75000018595668649, 1.883137918660746202, 0.4528999722754235568 ) ) ;
#15708 = FACE_OUTER_BOUND ( 'NONE', #25517, .T. ) ;
#15709 = VERTEX_POINT ( 'NONE', #14439 ) ;
#15710 = CARTESIAN_POINT ( 'NONE',  ( 52.18331218360316370, 8.688678219032366812, 2.049999999999818190 ) ) ;
#15711 = CARTESIAN_POINT ( 'NONE',  ( -60.64918514029853469, -2.458741238023958608, -1.115600605136573220 ) ) ;
#15712 = ADVANCED_FACE ( 'NONE', ( #18897 ), #4709, .T. ) ;
#15713 = VERTEX_POINT ( 'NONE', #29172 ) ;
#15714 = DIRECTION ( 'NONE',  ( -1.000000000000000000, 0.000000000000000000, 1.047444401652940007E-14 ) ) ;
#15715 = ORIENTED_EDGE ( 'NONE', *, *, #19031, .T. ) ;
#15716 = DIRECTION ( 'NONE',  ( 1.000000000000000000, -0.000000000000000000, -0.000000000000000000 ) ) ;
#15717 = FACE_OUTER_BOUND ( 'NONE', #23499, .T. ) ;
#15718 = EDGE_LOOP ( 'NONE', ( #10147, #513, #23201, #6593 ) ) ;
#15719 = VECTOR ( 'NONE', #11562, 1000.000000000000000 ) ;
#15720 = CARTESIAN_POINT ( 'NONE',  ( -55.88452994616203995, 2.269957418536587429E-14, -3.600000000000198597 ) ) ;
#15721 = CARTESIAN_POINT ( 'NONE',  ( -56.70655989232412253, -3.925981830489445379, -2.155497846303743205E-13 ) ) ;
#15722 = ORIENTED_EDGE ( 'NONE', *, *, #2208, .T. ) ;
#15723 = CARTESIAN_POINT ( 'NONE',  ( 57.01359174706111332, 0.7734660154240907692, -1.735448526467797459 ) ) ;
#15724 = ORIENTED_EDGE ( 'NONE', *, *, #23780, .F. ) ;
#15725 = SHAPE_REPRESENTATION ( 'End Cap', ( #9018 ), #21749 ) ;
#15726 = CARTESIAN_POINT ( 'NONE',  ( -59.06249999999995737, -1.962990915244707368, -3.400000000000216627 ) ) ;
#15727 = CARTESIAN_POINT ( 'NONE',  ( 61.22059884411343234, 0.7794434480088445749, 1.429589005548685954 ) ) ;
#15728 = CARTESIAN_POINT ( 'NONE',  ( -61.82620411128901594, -2.510158248709655648, 0.2872314057388253294 ) ) ;
#15729 = LINE ( 'NONE', #20344, #12948 ) ;
#15730 = CARTESIAN_POINT ( 'NONE',  ( -54.49999999999997868, -1.697688561373014160, -3.084438062315841833 ) ) ;
#15731 = ADVANCED_FACE ( 'NONE', ( #14287 ), #29010, .F. ) ;
#15733 = CYLINDRICAL_SURFACE ( 'NONE', #4807, 0.1500000000000001887 ) ;
#15732 = DIRECTION ( 'NONE',  ( -1.000000000000000000, 1.786249915856167978E-14, 3.435095992031092083E-15 ) ) ;
#15734 = DIRECTION ( 'NONE',  ( 0.3420201433256677137, -0.02340144900402421971, 0.9394011889198362608 ) ) ;
#15735 = DIRECTION ( 'NONE',  ( 1.000000000000000000, 3.053848253006669023E-16, -2.042510438544995415E-16 ) ) ;
#15736 = CARTESIAN_POINT ( 'NONE',  ( -59.69985929041246209, 2.111923219456912193, 1.749892808977832726 ) ) ;
#15737 = CARTESIAN_POINT ( 'NONE',  ( 58.74999981404334903, -1.734728236458829453, -0.9032433253517498928 ) ) ;
#15738 = CARTESIAN_POINT ( 'NONE',  ( 53.74860301653917816, 7.732465014774306589, -2.050000000000187672 ) ) ;
#15739 = VERTEX_POINT ( 'NONE', #9711 ) ;
#15740 = CARTESIAN_POINT ( 'NONE',  ( -62.06710100716625789, -2.637635658083895329, 0.1963493119579511614 ) ) ;
#15741 = CARTESIAN_POINT ( 'NONE',  ( -36.92405921417685732, -0.1434351685890525030, -5.407416993630365099 ) ) ;
#15742 = EDGE_CURVE ( 'NONE', #24661, #22181, #29233, .T. ) ;
#15743 = ORIENTED_EDGE ( 'NONE', *, *, #1559, .T. ) ;
#15744 = DIRECTION ( 'NONE',  ( 1.000000000000000000, 1.047444401652940007E-14, 0.000000000000000000 ) ) ;
#15745 = DIRECTION ( 'NONE',  ( 1.000000000000000000, 1.047444401652940007E-14, 0.000000000000000000 ) ) ;
#15747 = DIRECTION ( 'NONE',  ( 1.000000000000000000, -0.000000000000000000, -0.000000000000000000 ) ) ;
#15746 = CARTESIAN_POINT ( 'NONE',  ( -55.24999999999996447, 2.023778652682505581E-14, -3.400000000000196643 ) ) ;
#15748 = EDGE_LOOP ( 'NONE', ( #1589, #19744, #24781, #9455 ) ) ;
#15749 = ORIENTED_EDGE ( 'NONE', *, *, #31318, .F. ) ;
#15750 = DIRECTION ( 'NONE',  ( -1.499696682456171183E-15, -0.9030524935654884455, 0.4295302013422959697 ) ) ;
#15751 = CIRCLE ( 'NONE', #13204, 3.525000000000025224 ) ;
#15752 = ORIENTED_EDGE ( 'NONE', *, *, #3336, .F. ) ;
#15753 = DIRECTION ( 'NONE',  ( -1.000000000000000000, -0.000000000000000000, 3.491481338843133355E-15 ) ) ;
#15754 = CIRCLE ( 'NONE', #28906, 4.050000000000000711 ) ;
#15755 = EDGE_LOOP ( 'NONE', ( #17548, #22297, #3210, #25574 ) ) ;
#15756 = CARTESIAN_POINT ( 'NONE',  ( 21.97322666366011745, 8.076925076899296840, -2.050000000000075762 ) ) ;
#15757 = CARTESIAN_POINT ( 'NONE',  ( 61.25000000000003553, -1.323060376181777631, 1.499837071478349326 ) ) ;
#15758 = CARTESIAN_POINT ( 'NONE',  ( 58.75000000000001421, 0.6121634413844196931, -1.877732920580865272 ) ) ;
#15759 = ORIENTED_EDGE ( 'NONE', *, *, #15038, .T. ) ;
#15760 = CARTESIAN_POINT ( 'NONE',  ( -69.22071067811863543, 0.4319272620111411776, -2.106166859565393068 ) ) ;
#15761 = CARTESIAN_POINT ( 'NONE',  ( 52.20711756518984714, -0.7499999999994533262, 1.718465885608439825 ) ) ;
#15762 = CARTESIAN_POINT ( 'NONE',  ( -60.45655989232412253, -3.925981830489445379, -2.286428396510360233E-13 ) ) ;
#15763 = DIRECTION ( 'NONE',  ( 0.000000000000000000, -1.000000000000000000, 0.000000000000000000 ) ) ;
#15764 = CARTESIAN_POINT ( 'NONE',  ( 58.65266784251148380, 1.277991457600490932, 1.372094080476860878 ) ) ;
#15765 = EDGE_CURVE ( 'NONE', #15927, #16106, #1355, .T. ) ;
#15766 = AXIS2_PLACEMENT_3D ( 'NONE', #15405, #3387, #3543 ) ;
#15767 = CARTESIAN_POINT ( 'NONE',  ( 58.45000000000001705, 0.8000000000000002665, 2.421260002560650104 ) ) ;
#15768 = DIRECTION ( 'NONE',  ( -3.170125418975226039E-16, 0.9428090415820620240, 0.3333333333333372561 ) ) ;
#15770 = CARTESIAN_POINT ( 'NONE',  ( 51.06584210772579269, -4.410482998349241512, 1.311567113538989693 ) ) ;
#15769 = CARTESIAN_POINT ( 'NONE',  ( 58.75000000000000000, 2.008165151418601191, 0.5380862305919300592 ) ) ;
#15771 = FACE_OUTER_BOUND ( 'NONE', #558, .T. ) ;
#15772 = LINE ( 'NONE', #7212, #21144 ) ;
#15773 = AXIS2_PLACEMENT_3D ( 'NONE', #11480, #21163, #30794 ) ;
#15774 = DIRECTION ( 'NONE',  ( 0.000000000000000000, 0.000000000000000000, 1.000000000000000000 ) ) ;
#15775 = ORIENTED_EDGE ( 'NONE', *, *, #31173, .F. ) ;
#15776 = CARTESIAN_POINT ( 'NONE',  ( 54.19008868793212486, 6.697828837789025158, -2.050000000000189004 ) ) ;
#15777 = ORIENTED_EDGE ( 'NONE', *, *, #29676, .T. ) ;
#15778 = ORIENTED_EDGE ( 'NONE', *, *, #15600, .T. ) ;
#15779 = EDGE_CURVE ( 'NONE', #23465, #6272, #10962, .T. ) ;
#15780 = CARTESIAN_POINT ( 'NONE',  ( 51.77007169719453117, -3.673656954000176889, 1.824471899732607261 ) ) ;
#15781 = EDGE_LOOP ( 'NONE', ( #17532, #8823, #25247, #12101 ) ) ;
#15782 = CARTESIAN_POINT ( 'NONE',  ( 53.81176349924878366, 5.730864617276189676, 2.049999999999812417 ) ) ;
#15783 = CARTESIAN_POINT ( 'NONE',  ( -58.34585481156723574, -2.489203624310587060, 2.804704140674918911 ) ) ;
#15785 = CARTESIAN_POINT ( 'NONE',  ( -35.85663232820584057, -3.426725943139567576, 3.937891353488737423 ) ) ;
#15784 = CARTESIAN_POINT ( 'NONE',  ( -44.49999999999997868, 8.366749974758269874E-15, -1.589829192029513996E-13 ) ) ;
#15786 = VERTEX_POINT ( 'NONE', #23955 ) ;
#15787 = CARTESIAN_POINT ( 'NONE',  ( 32.54912305740081990, 8.004110617865640265, -2.050000000000113509 ) ) ;
#15788 = DIRECTION ( 'NONE',  ( 1.000000000000000000, -0.000000000000000000, -1.047444401652940007E-14 ) ) ;
#15789 = ORIENTED_EDGE ( 'NONE', *, *, #17482, .T. ) ;
#15791 = DIRECTION ( 'NONE',  ( 0.000000000000000000, 0.9996898646859344595, 0.02490330187381124133 ) ) ;
#15790 = CARTESIAN_POINT ( 'NONE',  ( -59.35358983848620795, 2.308634493194285486, 1.301040651491357503 ) ) ;
#15792 = DIRECTION ( 'NONE',  ( 0.000000000000000000, 0.2008964009354147484, -0.9796124928211139560 ) ) ;
#15793 = ORIENTED_EDGE ( 'NONE', *, *, #14425, .T. ) ;
#15794 = DIRECTION ( 'NONE',  ( 1.000000000000000000, 1.047444401652940007E-14, 0.000000000000000000 ) ) ;
#15795 = EDGE_CURVE ( 'NONE', #1490, #24741, #4478, .T. ) ;
#15796 = CARTESIAN_POINT ( 'NONE',  ( -44.59999999999998721, 1.557046979865768677, 3.273565289174733106 ) ) ;
#15797 = FACE_OUTER_BOUND ( 'NONE', #14105, .T. ) ;
#15798 = LINE ( 'NONE', #4850, #1584 ) ;
#15799 = DIRECTION ( 'NONE',  ( 0.000000000000000000, 0.000000000000000000, 1.000000000000000000 ) ) ;
#15800 = ORIENTED_EDGE ( 'NONE', *, *, #18713, .F. ) ;
#15801 = EDGE_CURVE ( 'NONE', #4799, #12883, #28672, .T. ) ;
#15802 = LINE ( 'NONE', #16424, #14493 ) ;
#15803 = EDGE_CURVE ( 'NONE', #28731, #17704, #6934, .T. ) ;
#15804 = CIRCLE ( 'NONE', #2148, 4.600000000000036948 ) ;
#15805 = EDGE_CURVE ( 'NONE', #5852, #23537, #9474, .T. ) ;
#15806 = CARTESIAN_POINT ( 'NONE',  ( -54.86042740578361077, -0.7887156198831597465, 3.845940847736172952 ) ) ;
#15807 = CARTESIAN_POINT ( 'NONE',  ( 51.90000000000001279, -4.227689052994015206, 1.125730994152046582 ) ) ;
#15808 = DIRECTION ( 'NONE',  ( 0.000000000000000000, -2.168404344971008128E-16, -1.000000000000000000 ) ) ;
#15809 = CARTESIAN_POINT ( 'NONE',  ( 58.65838214097815495, -1.874774200233337185, 0.03350837198770668934 ) ) ;
#15810 = CARTESIAN_POINT ( 'NONE',  ( 33.97047170734846588, 8.288075094363309248, 2.049999999999882139 ) ) ;
#15811 = VERTEX_POINT ( 'NONE', #11914 ) ;
#15812 = CARTESIAN_POINT ( 'NONE',  ( 51.80000000000002558, 6.475000000000062705, 2.049999999999819522 ) ) ;
#15813 = ORIENTED_EDGE ( 'NONE', *, *, #30919, .T. ) ;
#15814 = FACE_OUTER_BOUND ( 'NONE', #1244, .T. ) ;
#15815 = CARTESIAN_POINT ( 'NONE',  ( -54.49999999999997868, 1.549999999999999600, 4.029888335921975262 ) ) ;
#15816 = VERTEX_POINT ( 'NONE', #21600 ) ;
#15817 = EDGE_LOOP ( 'NONE', ( #13196, #3706, #10576, #24429 ) ) ;
#15818 = DIRECTION ( 'NONE',  ( 1.000000000000000000, 0.000000000000000000, 0.000000000000000000 ) ) ;
#15819 = DIRECTION ( 'NONE',  ( -1.000000000000000000, -3.053848253006669023E-16, 2.042510438544995169E-16 ) ) ;
#15821 = CARTESIAN_POINT ( 'NONE',  ( 58.75000000000000711, 1.077297519403823234, 1.655311165517741268 ) ) ;
#15820 = CARTESIAN_POINT ( 'NONE',  ( 58.45000000000001705, -0.8000000000000000444, 3.499999999999999556 ) ) ;
#15822 = CARTESIAN_POINT ( 'NONE',  ( -57.29792740578360366, 3.330682475591789871, 0.6830477631804107164 ) ) ;
#15823 = CIRCLE ( 'NONE', #13272, 4.000000000000000000 ) ;
#15824 = EDGE_CURVE ( 'NONE', #15927, #3896, #31240, .T. ) ;
#15825 = CARTESIAN_POINT ( 'NONE',  ( -35.85663232820601820, -4.683225679163349753, -2.703237727951245173 ) ) ;
#15826 = APPLICATION_PROTOCOL_DEFINITION ( 'draft international standard', 'automotive_design', 1998, #17699 ) ;
#15827 = EDGE_CURVE ( 'NONE', #4176, #28914, #3887, .T. ) ;
#15828 = ORIENTED_EDGE ( 'NONE', *, *, #24625, .T. ) ;
#15829 = CARTESIAN_POINT ( 'NONE',  ( -60.82202994616204705, 2.078460969082646770, 3.599999999999791367 ) ) ;
#15830 = CARTESIAN_POINT ( 'NONE',  ( 51.80000000000001137, 8.700000000000107647, -2.050000000000180123 ) ) ;
#15831 = EDGE_CURVE ( 'NONE', #5422, #9091, #2722, .T. ) ;
#15832 = CYLINDRICAL_SURFACE ( 'NONE', #2014, 1.000000000000000000 ) ;
#15833 = CARTESIAN_POINT ( 'NONE',  ( 15.29384114148388285, -0.3980941177579011003, 5.199999998461580120 ) ) ;
#15834 = EDGE_CURVE ( 'NONE', #4977, #13516, #8762, .T. ) ;
#15835 = CARTESIAN_POINT ( 'NONE',  ( -54.68749999999998579, -3.399999999999991029, -2.060885718922576431E-13 ) ) ;
#15837 = DIRECTION ( 'NONE',  ( -0.9993908270190958731, 0.03489949670250092062, 3.490905158897711881E-15 ) ) ;
#15836 = LINE ( 'NONE', #6501, #14010 ) ;
#15838 = AXIS2_PLACEMENT_3D ( 'NONE', #27376, #15030, #773 ) ;
#15839 = CARTESIAN_POINT ( 'NONE',  ( 53.74977035838708161, 4.800378271572134814, -2.050000000000184119 ) ) ;
#15841 = DIRECTION ( 'NONE',  ( 0.000000000000000000, -1.000000000000000000, -3.491481338843135722E-15 ) ) ;
#15840 = LINE ( 'NONE', #27878, #8888 ) ;
#15842 = ORIENTED_EDGE ( 'NONE', *, *, #15594, .F. ) ;
#15843 = CARTESIAN_POINT ( 'NONE',  ( 54.40000000000001990, 0.000000000000000000, 0.000000000000000000 ) ) ;
#15844 = CARTESIAN_POINT ( 'NONE',  ( -36.14504829323104218, 2.228024565339449481, -4.927420728799193128 ) ) ;
#15846 = FACE_OUTER_BOUND ( 'NONE', #29396, .T. ) ;
#15845 = CARTESIAN_POINT ( 'NONE',  ( 58.65266784251149801, 1.792820108340006602, 0.5492726012753877951 ) ) ;
#15847 = DIRECTION ( 'NONE',  ( 1.000000000000000000, 1.047444401652940007E-14, -0.000000000000000000 ) ) ;
#15848 = ORIENTED_EDGE ( 'NONE', *, *, #11260, .T. ) ;
#15849 = CARTESIAN_POINT ( 'NONE',  ( 53.94065574304038080, 7.474792160838902966, 2.049999999999810196 ) ) ;
#15850 = CARTESIAN_POINT ( 'NONE',  ( 48.00000000000001421, -4.319730106884873244, -1.256953381662404778 ) ) ;
#15851 = ORIENTED_EDGE ( 'NONE', *, *, #27559, .F. ) ;
#15852 = CARTESIAN_POINT ( 'NONE',  ( 50.59602332238209499, 0.1408342061609076379, -0.8215393206232032286 ) ) ;
#15853 = ORIENTED_EDGE ( 'NONE', *, *, #3844, .F. ) ;
#15854 = EDGE_CURVE ( 'NONE', #24915, #10286, #2873, .T. ) ;
#15855 = CARTESIAN_POINT ( 'NONE',  ( 69.20000000000001705, 0.6441176470588244607, -1.707553061181374066 ) ) ;
#15856 = CARTESIAN_POINT ( 'NONE',  ( 51.24099374247646921, -1.086790822298242087, -1.208135181987622486 ) ) ;
#15857 = ORIENTED_EDGE ( 'NONE', *, *, #28854, .T. ) ;
#15858 = SURFACE_SIDE_STYLE ('',( #13628 ) ) ;
#15859 = EDGE_CURVE ( 'NONE', #6367, #7461, #3112, .T. ) ;
#15860 = DIRECTION ( 'NONE',  ( 1.000000000000000000, 2.586136946169074517E-16, -0.000000000000000000 ) ) ;
#15861 = CARTESIAN_POINT ( 'NONE',  ( -55.83155989232411542, -1.962990915244706924, -3.400000000000204636 ) ) ;
#15862 = ORIENTED_EDGE ( 'NONE', *, *, #29771, .T. ) ;
#15863 = CARTESIAN_POINT ( 'NONE',  ( 56.95641943120798345, 0.7163990203283279179, -1.759764883066090801 ) ) ;
#15864 = ADVANCED_FACE ( 'NONE', ( #17442 ), #5572, .F. ) ;
#15865 = ORIENTED_EDGE ( 'NONE', *, *, #20410, .F. ) ;
#15866 = CIRCLE ( 'NONE', #17384, 2.750000000000000444 ) ;
#15867 = VERTEX_POINT ( 'NONE', #27407 ) ;
#15868 = CARTESIAN_POINT ( 'NONE',  ( -55.81249999999997158, 3.925981830489463142, -1.840516183884902743E-13 ) ) ;
#15869 = CARTESIAN_POINT ( 'NONE',  ( 31.59287277085155665, 7.495449159457250765, -1.425000000000109956 ) ) ;
#15870 = FACE_OUTER_BOUND ( 'NONE', #19767, .T. ) ;
#15871 = CYLINDRICAL_SURFACE ( 'NONE', #9966, 0.1000000000000000472 ) ;
#15872 = EDGE_CURVE ( 'NONE', #21960, #11981, #15066, .T. ) ;
#15874 = CARTESIAN_POINT ( 'NONE',  ( 61.00000000000002842, -0.8666666666660278739, -1.374595900215364708 ) ) ;
#15873 = CARTESIAN_POINT ( 'NONE',  ( -69.19999999999998863, -6.931756715175872842E-16, 2.447411951356162049E-15 ) ) ;
#15875 = CARTESIAN_POINT ( 'NONE',  ( 47.10000000000002274, -4.276948333784438283, 0.9210526315789470120 ) ) ;
#15876 = CARTESIAN_POINT ( 'NONE',  ( -55.56249999999997158, -3.238593381231837043, -2.874284765127025576 ) ) ;
#15877 = CARTESIAN_POINT ( 'NONE',  ( 54.12540754135503107, 6.691802926424371023, 2.049999999999799538 ) ) ;
#15878 = CARTESIAN_POINT ( 'NONE',  ( -54.49999999999997868, 0.000000000000000000, 0.000000000000000000 ) ) ;
#15879 = AXIS2_PLACEMENT_3D ( 'NONE', #626, #12971, #10287 ) ;
#15880 = DIRECTION ( 'NONE',  ( 1.000000000000000000, 1.047444401652940007E-14, 0.000000000000000000 ) ) ;
#15881 = ORIENTED_EDGE ( 'NONE', *, *, #22889, .F. ) ;
#15882 = LINE ( 'NONE', #16054, #24220 ) ;
#15883 = ORIENTED_EDGE ( 'NONE', *, *, #19502, .T. ) ;
#15884 = AXIS2_PLACEMENT_3D ( 'NONE', #29565, #26580, #5346 ) ;
#15885 = DIRECTION ( 'NONE',  ( 0.000000000000000000, 0.2008964009354147207, -0.9796124928211139560 ) ) ;
#15886 = CARTESIAN_POINT ( 'NONE',  ( -54.93749999999998579, 1.962990915244722689, 3.399999999999812506 ) ) ;
#15887 = ORIENTED_EDGE ( 'NONE', *, *, #22419, .T. ) ;
#15888 = ORIENTED_EDGE ( 'NONE', *, *, #15215, .T. ) ;
#15889 = CARTESIAN_POINT ( 'NONE',  ( 51.68179902492697408, -4.249104741287451859, -1.767319601065211909 ) ) ;
#15890 = ORIENTED_EDGE ( 'NONE', *, *, #24864, .T. ) ;
#15891 = EDGE_CURVE ( 'NONE', #27521, #14166, #12968, .T. ) ;
#15892 = FACE_OUTER_BOUND ( 'NONE', #28032, .T. ) ;
#15893 =( BOUNDED_SURFACE ( )  B_SPLINE_SURFACE ( 3, 2, ( 
 ( #15186, #15666, #3623 ),
 ( #24837, #22945, #20585 ),
 ( #30219, #27373, #8526 ),
 ( #770, #18208, #12793 ),
 ( #22651, #20119, #5684 ),
 ( #15334, #24983, #9167 ),
 ( #18828, #6949, #15955 ),
 ( #4088, #20884, #11363 ),
 ( #23109, #9317, #1400 ),
 ( #6626, #6473, #25932 ) ),
 .UNSPECIFIED., .F., .F., .F. ) 
 B_SPLINE_SURFACE_WITH_KNOTS ( ( 4, 2, 2, 2, 4 ),
 ( 3, 3 ),
 ( 0.0002526260074104870901, 0.0003606909493797115550, 0.0004687558913489360741, 0.0006848857752873850581, 0.001117145543164283026 ),
 ( 0.000000000000000000, 1.000000000000000000 ),
 .UNSPECIFIED. ) 
 GEOMETRIC_REPRESENTATION_ITEM ( )  RATIONAL_B_SPLINE_SURFACE ( (
 ( 1.000000000000000000, 0.9842509842511785179, 1.000000000000000000),
 ( 1.000000000000000000, 0.9838268088398656186, 1.000000000000000000),
 ( 1.000000000000000000, 0.9731519947952637084, 1.000000000000000000),
 ( 1.000000000000000000, 0.9499473078865111608, 1.000000000000000000),
 ( 1.000000000000000000, 0.9371632344323043151, 1.000000000000000000),
 ( 1.000000000000000000, 0.8981767195496317413, 1.000000000000000000),
 ( 1.000000000000000000, 0.8714317066438567183, 1.000000000000000000),
 ( 1.000000000000000000, 0.7945716934681402721, 1.000000000000000000),
 ( 1.000000000000000000, 0.7462340517456830247, 1.000000000000000000),
 ( 1.000000000000000000, 0.7071067811865260344, 1.000000000000000000) ) ) 
 REPRESENTATION_ITEM ( '' )  SURFACE ( )  );
#15894 = ORIENTED_EDGE ( 'NONE', *, *, #5431, .T. ) ;
#15895 = CARTESIAN_POINT ( 'NONE',  ( 51.25000000000002842, -0.7499999999994634292, 1.718465885608440269 ) ) ;
#15896 = DIRECTION ( 'NONE',  ( -1.000000000000000000, -3.053848253006669023E-16, 2.042510438544995415E-16 ) ) ;
#15897 = AXIS2_PLACEMENT_3D ( 'NONE', #2766, #22113, #403 ) ;
#15898 = B_SPLINE_CURVE_WITH_KNOTS ( 'NONE', 3,
 ( #30114, #27130, #13180, #8278 ),
 .UNSPECIFIED., .F., .F.,
 ( 4, 4 ),
 ( 0.000000000000000000, 1.346394374510315309E-05 ),
 .UNSPECIFIED. ) ;
#15899 = DIRECTION ( 'NONE',  ( -1.000000000000000000, 1.219044193948983948E-29, -3.491481338843133355E-15 ) ) ;
#15900 = ORIENTED_EDGE ( 'NONE', *, *, #21553, .T. ) ;
#15901 = DIRECTION ( 'NONE',  ( 0.000000000000000000, -0.9996898646859343485, -0.02490330187381124133 ) ) ;
#15903 = CARTESIAN_POINT ( 'NONE',  ( 51.31572262954149011, 1.002608958138273554, -1.395204572094392637 ) ) ;
#15902 = VECTOR ( 'NONE', #5659, 1000.000000000000000 ) ;
#15904 = CARTESIAN_POINT ( 'NONE',  ( 51.87416143049283335, 8.598705507415685290, -1.950000000000180256 ) ) ;
#15905 = CARTESIAN_POINT ( 'NONE',  ( 15.03925126672132961, 4.018128179617504792, 3.618665901676689778 ) ) ;
#15906 = EDGE_CURVE ( 'NONE', #11471, #10732, #20594, .T. ) ;
#15907 = CARTESIAN_POINT ( 'NONE',  ( 48.46963600013424411, 1.366688880095624503, 3.854642372925540350 ) ) ;
#15908 = TOROIDAL_SURFACE ( 'NONE', #24019, 4.275000000000000355, 0.1000000000000000056 ) ;
#15909 = CARTESIAN_POINT ( 'NONE',  ( 50.87477060347374902, 8.633605004118187765, 1.949999999999822320 ) ) ;
#15911 = CARTESIAN_POINT ( 'NONE',  ( 51.58853050958410336, -4.227727696248162026, 1.816297733665127812 ) ) ;
#15910 = CARTESIAN_POINT ( 'NONE',  ( 52.20711756518984714, -0.7499999999994533262, 1.718465885608439603 ) ) ;
#15912 = CARTESIAN_POINT ( 'NONE',  ( 46.90000000000001279, 1.734723475976807094E-15, 0.000000000000000000 ) ) ;
#15913 = CARTESIAN_POINT ( 'NONE',  ( 59.00000000000002132, 1.401298464324817071E-42, -6.179921969752347932E-13 ) ) ;
#15914 = DIRECTION ( 'NONE',  ( -1.000000000000000000, 0.000000000000000000, 1.047444401652940007E-14 ) ) ;
#15915 = ORIENTED_EDGE ( 'NONE', *, *, #45, .T. ) ;
#15916 = AXIS2_PLACEMENT_3D ( 'NONE', #23220, #25739, #18467 ) ;
#15917 = DIRECTION ( 'NONE',  ( 9.329605248950888974E-15, -1.000000000000000000, 0.000000000000000000 ) ) ;
#15918 = ORIENTED_EDGE ( 'NONE', *, *, #19908, .F. ) ;
#15919 = CARTESIAN_POINT ( 'NONE',  ( 51.80000000000003268, -3.700421601131613780, 1.984561589293431405 ) ) ;
#15920 = EDGE_LOOP ( 'NONE', ( #11317, #5647 ) ) ;
#15921 = CARTESIAN_POINT ( 'NONE',  ( 51.80000000000002558, 8.700707106781294442, 2.049999999999819522 ) ) ;
#15922 = AXIS2_PLACEMENT_3D ( 'NONE', #3569, #8304, #17972 ) ;
#15923 = CARTESIAN_POINT ( 'NONE',  ( -56.34585481156723574, 3.673546848079182858, 0.7533615035078061739 ) ) ;
#15925 = FACE_OUTER_BOUND ( 'NONE', #1703, .T. ) ;
#15924 = CARTESIAN_POINT ( 'NONE',  ( 61.25000000000003553, -0.9999999999993586242, 1.586072192556190252 ) ) ;
#15926 = ORIENTED_EDGE ( 'NONE', *, *, #23161, .F. ) ;
#15927 = VERTEX_POINT ( 'NONE', #22685 ) ;
#15928 = CARTESIAN_POINT ( 'NONE',  ( 26.61278927081361090, 5.319531372976052275, -2.050000000000092637 ) ) ;
#15929 = ADVANCED_FACE ( 'NONE', ( #15369 ), #24722, .F. ) ;
#15930 = B_SPLINE_CURVE_WITH_KNOTS ( 'NONE', 3,
 ( #28971, #16949, #24231, #20846, #10852, #27951 ),
 .UNSPECIFIED., .F., .F.,
 ( 4, 2, 4 ),
 ( 0.000000000000000000, 0.0001000270069604649562, 0.0002000540139209299123 ),
 .UNSPECIFIED. ) ;
#15931 = CARTESIAN_POINT ( 'NONE',  ( -67.99999999999997158, -3.266925685480240183E-16, 2.202315069465531314E-15 ) ) ;
#15932 = EDGE_LOOP ( 'NONE', ( #16138, #6726, #4706, #13824 ) ) ;
#15934 = DIRECTION ( 'NONE',  ( -1.000000000000000000, -0.000000000000000000, 0.000000000000000000 ) ) ;
#15933 = FACE_BOUND ( 'NONE', #21957, .T. ) ;
#15935 = AXIS2_PLACEMENT_3D ( 'NONE', #3020, #8087, #484 ) ;
#15936 = FACE_OUTER_BOUND ( 'NONE', #27113, .T. ) ;
#15937 = ORIENTED_EDGE ( 'NONE', *, *, #7484, .T. ) ;
#15938 = LINE ( 'NONE', #11196, #27287 ) ;
#15939 = DIRECTION ( 'NONE',  ( 0.000000000000000000, 0.000000000000000000, 1.000000000000000000 ) ) ;
#15940 = DIRECTION ( 'NONE',  ( -1.000000000000000000, -0.000000000000000000, -0.000000000000000000 ) ) ;
#15941 = CARTESIAN_POINT ( 'NONE',  ( 57.02114944868134216, 0.7500000000000000000, 1.778342400449481442 ) ) ;
#15942 = CARTESIAN_POINT ( 'NONE',  ( -56.63452994616203284, 2.093608279459369510E-14, -3.600000000000201261 ) ) ;
#15943 = AXIS2_PLACEMENT_3D ( 'NONE', #9071, #18746, #28386 ) ;
#15944 = TOROIDAL_SURFACE ( 'NONE', #21539, 1.302039949377232331, 0.05000000000000000278 ) ;
#15945 = EDGE_CURVE ( 'NONE', #11521, #18051, #27145, .T. ) ;
#15946 = CARTESIAN_POINT ( 'NONE',  ( 15.56401610563799487, 3.953723660658996497, 3.694477770903627167 ) ) ;
#15947 = AXIS2_PLACEMENT_3D ( 'NONE', #21472, #31107, #19101 ) ;
#15948 = CIRCLE ( 'NONE', #27568, 0.4600000000000000755 ) ;
#15949 = CARTESIAN_POINT ( 'NONE',  ( -58.79792740578360366, 3.330682475591788982, 0.6830477631804159344 ) ) ;
#15950 = CARTESIAN_POINT ( 'NONE',  ( -56.84585481156722864, -2.489203624310586616, 2.804704140674918467 ) ) ;
#15951 =( BOUNDED_CURVE ( )  B_SPLINE_CURVE ( 3, ( #27575, #30269, #15856, #1288 ),
 .UNSPECIFIED., .F., .T. ) 
 B_SPLINE_CURVE_WITH_KNOTS ( ( 4, 4 ),
 ( 0.8272220676012502771, 0.8437250283369835957 ),
 .UNSPECIFIED. ) 
 CURVE ( )  GEOMETRIC_REPRESENTATION_ITEM ( )  RATIONAL_B_SPLINE_CURVE ( ( 1.000000000000000000, 0.9999773044860189586, 0.9999773044860189586, 1.000000000000000000 ) ) 
 REPRESENTATION_ITEM ( '' )  );
#15952 = EDGE_CURVE ( 'NONE', #22807, #21791, #17610, .T. ) ;
#15953 = LINE ( 'NONE', #23260, #24094 ) ;
#15954 = FACE_OUTER_BOUND ( 'NONE', #18876, .T. ) ;
#15955 = CARTESIAN_POINT ( 'NONE',  ( 48.33019736648184050, 1.141995257496368987, -3.938405479918978713 ) ) ;
#15956 = EDGE_LOOP ( 'NONE', ( #24323, #27223, #25435, #30814 ) ) ;
#15957 = CARTESIAN_POINT ( 'NONE',  ( -44.59999999999998010, -2.649999999999991918, -1.685844928847700321E-13 ) ) ;
#15958 = ORIENTED_EDGE ( 'NONE', *, *, #17729, .T. ) ;
#15959 = CARTESIAN_POINT ( 'NONE',  ( 58.66054497608050866, 0.5000000000006143974, -1.807104036850122109 ) ) ;
#15961 = LINE ( 'NONE', #15815, #8579 ) ;
#15960 = DIRECTION ( 'NONE',  ( 1.000000000000000000, -1.219044193948983948E-29, 3.491481338843133355E-15 ) ) ;
#15962 = VERTEX_POINT ( 'NONE', #10020 ) ;
#15963 = AXIS2_PLACEMENT_3D ( 'NONE', #8994, #11536, #18664 ) ;
#15964 = FACE_OUTER_BOUND ( 'NONE', #29193, .T. ) ;
#15965 = VECTOR ( 'NONE', #21905, 1000.000000000000114 ) ;
#15966 = EDGE_CURVE ( 'NONE', #30566, #11854, #4389, .T. ) ;
#15967 = CARTESIAN_POINT ( 'NONE',  ( 58.50000000000001421, -0.8000000000000000444, -1.778341924377873751 ) ) ;
#15969 = CARTESIAN_POINT ( 'NONE',  ( 58.75000000000000711, 1.877732920581777432, -0.6121634413828938026 ) ) ;
#15968 = CYLINDRICAL_SURFACE ( 'NONE', #18586, 0.05000000000000143219 ) ;
#15970 = VERTEX_POINT ( 'NONE', #14896 ) ;
#15971 = CARTESIAN_POINT ( 'NONE',  ( -56.67292740578360366, 2.256877952708269408, -2.542931754211925188 ) ) ;
#15972 = ADVANCED_FACE ( 'NONE', ( #24558 ), #13978, .F. ) ;
#15973 = AXIS2_PLACEMENT_3D ( 'NONE', #20385, #30173, #30007 ) ;
#15974 = DIRECTION ( 'NONE',  ( -2.614381936396368743E-16, 0.2008964009354147762, -0.9796124928211139560 ) ) ;
#15975 = SHAPE_DEFINITION_REPRESENTATION ( #12824, #27890 ) ;
#15976 = CIRCLE ( 'NONE', #2334, 4.375000000000000000 ) ;
#15977 = VECTOR ( 'NONE', #13288, 1000.000000000000000 ) ;
#15978 = CARTESIAN_POINT ( 'NONE',  ( 53.73313642785004873, 5.556167542617246546, -1.667742524038318352 ) ) ;
#15979 = AXIS2_PLACEMENT_3D ( 'NONE', #24447, #29357, #24760 ) ;
#15980 = CARTESIAN_POINT ( 'NONE',  ( 25.68808851933979298, 5.234409799644741845, 1.949999999999910916 ) ) ;
#15981 = ORIENTED_EDGE ( 'NONE', *, *, #22449, .T. ) ;
#15982 = EDGE_CURVE ( 'NONE', #5897, #30927, #12529, .T. ) ;
#15983 = AXIS2_PLACEMENT_3D ( 'NONE', #16182, #4138, #13725 ) ;
#15984 = CARTESIAN_POINT ( 'NONE',  ( -54.49999999999999289, 1.499999999999995781, 4.029888335921750553 ) ) ;
#15985 = CARTESIAN_POINT ( 'NONE',  ( -36.68866260399369139, 3.738196885377705225, -3.908481927057698257 ) ) ;
#15986 = CARTESIAN_POINT ( 'NONE',  ( -59.35162536475819905, 3.281785115337339409, 1.250136525132572451 ) ) ;
#15987 = FACE_OUTER_BOUND ( 'NONE', #25007, .T. ) ;
#15988 = AXIS2_PLACEMENT_3D ( 'NONE', #3110, #12756, #20073 ) ;
#15989 = DIRECTION ( 'NONE',  ( 1.000000000000000000, 3.053848253006669023E-16, -2.042510438544995415E-16 ) ) ;
#15990 = AXIS2_PLACEMENT_3D ( 'NONE', #26331, #31066, #11762 ) ;
#15992 = DIRECTION ( 'NONE',  ( 1.000000000000000000, -1.219044193948983948E-29, 3.491481338843133355E-15 ) ) ;
#15991 = CARTESIAN_POINT ( 'NONE',  ( 58.45000000000001705, -0.7500000000000000000, 2.421260002560649660 ) ) ;
#15994 = EDGE_CURVE ( 'NONE', #6668, #14986, #22106, .T. ) ;
#15993 =( GEOMETRIC_REPRESENTATION_CONTEXT ( 3 ) GLOBAL_UNCERTAINTY_ASSIGNED_CONTEXT ( ( #10746 ) ) GLOBAL_UNIT_ASSIGNED_CONTEXT ( ( #30587, #16354, #6693 ) ) REPRESENTATION_CONTEXT ( 'NONE', 'WORKASPACE' ) );
#15995 = DIRECTION ( 'NONE',  ( -1.000000000000000000, 0.000000000000000000, 1.047444401652940007E-14 ) ) ;
#15996 = AXIS2_PLACEMENT_3D ( 'NONE', #19142, #16756, #12151 ) ;
#15998 = DIRECTION ( 'NONE',  ( -1.000000000000000000, 0.000000000000000000, 1.047444401652940007E-14 ) ) ;
#15997 = LINE ( 'NONE', #26132, #26127 ) ;
#15999 = ORIENTED_EDGE ( 'NONE', *, *, #2830, .F. ) ;
#16000 = AXIS2_PLACEMENT_3D ( 'NONE', #18854, #4432, #6494 ) ;
#16001 = CARTESIAN_POINT ( 'NONE',  ( -62.05596007256994540, -2.671012538737645770, -0.3731730811386074209 ) ) ;
#16002 = AXIS2_PLACEMENT_3D ( 'NONE', #16200, #6690, #7022 ) ;
#16003 = FACE_OUTER_BOUND ( 'NONE', #20636, .T. ) ;
#16005 = CARTESIAN_POINT ( 'NONE',  ( 51.80000000000001137, 4.350000000000017408, -2.050000000000180123 ) ) ;
#16004 = CARTESIAN_POINT ( 'NONE',  ( 58.72427158855717266, 1.822388627307728992, 0.4415141953931043806 ) ) ;
#16006 = CARTESIAN_POINT ( 'NONE',  ( -35.85663232820584057, 0.000000000000000000, 5.200000000000000178 ) ) ;
#16007 = ORIENTED_EDGE ( 'NONE', *, *, #13390, .T. ) ;
#16008 = CARTESIAN_POINT ( 'NONE',  ( 51.87765138016309407, 8.698644590117595499, 2.049999999999819522 ) ) ;
#16009 = CARTESIAN_POINT ( 'NONE',  ( 50.38147505302056572, -1.153996415704667156, 3.890257736381617537 ) ) ;
#16010 = ADVANCED_FACE ( 'NONE', ( #28316 ), #13874, .T. ) ;
#16011 = ORIENTED_EDGE ( 'NONE', *, *, #7264, .T. ) ;
#16012 = ADVANCED_FACE ( 'NONE', ( #16286 ), #8431, .F. ) ;
#16013 = CARTESIAN_POINT ( 'NONE',  ( 64.25000000000001421, 1.163569835200988601E-28, -2.243276760206714411E-13 ) ) ;
#16014 = AXIS2_PLACEMENT_3D ( 'NONE', #23586, #16626, #6638 ) ;
#16015 = ORIENTED_EDGE ( 'NONE', *, *, #1528, .F. ) ;
#16016 = EDGE_CURVE ( 'NONE', #19416, #26766, #4232, .T. ) ;
#16017 = CIRCLE ( 'NONE', #3368, 10.00000000000000178 ) ;
#16018 = DIRECTION ( 'NONE',  ( 3.016910393003118404E-15, 0.000000000000000000, 1.000000000000000000 ) ) ;
#16019 = CARTESIAN_POINT ( 'NONE',  ( 51.23644008536121675, 1.080112125196981410, -1.214076932077873039 ) ) ;
#16020 = ORIENTED_EDGE ( 'NONE', *, *, #27958, .F. ) ;
#16021 = CIRCLE ( 'NONE', #24634, 0.09999999999999988065 ) ;
#16022 = DIRECTION ( 'NONE',  ( 0.000000000000000000, 1.000000000000000000, 0.000000000000000000 ) ) ;
#16023 = CARTESIAN_POINT ( 'NONE',  ( -58.08155989232410832, -1.962990915244706924, -3.400000000000212630 ) ) ;
#16024 = ORIENTED_EDGE ( 'NONE', *, *, #26043, .T. ) ;
#16025 = AXIS2_PLACEMENT_3D ( 'NONE', #16, #12048, #17257 ) ;
#16026 = CARTESIAN_POINT ( 'NONE',  ( 58.45000000000001705, -0.8000000000000002665, 2.421260002560650104 ) ) ;
#16027 = VERTEX_POINT ( 'NONE', #1124 ) ;
#16028 = EDGE_LOOP ( 'NONE', ( #14272, #17376, #20407, #30106 ) ) ;
#16029 = CLOSED_SHELL ( 'NONE', ( #13105, #17637, #28536, #7296, #17786, #15864, #5037, #16796, #22012, #6728, #26848, #22163, #16610, #14153, #10774, #16954, #27871, #18136, #17941, #17632, #25251, #4508, #9278, #28956, #16440, #17307, #15929, #370, #15731, #2142, #18955, #12954, #20686, #16961, #19304, #25408, #30123, #28376, #13933, #1201, #25373, #443, #599, #23446, #25387, #30262, #14469, #15206, #21231, #30060, #24373, #29944, #10963, #17815, #30474, #5288, #19726, #16999, #20462, #5475, #12964, #11658, #25309, #23711, #21065, #6489, #23645, #7550, #21078, #2649, #14169, #14236, #18243, #30710, #1985, #2139, #24133, #28168, #18470, #12169, #939, #17809, #9312, #18025, #30096, #14994, #13488, #25803, #11798, #4585, #29633, #1908, #16012, #4853, #217, #24700, #30987, #15387, #835, #284, #11589, #25978, #906, #18317, #3668, #25410, #3284, #10753, #22769, #17879, #29337, #20638, #18416, #13749, #20832, #6475, #11211, #7327, #9093, #11730, #20418, #9049, #12748, #17749, #25947, #17686, #27981, #14321, #892, #26752, #16380, #24478, #923, #9776, #4911, #2503, #29937, #27303, #16050, #14266, #30198, #3290, #24425, #23566, #7895, #1114, #17844, #17362, #15077, #26418, #26783, #22200, #29000, #16199, #29973, #4643, #22220, #16229, #29882, #30890, #16109, #1725, #19149, #15407, #5309, #30671, #12227, #13458, #9611, #23850, #6215, #30503, #8745, #6415 ) ) ;
#16030 = CIRCLE ( 'NONE', #17479, 0.1500000000000001887 ) ;
#16031 = CARTESIAN_POINT ( 'NONE',  ( -56.74999999999995737, 2.023778652682507474E-14, -3.400000000000201972 ) ) ;
#16032 = AXIS2_PLACEMENT_3D ( 'NONE', #15913, #13540, #25421 ) ;
#16033 = CIRCLE ( 'NONE', #21096, 0.2500000000000000000 ) ;
#16034 = CARTESIAN_POINT ( 'NONE',  ( 56.96751809705963154, -0.7713737938325972987, 2.482938273535672646 ) ) ;
#16035 = LINE ( 'NONE', #16681, #4117 ) ;
#16036 = CARTESIAN_POINT ( 'NONE',  ( 36.50000000000002132, 2.326828918379971365E-16, 1.899999999999999911 ) ) ;
#16037 = DIRECTION ( 'NONE',  ( 1.000000000000000000, 3.053848253006669023E-16, -2.042510438544995415E-16 ) ) ;
#16039 = DIRECTION ( 'NONE',  ( 3.016910393003118404E-15, 0.000000000000000000, 1.000000000000000000 ) ) ;
#16038 = FACE_OUTER_BOUND ( 'NONE', #11748, .T. ) ;
#16040 = VECTOR ( 'NONE', #16044, 1000.000000000000000 ) ;
#16041 = EDGE_CURVE ( 'NONE', #22264, #23376, #29165, .T. ) ;
#16042 = AXIS2_PLACEMENT_3D ( 'NONE', #9659, #12023, #21530 ) ;
#16043 = DIRECTION ( 'NONE',  ( 0.000000000000000000, 0.000000000000000000, 1.000000000000000000 ) ) ;
#16044 = DIRECTION ( 'NONE',  ( 3.491481338843133355E-15, 3.491481338843133355E-15, -1.000000000000000000 ) ) ;
#16045 = EDGE_CURVE ( 'NONE', #30038, #2131, #22835, .T. ) ;
#16046 = DIRECTION ( 'NONE',  ( 0.000000000000000000, 0.000000000000000000, 1.000000000000000000 ) ) ;
#16047 = CARTESIAN_POINT ( 'NONE',  ( -59.67203891626250112, -2.203043321329347215, 1.525444001725758447 ) ) ;
#16049 = CARTESIAN_POINT ( 'NONE',  ( -59.52340461522653925, 2.130728629699490284, 1.584472915547397776 ) ) ;
#16048 = AXIS2_PLACEMENT_3D ( 'NONE', #19233, #18318, #4790 ) ;
#16050 = ADVANCED_FACE ( 'NONE', ( #28469 ), #6771, .T. ) ;
#16051 = DIRECTION ( 'NONE',  ( 0.000000000000000000, 0.000000000000000000, 1.000000000000000000 ) ) ;
#16052 = VERTEX_POINT ( 'NONE', #15698 ) ;
#16054 = CARTESIAN_POINT ( 'NONE',  ( 51.89161117884420094, 9.098400920928357394, 1.949999999999818767 ) ) ;
#16053 = FACE_OUTER_BOUND ( 'NONE', #26318, .T. ) ;
#16055 = CARTESIAN_POINT ( 'NONE',  ( -36.79682133506354091, -0.5584590966806997070, -5.380195666604552507 ) ) ;
#16056 = AXIS2_PLACEMENT_3D ( 'NONE', #24357, #2669, #16775 ) ;
#16057 = ORIENTED_EDGE ( 'NONE', *, *, #13490, .F. ) ;
#16058 = VECTOR ( 'NONE', #9280, 1000.000000000000000 ) ;
#16059 = CIRCLE ( 'NONE', #9506, 0.09999999999999933942 ) ;
#16060 = CARTESIAN_POINT ( 'NONE',  ( 51.27141371434416328, 0.9996500697957936277, 1.586307688445277586 ) ) ;
#16061 = FACE_OUTER_BOUND ( 'NONE', #28521, .T. ) ;
#16062 = CARTESIAN_POINT ( 'NONE',  ( -57.99999999999997868, 2.944486372867092250, 1.699999999999805667 ) ) ;
#16063 = ORIENTED_EDGE ( 'NONE', *, *, #31135, .T. ) ;
#16064 = ORIENTED_EDGE ( 'NONE', *, *, #9646, .T. ) ;
#16065 = CARTESIAN_POINT ( 'NONE',  ( 58.75000000000002842, -1.077297519403983106, -1.655311165516836436 ) ) ;
#16066 = VERTEX_POINT ( 'NONE', #30083 ) ;
#16067 = CARTESIAN_POINT ( 'NONE',  ( 58.72419296898096519, -1.645806614394166534, 0.8985315506029413202 ) ) ;
#16068 = CARTESIAN_POINT ( 'NONE',  ( -69.22071067811863543, -6.995007661688606141E-16, 2.451642053546763754E-15 ) ) ;
#16069 = VERTEX_POINT ( 'NONE', #8400 ) ;
#16070 = CARTESIAN_POINT ( 'NONE',  ( 24.17629218420043102, 5.599093920765165322, -1.950000000000019273 ) ) ;
#16071 = DIRECTION ( 'NONE',  ( 1.000000000000000000, 0.000000000000000000, -1.047444401652940007E-14 ) ) ;
#16072 = CIRCLE ( 'NONE', #29711, 0.2499999999999987788 ) ;
#16073 = DIRECTION ( 'NONE',  ( 0.000000000000000000, 0.000000000000000000, -1.000000000000000000 ) ) ;
#16074 = VERTEX_POINT ( 'NONE', #18086 ) ;
#16075 = VERTEX_POINT ( 'NONE', #27728 ) ;
#16076 = AXIS2_PLACEMENT_3D ( 'NONE', #4882, #23748, #2040 ) ;
#16077 = AXIS2_PLACEMENT_3D ( 'NONE', #9823, #19490, #29138 ) ;
#16078 = LINE ( 'NONE', #30620, #11203 ) ;
#16079 = APPLICATION_CONTEXT ( 'automotive_design' ) ;
#16080 = CARTESIAN_POINT ( 'NONE',  ( 15.71019289815287934, -0.8926979523208187217, 5.334280177567952919 ) ) ;
#16081 = CARTESIAN_POINT ( 'NONE',  ( 51.25879181974310939, -0.9981351195451134695, 1.403212705160382212 ) ) ;
#16082 = CARTESIAN_POINT ( 'NONE',  ( 58.45000000000001705, -0.8000000000000000444, 2.471260002560649927 ) ) ;
#16083 = DIRECTION ( 'NONE',  ( 0.000000000000000000, 0.000000000000000000, 1.000000000000000000 ) ) ;
#16084 = DIRECTION ( 'NONE',  ( 1.000000000000000000, 3.054025858079668409E-16, -2.042474015755241579E-16 ) ) ;
#16085 = DIRECTION ( 'NONE',  ( 1.000000000000000000, 1.047444401652940007E-14, 0.000000000000000000 ) ) ;
#16087 = CARTESIAN_POINT ( 'NONE',  ( 51.77958208625742031, -4.146195171498040288, 1.996297985640307360 ) ) ;
#16086 = CARTESIAN_POINT ( 'NONE',  ( -36.76447480099788123, -2.670851142931307542, 4.702170608191340584 ) ) ;
#16088 = B_SPLINE_CURVE_WITH_KNOTS ( 'NONE', 3,
 ( #14557, #26430, #24222, #16786 ),
 .UNSPECIFIED., .F., .F.,
 ( 4, 4 ),
 ( 0.000000000000000000, 0.0001493943817025057165 ),
 .UNSPECIFIED. ) ;
#16089 = EDGE_CURVE ( 'NONE', #10599, #15131, #19578, .T. ) ;
#16090 = CARTESIAN_POINT ( 'NONE',  ( 51.80000000000001137, -4.144729964592930749, 1.074323956811003011 ) ) ;
#16091 = EDGE_CURVE ( 'NONE', #8907, #24531, #23046, .T. ) ;
#16092 = B_SPLINE_CURVE_WITH_KNOTS ( 'NONE', 3,
 ( #992, #24736, #12839, #12692, #1137, #6203, #8261, #29632, #17927, #7958, #13013, #18252, #10788, #22521, #25206, #8417 ),
 .UNSPECIFIED., .F., .F.,
 ( 4, 3, 3, 3, 3, 4 ),
 ( 0.000000000000000000, 3.304654905549463427E-05, 6.654308848431682766E-05, 0.0001011328993923933043, 0.0001374176636839670798, 0.0001650454644847091615 ),
 .UNSPECIFIED. ) ;
#16093 = PLANE ( 'NONE',  #20123 ) ;
#16094 = CARTESIAN_POINT ( 'NONE',  ( 58.75000000000000711, 1.320082690053780983, 1.469015551797191010 ) ) ;
#16095 = CARTESIAN_POINT ( 'NONE',  ( 48.40000000000001990, 0.6304760106459513791, -3.950000000000022826 ) ) ;
#16096 = ORIENTED_EDGE ( 'NONE', *, *, #5681, .T. ) ;
#16097 = TOROIDAL_SURFACE ( 'NONE', #13543, 1.975000000000001865, 0.1000000000000000056 ) ;
#16098 = EDGE_LOOP ( 'NONE', ( #21278, #16131, #29904, #14235 ) ) ;
#16099 = CARTESIAN_POINT ( 'NONE',  ( 58.75000000000002132, 6.153735859711025284E-13, 3.111507638930570854E-58 ) ) ;
#16100 =( BOUNDED_CURVE ( )  B_SPLINE_CURVE ( 2, ( #13183, #20194, #20496, #1157, #7988, #5924, #20021, #17807, #17651 ),
 .UNSPECIFIED., .F., .T. ) 
 B_SPLINE_CURVE_WITH_KNOTS ( ( 3, 2, 2, 2, 3 ),
 ( 0.4166666666666666852, 0.4259259259259259300, 0.4444444444444444198, 0.4629629629629629650, 0.4722222222222222099 ),
 .UNSPECIFIED. ) 
 CURVE ( )  GEOMETRIC_REPRESENTATION_ITEM ( )  RATIONAL_B_SPLINE_CURVE ( ( 0.9330127018922194093, 0.9330127018922195203, 1.000000000000000000, 0.8660254037844387076, 1.000000000000000000, 0.8660254037844387076, 1.000000000000000000, 0.9330127018922194093, 0.9330127018922194093 ) ) 
 REPRESENTATION_ITEM ( '' )  );
#16101 = ORIENTED_EDGE ( 'NONE', *, *, #24967, .T. ) ;
#16102 = CARTESIAN_POINT ( 'NONE',  ( 53.25573957143296155, 8.250120694359615925, 2.049999999999814193 ) ) ;
#16103 = CARTESIAN_POINT ( 'NONE',  ( -58.90835481156722864, -3.238593381231842816, -2.874284765127022023 ) ) ;
#16105 = CARTESIAN_POINT ( 'NONE',  ( -36.22818246778668794, 3.722599991951159648, 3.938370952810205772 ) ) ;
#16104 = CARTESIAN_POINT ( 'NONE',  ( 58.75000000000000711, 1.077297519403823678, 1.655311165517741490 ) ) ;
#16106 = VERTEX_POINT ( 'NONE', #7730 ) ;
#16107 = ORIENTED_EDGE ( 'NONE', *, *, #10869, .T. ) ;
#16108 = CARTESIAN_POINT ( 'NONE',  ( 23.93173257309099000, 5.810883422836172763, -2.050000000000082423 ) ) ;
#16109 = ADVANCED_FACE ( 'NONE', ( #19786 ), #20105, .T. ) ;
#16110 = DIRECTION ( 'NONE',  ( -1.000000000000000000, 0.000000000000000000, 0.000000000000000000 ) ) ;
#16111 = ORIENTED_EDGE ( 'NONE', *, *, #6365, .T. ) ;
#16113 = CARTESIAN_POINT ( 'NONE',  ( -71.49999999999998579, -1.395601618875910821E-15, 2.917180974979867506E-15 ) ) ;
#16112 = DIRECTION ( 'NONE',  ( 0.000000000000000000, 0.2008964009354147762, -0.9796124928211140670 ) ) ;
#16114 = CARTESIAN_POINT ( 'NONE',  ( 51.87673771347595419, 8.672480599449029270, -2.050000000000180567 ) ) ;
#16115 = VERTEX_POINT ( 'NONE', #25561 ) ;
#16116 = CARTESIAN_POINT ( 'NONE',  ( -36.89250464418361020, 5.233646053067060322, -1.367284724151316189 ) ) ;
#16117 = FACE_BOUND ( 'NONE', #11299, .T. ) ;
#16118 = DIRECTION ( 'NONE',  ( 0.000000000000000000, 0.000000000000000000, 1.000000000000000000 ) ) ;
#16119 = LINE ( 'NONE', #21202, #93 ) ;
#16120 = CARTESIAN_POINT ( 'NONE',  ( -58.69702994616204705, 4.156921938165313080, -1.932741547809596393E-13 ) ) ;
#16121 = CIRCLE ( 'NONE', #24217, 0.2500000000000000000 ) ;
#16122 = AXIS2_PLACEMENT_3D ( 'NONE', #2906, #22083, #17316 ) ;
#16123 = AXIS2_PLACEMENT_3D ( 'NONE', #29750, #15333, #15501 ) ;
#16124 = DIRECTION ( 'NONE',  ( 1.000000000000000000, 1.047444401652940007E-14, 0.000000000000000000 ) ) ;
#16125 = CARTESIAN_POINT ( 'NONE',  ( -59.17292740578360366, -3.330682475591780101, -0.6830477631804271477 ) ) ;
#16126 = EDGE_CURVE ( 'NONE', #2006, #320, #8357, .T. ) ;
#16127 = CARTESIAN_POINT ( 'NONE',  ( -55.95655989232413674, -3.399999999999990585, -2.144552914728849520E-13 ) ) ;
#16128 = CARTESIAN_POINT ( 'NONE',  ( -54.44999999999997442, -1.499999999999999556, 4.029888335921975262 ) ) ;
#16129 = CARTESIAN_POINT ( 'NONE',  ( -36.22955757456081471, 0.2668145608218083775, 5.199999998579032834 ) ) ;
#16130 = CARTESIAN_POINT ( 'NONE',  ( -64.28602961791190751, 2.263268244922573835, 0.05638033785850931484 ) ) ;
#16131 = ORIENTED_EDGE ( 'NONE', *, *, #19611, .F. ) ;
#16132 = CARTESIAN_POINT ( 'NONE',  ( 58.75000000000000711, 1.749377236609743091, 0.8979909453705852140 ) ) ;
#16133 = EDGE_LOOP ( 'NONE', ( #19206, #26306, #11364, #3867 ) ) ;
#16134 = PRESENTATION_STYLE_ASSIGNMENT (( #30373 ) ) ;
#16136 = CARTESIAN_POINT ( 'NONE',  ( -59.51024032614731851, 3.088598804228899652, 1.421463128792039843 ) ) ;
#16135 = CYLINDRICAL_SURFACE ( 'NONE', #25644, 3.399999999999999911 ) ;
#16137 = VERTEX_POINT ( 'NONE', #10118 ) ;
#16138 = ORIENTED_EDGE ( 'NONE', *, *, #16340, .T. ) ;
#16139 = CARTESIAN_POINT ( 'NONE',  ( 51.25000000000001421, 1.100000000000534994, 1.001327244211404732 ) ) ;
#16140 = STYLED_ITEM ( 'NONE', ( #21896 ), #14241 ) ;
#16141 = EDGE_CURVE ( 'NONE', #27455, #6127, #3816, .T. ) ;
#16142 = CARTESIAN_POINT ( 'NONE',  ( 51.01608411450972369, -0.7569233679470201981, -1.030722644926826526 ) ) ;
#16144 = DIRECTION ( 'NONE',  ( 1.000000000000000000, 1.047444401652940007E-14, 0.000000000000000000 ) ) ;
#16143 = CARTESIAN_POINT ( 'NONE',  ( -59.94702994616205416, -2.078460969082657872, 3.599999999999778932 ) ) ;
#16145 = VERTEX_POINT ( 'NONE', #6257 ) ;
#16146 = CARTESIAN_POINT ( 'NONE',  ( -58.04792740578360366, 3.330682475591789427, 0.6830477631804109384 ) ) ;
#16147 = DIRECTION ( 'NONE',  ( 0.000000000000000000, 0.000000000000000000, 1.000000000000000000 ) ) ;
#16148 = CARTESIAN_POINT ( 'NONE',  ( 52.98660665890137267, 4.708212704504920687, -1.586977526147875350 ) ) ;
#16149 = CARTESIAN_POINT ( 'NONE',  ( 47.00000000000002842, -3.933368109459640660, 2.186004417993010485 ) ) ;
#16150 = CARTESIAN_POINT ( 'NONE',  ( -54.48779575765000516, 1.517266520141196118, -4.041867453639657271 ) ) ;
#16151 = TOROIDAL_SURFACE ( 'NONE', #2995, 3.525000000000025224, 0.1000000000000000056 ) ;
#16152 = ORIENTED_EDGE ( 'NONE', *, *, #11089, .T. ) ;
#16153 = CARTESIAN_POINT ( 'NONE',  ( 57.03469936322583322, -0.7478111487523275702, 1.780306085601951027 ) ) ;
#16154 = CARTESIAN_POINT ( 'NONE',  ( 61.23787131559241459, 0.8905369330983690102, -1.779178344869518202 ) ) ;
#16155 = CARTESIAN_POINT ( 'NONE',  ( -59.34124040948578482, 3.262940601168114796, 1.250136525132572451 ) ) ;
#16156 = DIRECTION ( 'NONE',  ( -1.000000000000000000, -0.000000000000000000, 3.491481338843133355E-15 ) ) ;
#16157 = COLOUR_RGB ( '', 0.72549020, 0.75294118, 0.79215686) ;
#16158 = CARTESIAN_POINT ( 'NONE',  ( 50.30000000000001847, 1.391941090707534023, -3.850000000000022737 ) ) ;
#16159 = AXIS2_PLACEMENT_3D ( 'NONE', #2805, #15157, #22152 ) ;
#16160 = EDGE_CURVE ( 'NONE', #23063, #2126, #30463, .T. ) ;
#16162 = DIRECTION ( 'NONE',  ( 1.000000000000000000, -0.000000000000000000, 0.000000000000000000 ) ) ;
#16161 = CARTESIAN_POINT ( 'NONE',  ( 31.59287277085072532, 7.495449159458786426, 1.424999999999890132 ) ) ;
#16163 = EDGE_CURVE ( 'NONE', #171, #1692, #19009, .T. ) ;
#16165 = CIRCLE ( 'NONE', #14152, 2.750000000000000444 ) ;
#16164 = CARTESIAN_POINT ( 'NONE',  ( 48.00000000000001421, -4.319730106884872356, -1.256953381662404556 ) ) ;
#16167 = DIRECTION ( 'NONE',  ( 1.000000000000000000, 1.047444401652940007E-14, 0.000000000000000000 ) ) ;
#16166 = CARTESIAN_POINT ( 'NONE',  ( 61.25000000000002132, 6.415596960124259844E-13, 3.111507638930570854E-58 ) ) ;
#16168 = ORIENTED_EDGE ( 'NONE', *, *, #16650, .T. ) ;
#16169 = CYLINDRICAL_SURFACE ( 'NONE', #1268, 2.000000000000000000 ) ;
#16170 = DIRECTION ( 'NONE',  ( 1.000000000000000000, 0.000000000000000000, 0.000000000000000000 ) ) ;
#16172 = CARTESIAN_POINT ( 'NONE',  ( -54.44999999999997442, -1.549999999999999600, -4.029888335921975262 ) ) ;
#16171 = CARTESIAN_POINT ( 'NONE',  ( 58.75000000000000000, 1.922185811755142915, 0.4146205000036791710 ) ) ;
#16173 = CARTESIAN_POINT ( 'NONE',  ( 15.98305126557428935, -5.283830060792393368, 1.151642405604310859 ) ) ;
#16174 = ORIENTED_EDGE ( 'NONE', *, *, #5998, .F. ) ;
#16175 = ORIENTED_EDGE ( 'NONE', *, *, #21915, .F. ) ;
#16176 = CARTESIAN_POINT ( 'NONE',  ( -36.31414349454750834, -4.927920137446197835, 1.660974799722073403 ) ) ;
#16177 = DIRECTION ( 'NONE',  ( -1.000000000000000000, -0.000000000000000000, 3.491481338843133355E-15 ) ) ;
#16178 = EDGE_CURVE ( 'NONE', #21494, #1093, #20692, .T. ) ;
#16179 = VERTEX_POINT ( 'NONE', #2992 ) ;
#16180 = PLANE ( 'NONE',  #7336 ) ;
#16181 = ORIENTED_EDGE ( 'NONE', *, *, #3039, .T. ) ;
#16182 = CARTESIAN_POINT ( 'NONE',  ( 58.65000000000004121, -1.932246131436418768, 0.4087173687851147208 ) ) ;
#16183 = EDGE_LOOP ( 'NONE', ( #5498, #30376, #25427, #13015 ) ) ;
#16184 =( NAMED_UNIT ( * ) SI_UNIT ( $, .STERADIAN. ) SOLID_ANGLE_UNIT ( ) );
#16185 = CARTESIAN_POINT ( 'NONE',  ( -55.07202994616204705, 2.078460969082675192, -3.600000000000186606 ) ) ;
#16186 = TOROIDAL_SURFACE ( 'NONE', #11622, 4.000000000000022204, 0.1000000000000000056 ) ;
#16187 = CARTESIAN_POINT ( 'NONE',  ( -58.33155989232413674, -1.962990915244731571, 3.399999999999784528 ) ) ;
#16188 = ORIENTED_EDGE ( 'NONE', *, *, #26976, .F. ) ;
#16189 = EDGE_LOOP ( 'NONE', ( #7053, #2980, #26453, #6474 ) ) ;
#16190 = EDGE_CURVE ( 'NONE', #18491, #9980, #17478, .T. ) ;
#16191 = PRODUCT ( 'End Cap', 'End Cap', '', ( #22669 ) ) ;
#16192 = ORIENTED_EDGE ( 'NONE', *, *, #21764, .F. ) ;
#16193 = CIRCLE ( 'NONE', #2037, 2.525000000000001243 ) ;
#16194 = CARTESIAN_POINT ( 'NONE',  ( -55.69702994616204705, 4.156921938165313080, -1.827997107644302771E-13 ) ) ;
#16195 = CARTESIAN_POINT ( 'NONE',  ( -55.01905989232411542, 2.107054635024524725E-14, -3.400000000000195310 ) ) ;
#16196 = CARTESIAN_POINT ( 'NONE',  ( 27.56628230087644127, 5.372092466067858396, -1.425000000000095746 ) ) ;
#16197 = CARTESIAN_POINT ( 'NONE',  ( 58.75000000000000711, 1.470078920828144620, -1.470078920826818125 ) ) ;
#16198 = DIRECTION ( 'NONE',  ( 0.000000000000000000, 0.9996898646859344595, 0.02490330187381124133 ) ) ;
#16199 = ADVANCED_FACE ( 'NONE', ( #19936 ), #30592, .T. ) ;
#16201 = CARTESIAN_POINT ( 'NONE',  ( -44.59999999999997300, 8.366749974758367693E-15, -1.870876429524646202E-13 ) ) ;
#16200 = CARTESIAN_POINT ( 'NONE',  ( -57.22499999999997300, 2.964020293532818446E-15, 1.549317489258312010E-18 ) ) ;
#16202 = EDGE_CURVE ( 'NONE', #3831, #23278, #4627, .T. ) ;
#16203 = EDGE_CURVE ( 'NONE', #28519, #7502, #16718, .T. ) ;
#16204 = PLANE ( 'NONE',  #12946 ) ;
#16205 = DIRECTION ( 'NONE',  ( 0.000000000000000000, 0.000000000000000000, -1.000000000000000000 ) ) ;
#16206 = CARTESIAN_POINT ( 'NONE',  ( 15.17214319754858209, 5.086913993735701744, -1.171642046065806131 ) ) ;
#16207 = CARTESIAN_POINT ( 'NONE',  ( 58.72419296898085150, -1.601054456120828640, -0.9760445624807464471 ) ) ;
#16208 = DIRECTION ( 'NONE',  ( 1.000000000000000000, -7.137062321647928144E-17, -7.924918191826694281E-17 ) ) ;
#16209 = DIRECTION ( 'NONE',  ( -1.000000000000000000, -0.000000000000000000, -0.000000000000000000 ) ) ;
#16210 = VERTEX_POINT ( 'NONE', #31270 ) ;
#16212 = CARTESIAN_POINT ( 'NONE',  ( 50.41049980741060921, -0.7811435014051421044, 4.027217152858629134 ) ) ;
#16211 = CARTESIAN_POINT ( 'NONE',  ( 54.11179973533069898, 5.509196088239827205, 2.049999999999811084 ) ) ;
#16213 = B_SPLINE_CURVE_WITH_KNOTS ( 'NONE', 3,
 ( #18240, #15839, #22979, #27877, #1265, #8558, #980, #20458, #13444, #23147, #13605, #8702, #27408, #13000, #18386, #5720, #15370, #25019, #3349, #11725, #4269 ),
 .UNSPECIFIED., .F., .F.,
 ( 4, 2, 2, 1, 2, 2, 2, 1, 1, 2, 2, 4 ),
 ( 0.000000000000000000, 0.4999999998174028959, 0.5312499998059895256, 0.5624999997945763219, 0.6249999997717561318, 0.7499999997261151963, 0.7578124997232579263, 0.7656249997204006563, 0.7812499997146973296, 0.8124999997032911203, 0.8749999996804787017, 0.9999999996348539755 ),
 .UNSPECIFIED. ) ;
#16214 = FACE_OUTER_BOUND ( 'NONE', #30103, .T. ) ;
#16215 = AXIS2_PLACEMENT_3D ( 'NONE', #16936, #7126, #7433 ) ;
#16216 = ORIENTED_EDGE ( 'NONE', *, *, #5826, .F. ) ;
#16217 = CARTESIAN_POINT ( 'NONE',  ( -63.82928932188132620, 6.399178848011186396E-16, 2.550935903222500290E-15 ) ) ;
#16218 = LINE ( 'NONE', #13806, #22909 ) ;
#16219 = CARTESIAN_POINT ( 'NONE',  ( -55.38452994616205416, -3.117691453623976816, 1.799999999999791100 ) ) ;
#16220 = ORIENTED_EDGE ( 'NONE', *, *, #28100, .F. ) ;
#16221 = ORIENTED_EDGE ( 'NONE', *, *, #3523, .F. ) ;
#16222 = CARTESIAN_POINT ( 'NONE',  ( 33.47623932017462778, 2.270506450603774156E-15, 4.375000000000000000 ) ) ;
#16223 = ORIENTED_EDGE ( 'NONE', *, *, #17523, .T. ) ;
#16224 = CARTESIAN_POINT ( 'NONE',  ( 58.74999999999981526, -1.571497941946529142, 1.022750809560129648 ) ) ;
#16225 = CARTESIAN_POINT ( 'NONE',  ( -61.06249999999995737, -0.8699069336946632092, 4.241846523238429256 ) ) ;
#16226 = EDGE_LOOP ( 'NONE', ( #4526, #9589, #674, #9833 ) ) ;
#16227 = DIRECTION ( 'NONE',  ( 1.000000000000000000, -1.219044193948983948E-29, 3.491481338843133355E-15 ) ) ;
#16228 = CARTESIAN_POINT ( 'NONE',  ( 58.66133336607577320, -1.875011749335998124, 0.03256983989574745858 ) ) ;
#16229 = ADVANCED_FACE ( 'NONE', ( #26358 ), #5321, .T. ) ;
#16230 = FACE_OUTER_BOUND ( 'NONE', #402, .T. ) ;
#16231 = VERTEX_POINT ( 'NONE', #4343 ) ;
#16232 = ORIENTED_EDGE ( 'NONE', *, *, #16268, .T. ) ;
#16233 = DIRECTION ( 'NONE',  ( 0.000000000000000000, -0.2008964009354152203, 0.9796124928211138450 ) ) ;
#16234 = EDGE_CURVE ( 'NONE', #26742, #25704, #4662, .T. ) ;
#16235 = CARTESIAN_POINT ( 'NONE',  ( -55.81249999999997868, 3.400000000000007905, -1.865662262041272555E-13 ) ) ;
#16236 = DIRECTION ( 'NONE',  ( -1.000000000000000000, 0.000000000000000000, 3.491481338843133355E-15 ) ) ;
#16237 = AXIS2_PLACEMENT_3D ( 'NONE', #5554, #30234, #30385 ) ;
#16238 = DIRECTION ( 'NONE',  ( -0.000000000000000000, -0.000000000000000000, 1.000000000000000000 ) ) ;
#16239 = FACE_OUTER_BOUND ( 'NONE', #17723, .T. ) ;
#16240 = CIRCLE ( 'NONE', #21824, 1.875000000000001776 ) ;
#16241 = CARTESIAN_POINT ( 'NONE',  ( 47.00000000000002132, 2.428612866367529932E-14, 0.000000000000000000 ) ) ;
#16242 = CARTESIAN_POINT ( 'NONE',  ( 53.85185227134009978, 5.786610019663855020, -1.878038514704438500 ) ) ;
#16244 = CARTESIAN_POINT ( 'NONE',  ( 58.65838214097809100, -0.9083679987361445995, 1.640356269755778751 ) ) ;
#16243 = CARTESIAN_POINT ( 'NONE',  ( 58.66120520762600421, -0.4851925435080639004, -1.811135885493848408 ) ) ;
#16245 = EDGE_CURVE ( 'NONE', #14659, #2157, #28603, .T. ) ;
#16246 = DIRECTION ( 'NONE',  ( 1.000000000000000000, -1.219044193948983948E-29, 3.491481338843133355E-15 ) ) ;
#16247 = CARTESIAN_POINT ( 'NONE',  ( -67.99999999999997158, 0.3264566515200485464, -1.591870300834308471 ) ) ;
#16248 = FACE_OUTER_BOUND ( 'NONE', #1663, .T. ) ;
#16249 = CARTESIAN_POINT ( 'NONE',  ( -54.44999999999997442, 0.000000000000000000, 0.000000000000000000 ) ) ;
#16250 = ORIENTED_EDGE ( 'NONE', *, *, #20575, .T. ) ;
#16251 = ORIENTED_EDGE ( 'NONE', *, *, #30024, .T. ) ;
#16252 = CARTESIAN_POINT ( 'NONE',  ( 51.30406804459317271, -3.900599430603180817, 1.266782962024575410 ) ) ;
#16253 = ORIENTED_EDGE ( 'NONE', *, *, #18427, .F. ) ;
#16254 = CARTESIAN_POINT ( 'NONE',  ( 53.90177594311671072, 7.547472342232321552, 2.049999999999811973 ) ) ;
#16255 = CARTESIAN_POINT ( 'NONE',  ( -58.72085481156723574, 2.489203624310592389, -2.804704140674918911 ) ) ;
#16257 = CARTESIAN_POINT ( 'NONE',  ( -36.68866260399460799, 2.562020839648815773, 4.763023844700911447 ) ) ;
#16256 = DIRECTION ( 'NONE',  ( -1.000000000000000000, 1.219044193948983948E-29, -3.491481338843133355E-15 ) ) ;
#16258 = EDGE_LOOP ( 'NONE', ( #24772, #13964, #12775, #9949 ) ) ;
#16259 = EDGE_LOOP ( 'NONE', ( #1034, #20704, #19742, #10177 ) ) ;
#16260 = CARTESIAN_POINT ( 'NONE',  ( 31.59287277085155665, 7.495449159457250765, -1.425000000000109956 ) ) ;
#16261 = ORIENTED_EDGE ( 'NONE', *, *, #2212, .F. ) ;
#16262 = FACE_OUTER_BOUND ( 'NONE', #19212, .T. ) ;
#16263 = ORIENTED_EDGE ( 'NONE', *, *, #28388, .F. ) ;
#16265 = CARTESIAN_POINT ( 'NONE',  ( -60.44999999999996021, -0.8596938233273121455, 4.192045280110958672 ) ) ;
#16264 = CARTESIAN_POINT ( 'NONE',  ( 52.20711756518984004, -0.4999999999994533817, -1.807104036850122109 ) ) ;
#16266 = ORIENTED_EDGE ( 'NONE', *, *, #18301, .F. ) ;
#16267 = DIRECTION ( 'NONE',  ( 6.938893903907228378E-15, -6.071532165918824830E-15, 1.000000000000000000 ) ) ;
#16268 = EDGE_CURVE ( 'NONE', #4097, #12947, #27070, .T. ) ;
#16269 = CARTESIAN_POINT ( 'NONE',  ( 52.13000000000001677, 0.5000000000005460077, -1.996089927833914146 ) ) ;
#16270 = EDGE_CURVE ( 'NONE', #25398, #7079, #15948, .T. ) ;
#16271 = CARTESIAN_POINT ( 'NONE',  ( -54.49865678108456279, -1.537045020190657807, -3.323865043138457320 ) ) ;
#16272 = CIRCLE ( 'NONE', #24358, 0.05000000000000012768 ) ;
#16273 = CARTESIAN_POINT ( 'NONE',  ( -54.49999999999996447, 2.023778652682504319E-14, -3.400000000000193978 ) ) ;
#16274 = ADVANCED_FACE ( 'NONE', ( #21636 ), #17481, .T. ) ;
#16275 = CARTESIAN_POINT ( 'NONE',  ( -57.07202994616206126, 2.078460969082646770, 3.599999999999804690 ) ) ;
#16276 = CARTESIAN_POINT ( 'NONE',  ( -59.17366934936939060, -2.509710670695419754, -0.9445351920416235059 ) ) ;
#16277 = AXIS2_PLACEMENT_3D ( 'NONE', #26395, #21677, #23873 ) ;
#16278 = CARTESIAN_POINT ( 'NONE',  ( 61.09423418604053069, -0.6373668173463740150, -1.895722432252557432 ) ) ;
#16279 = CYLINDRICAL_SURFACE ( 'NONE', #14025, 0.2500000000000000555 ) ;
#16280 = CARTESIAN_POINT ( 'NONE',  ( -55.67292740578360366, 1.073804522883521573, 3.225979517392336238 ) ) ;
#16282 = EDGE_CURVE ( 'NONE', #15709, #7802, #24155, .T. ) ;
#16281 = B_SPLINE_CURVE_WITH_KNOTS ( 'NONE', 3,
 ( #13960, #23957, #16356, #31242, #4480, #21134, #9392, #11446, #11610, #30922, #13650, #9240, #26002, #14131, #4310, #9568 ),
 .UNSPECIFIED., .F., .F.,
 ( 4, 2, 2, 2, 2, 2, 2, 4 ),
 ( 0.000000000000000000, 0.0004351083927046470894, 0.0008702167854092941789, 0.001740433570818589008, 0.002175541963523235176, 0.002610650356227881344, 0.003045758748932527512, 0.003480867141637172812 ),
 .UNSPECIFIED. ) ;
#16283 =( BOUNDED_CURVE ( )  B_SPLINE_CURVE ( 2, ( #13406, #6476, #4090, #23416, #21219, #30515, #1697, #11365, #18213 ),
 .UNSPECIFIED., .F., .T. ) 
 B_SPLINE_CURVE_WITH_KNOTS ( ( 3, 2, 2, 2, 3 ),
 ( 0.3611111111111111605, 0.3703703703703703498, 0.3888888888888888951, 0.4074074074074073848, 0.4166666666666666852 ),
 .UNSPECIFIED. ) 
 CURVE ( )  GEOMETRIC_REPRESENTATION_ITEM ( )  RATIONAL_B_SPLINE_CURVE ( ( 0.9330127018922194093, 0.9330127018922197424, 1.000000000000000000, 0.8660254037844387076, 1.000000000000000000, 0.8660254037844387076, 1.000000000000000000, 0.9330127018922191873, 0.9330127018922194093 ) ) 
 REPRESENTATION_ITEM ( '' )  );
#16284 = CARTESIAN_POINT ( 'NONE',  ( 64.95000000000001705, 1.401298464324817071E-42, -6.803151388735846952E-13 ) ) ;
#16285 = ORIENTED_EDGE ( 'NONE', *, *, #7232, .F. ) ;
#16286 = FACE_OUTER_BOUND ( 'NONE', #1640, .T. ) ;
#16287 = CARTESIAN_POINT ( 'NONE',  ( -59.48573950359912743, 3.423031164920794289, -1.114835254188495162 ) ) ;
#16288 = CARTESIAN_POINT ( 'NONE',  ( -36.68866260399460799, -0.7269167730137759964, 5.359285300587722567 ) ) ;
#16289 = DIRECTION ( 'NONE',  ( 0.000000000000000000, -1.000000000000000000, 0.000000000000000000 ) ) ;
#16290 = ORIENTED_EDGE ( 'NONE', *, *, #16750, .F. ) ;
#16291 = CARTESIAN_POINT ( 'NONE',  ( 58.65838214097829706, 1.640356269756469310, 0.9083679987366242159 ) ) ;
#16292 = EDGE_LOOP ( 'NONE', ( #7659, #5004, #28262, #8614, #9687 ) ) ;
#16293 = SURFACE_SIDE_STYLE ('',( #9321 ) ) ;
#16294 = AXIS2_PLACEMENT_3D ( 'NONE', #9629, #28922, #7235 ) ;
#16296 = CARTESIAN_POINT ( 'NONE',  ( 58.50000000000001421, 0.000000000000000000, 0.000000000000000000 ) ) ;
#16295 = CARTESIAN_POINT ( 'NONE',  ( 48.39103590182073589, 1.199904535326282495, 3.921111011342365504 ) ) ;
#16297 = ORIENTED_EDGE ( 'NONE', *, *, #30915, .T. ) ;
#16298 = EDGE_LOOP ( 'NONE', ( #6757, #11358, #17834, #19421 ) ) ;
#16299 = DIRECTION ( 'NONE',  ( -1.000000000000000000, -0.000000000000000000, -0.000000000000000000 ) ) ;
#16300 = DIRECTION ( 'NONE',  ( 0.000000000000000000, -0.9996898646859344595, -0.02490330187381124480 ) ) ;
#16302 = CARTESIAN_POINT ( 'NONE',  ( 51.80000000000001137, -3.933368109459640660, -2.186004417993355542 ) ) ;
#16301 = CARTESIAN_POINT ( 'NONE',  ( 51.60138551324653378, -4.191665075176590705, -1.623492990431073979 ) ) ;
#16303 = ORIENTED_EDGE ( 'NONE', *, *, #25693, .F. ) ;
#16304 = CARTESIAN_POINT ( 'NONE',  ( -59.73542740578360366, 0.7887156198831659637, -3.845940847736173840 ) ) ;
#16305 = CARTESIAN_POINT ( 'NONE',  ( -36.72207054450174013, 3.705258523861193254, 3.939862169952904836 ) ) ;
#16306 = CONTEXT_DEPENDENT_SHAPE_REPRESENTATION ( #28609, #22734 ) ;
#16307 = ADVANCED_FACE ( 'NONE', ( #21164 ), #16554, .T. ) ;
#16308 = SPHERICAL_SURFACE ( 'NONE', #2290, 0.1000000000000000056 ) ;
#16309 = DIRECTION ( 'NONE',  ( 0.000000000000000000, 0.2008964009354147484, -0.9796124928211139560 ) ) ;
#16310 = AXIS2_PLACEMENT_3D ( 'NONE', #4051, #23374, #1655 ) ;
#16311 = EDGE_LOOP ( 'NONE', ( #8973, #4967, #25399, #3408 ) ) ;
#16312 = CARTESIAN_POINT ( 'NONE',  ( -77.29999999999998295, -0.4398635404618146394, -0.01095745282447164320 ) ) ;
#16313 = CARTESIAN_POINT ( 'NONE',  ( -36.04518387042614336, 2.525801254962709130, -4.794550361020548657 ) ) ;
#16314 = CARTESIAN_POINT ( 'NONE',  ( 58.66107449606957402, -1.606832818401185747, -0.9668599424570839540 ) ) ;
#16315 = DIRECTION ( 'NONE',  ( 1.015447888376667464E-14, 0.000000000000000000, 1.000000000000000000 ) ) ;
#16316 = CARTESIAN_POINT ( 'NONE',  ( 57.00303004862897183, -0.7171412854886025645, -2.441992855427530085 ) ) ;
#16317 = EDGE_CURVE ( 'NONE', #28072, #2901, #13397, .T. ) ;
#16319 = CARTESIAN_POINT ( 'NONE',  ( 58.74999981196286569, -1.865248186429863564, -0.5877861523402161392 ) ) ;
#16318 = CARTESIAN_POINT ( 'NONE',  ( 68.95000000000003126, 1.401298464324817071E-42, -7.222129149397022450E-13 ) ) ;
#16321 = DIRECTION ( 'NONE',  ( -1.000000000000000000, -0.000000000000000000, 3.491481338843133355E-15 ) ) ;
#16320 = DIRECTION ( 'NONE',  ( 0.000000000000000000, 0.000000000000000000, -1.000000000000000000 ) ) ;
#16322 = VERTEX_POINT ( 'NONE', #23507 ) ;
#16323 = CARTESIAN_POINT ( 'NONE',  ( 61.25000000000004263, -0.8718791990806975534, -1.626461527140063756 ) ) ;
#16324 = LINE ( 'NONE', #1585, #19903 ) ;
#16325 = AXIS2_PLACEMENT_3D ( 'NONE', #6241, #28247, #6557 ) ;
#16327 = CARTESIAN_POINT ( 'NONE',  ( -36.22955757456059445, 5.027944117023995574, 1.353132643598440987 ) ) ;
#16326 = CARTESIAN_POINT ( 'NONE',  ( -54.49999999999997868, -4.276948333784439171, 0.9210526315789471230 ) ) ;
#16328 = DIRECTION ( 'NONE',  ( 1.000000000000000000, 1.018631342913014973E-14, 0.000000000000000000 ) ) ;
#16329 = ORIENTED_EDGE ( 'NONE', *, *, #23521, .T. ) ;
#16330 = EDGE_CURVE ( 'NONE', #21195, #24526, #4842, .T. ) ;
#16331 = ORIENTED_EDGE ( 'NONE', *, *, #10667, .T. ) ;
#16332 = CARTESIAN_POINT ( 'NONE',  ( -36.39645873810206211, -4.962973169597136192, 2.162832296644333852 ) ) ;
#16333 = DIRECTION ( 'NONE',  ( 1.000000000000000000, 1.047444401652940007E-14, 0.000000000000000000 ) ) ;
#16334 = EDGE_LOOP ( 'NONE', ( #20179, #4012, #11576, #29559 ) ) ;
#16335 = DIRECTION ( 'NONE',  ( 1.000000000000000000, 1.047444401652940007E-14, 0.000000000000000000 ) ) ;
#16336 = EDGE_LOOP ( 'NONE', ( #17046, #6446, #9013, #11328 ) ) ;
#16337 = CARTESIAN_POINT ( 'NONE',  ( 58.64999999999999147, 1.872332544501737139, 0.09997921184905474157 ) ) ;
#16338 = ORIENTED_EDGE ( 'NONE', *, *, #11524, .T. ) ;
#16339 =( LENGTH_UNIT ( ) NAMED_UNIT ( * ) SI_UNIT ( .MILLI., .METRE. ) );
#16340 = EDGE_CURVE ( 'NONE', #11624, #16493, #18502, .T. ) ;
#16341 = CARTESIAN_POINT ( 'NONE',  ( -56.51905989232411542, 2.023778652682506843E-14, -3.400000000000200640 ) ) ;
#16342 = ORIENTED_EDGE ( 'NONE', *, *, #24969, .F. ) ;
#16343 = VERTEX_POINT ( 'NONE', #2456 ) ;
#16344 = ORIENTED_EDGE ( 'NONE', *, *, #17072, .F. ) ;
#16345 = CARTESIAN_POINT ( 'NONE',  ( -55.44702994616206126, -2.078460969082657872, 3.599999999999794920 ) ) ;
#16346 = CARTESIAN_POINT ( 'NONE',  ( 30.78427835929706902, 7.077770142316450297, -1.425000000000106626 ) ) ;
#16347 = CIRCLE ( 'NONE', #23947, 0.1500000000000001887 ) ;
#16348 = DIRECTION ( 'NONE',  ( 0.000000000000000000, 1.224646799147353947E-16, 1.000000000000000000 ) ) ;
#16349 = AXIS2_PLACEMENT_3D ( 'NONE', #11766, #16209, #18593 ) ;
#16350 = CARTESIAN_POINT ( 'NONE',  ( -61.40479058095097287, -2.566399095993047830, -0.8388061039871230751 ) ) ;
#16351 = ADVANCED_FACE ( 'NONE', ( #12112 ), #14932, .T. ) ;
#16353 = CARTESIAN_POINT ( 'NONE',  ( -58.02900635094607651, -1.737685414808523232, 3.471684241605558885 ) ) ;
#16352 = CARTESIAN_POINT ( 'NONE',  ( 69.20000000000001705, -0.7500000000000000000, -2.238246715074081017 ) ) ;
#16354 =( NAMED_UNIT ( * ) PLANE_ANGLE_UNIT ( ) SI_UNIT ( $, .RADIAN. ) );
#16355 = CARTESIAN_POINT ( 'NONE',  ( 58.50000000000001421, 0.8000000000000000444, 2.421260002560649660 ) ) ;
#16356 = CARTESIAN_POINT ( 'NONE',  ( -36.14490256869206775, -2.228039998204413230, -4.927410888447854020 ) ) ;
#16357 = CARTESIAN_POINT ( 'NONE',  ( 56.95000000000001705, 0.7137254901960785602, 2.500119182087999548 ) ) ;
#16358 = CARTESIAN_POINT ( 'NONE',  ( 57.00000000000001421, 0.7137254901960804476, -2.500119182088006209 ) ) ;
#16359 = DIRECTION ( 'NONE',  ( -5.046468293750706671E-15, 0.000000000000000000, -1.000000000000000000 ) ) ;
#16360 = ORIENTED_EDGE ( 'NONE', *, *, #29057, .F. ) ;
#16362 = DIRECTION ( 'NONE',  ( 0.000000000000000000, -1.000000000000000000, 0.000000000000000000 ) ) ;
#16361 = CARTESIAN_POINT ( 'NONE',  ( -69.22071067811863543, -6.995007661688606141E-16, 2.451642053546763754E-15 ) ) ;
#16363 = EDGE_CURVE ( 'NONE', #28473, #28315, #25058, .T. ) ;
#16364 = CARTESIAN_POINT ( 'NONE',  ( 58.75000000000002132, 6.153735859711025284E-13, 3.111507638930570854E-58 ) ) ;
#16365 = ORIENTED_EDGE ( 'NONE', *, *, #8715, .F. ) ;
#16366 = FILL_AREA_STYLE ('',( #4017 ) ) ;
#16367 = TOROIDAL_SURFACE ( 'NONE', #14349, 0.3000000000000000444, 0.05000000000000000278 ) ;
#16368 = CARTESIAN_POINT ( 'NONE',  ( 63.50000000000002842, 1.401298464324817071E-42, -6.651271950496169736E-13 ) ) ;
#16369 = CARTESIAN_POINT ( 'NONE',  ( -60.18749999999998579, 1.962990915244722689, 3.399999999999794742 ) ) ;
#16370 = EDGE_LOOP ( 'NONE', ( #21579, #30825 ) ) ;
#16371 = ORIENTED_EDGE ( 'NONE', *, *, #4359, .F. ) ;
#16372 = CARTESIAN_POINT ( 'NONE',  ( 15.39414421509791175, 4.855742670514265669, 1.883114206442366489 ) ) ;
#16373 = ORIENTED_EDGE ( 'NONE', *, *, #5356, .F. ) ;
#16374 = CARTESIAN_POINT ( 'NONE',  ( 58.72427158855736451, -1.600821037878293884, 0.9764256747731572261 ) ) ;
#16375 = ADVANCED_FACE ( 'NONE', ( #5131 ), #19860, .F. ) ;
#16376 = CARTESIAN_POINT ( 'NONE',  ( 54.12540754135502397, 6.691802926424378128, -2.050000000000183675 ) ) ;
#16377 = ORIENTED_EDGE ( 'NONE', *, *, #15436, .T. ) ;
#16378 = CARTESIAN_POINT ( 'NONE',  ( -59.69999999999997442, -3.399999999999991473, -2.235080921937235780E-13 ) ) ;
#16379 = CYLINDRICAL_SURFACE ( 'NONE', #27836, 2.525000000000001243 ) ;
#16380 = ADVANCED_FACE ( 'NONE', ( #2915 ), #223, .F. ) ;
#16381 = DIRECTION ( 'NONE',  ( 0.000000000000000000, 0.9996898646859344595, 0.02490330187381124133 ) ) ;
#16382 = ORIENTED_EDGE ( 'NONE', *, *, #24625, .F. ) ;
#16383 = ORIENTED_EDGE ( 'NONE', *, *, #27891, .T. ) ;
#16384 = CARTESIAN_POINT ( 'NONE',  ( 47.00000000000002132, 1.426739617975221641, -3.843750000000023093 ) ) ;
#16385 = CARTESIAN_POINT ( 'NONE',  ( -62.09999999999997300, -2.718470093012312905, 0.1920549639088918459 ) ) ;
#16386 = CARTESIAN_POINT ( 'NONE',  ( 56.98109951608436319, -0.7885528131279547770, -2.477553856021609491 ) ) ;
#16387 = ORIENTED_EDGE ( 'NONE', *, *, #16178, .T. ) ;
#16388 = DIRECTION ( 'NONE',  ( 0.5633368246415177971, -0.8262273428075421755, 0.000000000000000000 ) ) ;
#16389 = DIRECTION ( 'NONE',  ( 0.000000000000000000, 0.000000000000000000, 1.000000000000000000 ) ) ;
#16390 = EDGE_CURVE ( 'NONE', #7615, #15970, #12912, .T. ) ;
#16391 = DIRECTION ( 'NONE',  ( 2.114027855662425118E-44, -1.000000000000000000, -3.491481338843139666E-15 ) ) ;
#16392 = CARTESIAN_POINT ( 'NONE',  ( 57.03052440771394060, 0.7462437932013319397, -1.781707539322121336 ) ) ;
#16394 = CARTESIAN_POINT ( 'NONE',  ( 58.75000000000002842, -0.8979909453704965072, 1.749377236608653297 ) ) ;
#16393 =( NAMED_UNIT ( * ) SI_UNIT ( $, .STERADIAN. ) SOLID_ANGLE_UNIT ( ) );
#16395 = DIRECTION ( 'NONE',  ( 1.000000000000000000, 3.054025858079668409E-16, -2.042474015755241579E-16 ) ) ;
#16396 = CARTESIAN_POINT ( 'NONE',  ( 51.80000000000001847, -3.726179070414207928, -1.000000000000002220 ) ) ;
#16397 = CARTESIAN_POINT ( 'NONE',  ( 51.80000000000001847, 2.428612866367529932E-14, 0.000000000000000000 ) ) ;
#16398 = ORIENTED_EDGE ( 'NONE', *, *, #15600, .F. ) ;
#16399 = EDGE_CURVE ( 'NONE', #13704, #6992, #20019, .T. ) ;
#16400 = VECTOR ( 'NONE', #14208, 1000.000000000000000 ) ;
#16401 = CARTESIAN_POINT ( 'NONE',  ( 51.14630318392405428, 0.9364487020640391846, 1.503522130792586342 ) ) ;
#16402 = ORIENTED_EDGE ( 'NONE', *, *, #22563, .F. ) ;
#16403 = ADVANCED_FACE ( 'NONE', ( #7662 ), #7592, .T. ) ;
#16404 = CARTESIAN_POINT ( 'NONE',  ( 53.71283936284426375, 7.813984279442741432, 2.049999999999812417 ) ) ;
#16405 = CARTESIAN_POINT ( 'NONE',  ( -58.15835481156722864, -3.238593381231841928, -2.874284765127022023 ) ) ;
#16406 = CARTESIAN_POINT ( 'NONE',  ( 58.75000000000002132, 6.153735859711025284E-13, 3.111507638930570854E-58 ) ) ;
#16407 = ORIENTED_EDGE ( 'NONE', *, *, #771, .T. ) ;
#16408 = CARTESIAN_POINT ( 'NONE',  ( 60.75000000000001421, 0.6500000000006362910, -1.489337100860648189 ) ) ;
#16409 = ORIENTED_EDGE ( 'NONE', *, *, #25886, .F. ) ;
#16410 = DIRECTION ( 'NONE',  ( 0.000000000000000000, 0.9996898646859343485, 0.02490330187381116153 ) ) ;
#16411 = EDGE_LOOP ( 'NONE', ( #14340, #3859, #10170, #4463, #19812, #29299, #10398, #1181, #2895, #7013 ) ) ;
#16413 = DIRECTION ( 'NONE',  ( 0.000000000000000000, -0.9996898646859344595, -0.02490330187381124480 ) ) ;
#16412 = DIRECTION ( 'NONE',  ( 0.000000000000000000, 0.000000000000000000, 1.000000000000000000 ) ) ;
#16414 = EDGE_CURVE ( 'NONE', #556, #13873, #6352, .T. ) ;
#16415 = ORIENTED_EDGE ( 'NONE', *, *, #28770, .F. ) ;
#16416 = AXIS2_PLACEMENT_3D ( 'NONE', #12137, #31127, #14660 ) ;
#16417 = CARTESIAN_POINT ( 'NONE',  ( 53.38804190906846259, 7.887047813379708394, 1.884060075242533161 ) ) ;
#16418 = EDGE_CURVE ( 'NONE', #7185, #16500, #10844, .T. ) ;
#16419 = CARTESIAN_POINT ( 'NONE',  ( 58.64999999999999147, 1.834410884276644449, -0.3880228184651526857 ) ) ;
#16420 = CARTESIAN_POINT ( 'NONE',  ( 47.87910813548244704, -4.387164041431067751, 1.383037119376591351 ) ) ;
#16421 = CARTESIAN_POINT ( 'NONE',  ( 57.01079215475500206, 0.7500001437588036390, -1.746008375800299772 ) ) ;
#16422 = CARTESIAN_POINT ( 'NONE',  ( -57.69702994616206126, -2.078460969082657872, 3.599999999999786926 ) ) ;
#16423 = CARTESIAN_POINT ( 'NONE',  ( 61.25000000000000711, 1.323060376182058961, -1.499837071477343242 ) ) ;
#16424 = CARTESIAN_POINT ( 'NONE',  ( 52.20711756518984004, -0.4999999999994533817, -1.996089927833914146 ) ) ;
#16425 =( BOUNDED_CURVE ( )  B_SPLINE_CURVE ( 2, ( #6109, #25409, #13355, #28893, #26357, #21320, #31097, #30950, #26680 ),
 .UNSPECIFIED., .F., .T. ) 
 B_SPLINE_CURVE_WITH_KNOTS ( ( 3, 2, 2, 2, 3 ),
 ( 0.5833333333333333703, 0.5925925925925925597, 0.6111111111111111605, 0.6296296296296296502, 0.6388888888888889506 ),
 .UNSPECIFIED. ) 
 CURVE ( )  GEOMETRIC_REPRESENTATION_ITEM ( )  RATIONAL_B_SPLINE_CURVE ( ( 0.9330127018922194093, 0.9330127018922197424, 1.000000000000000000, 0.8660254037844387076, 1.000000000000000000, 0.8660254037844387076, 1.000000000000000000, 0.9330127018922189652, 0.9330127018922194093 ) ) 
 REPRESENTATION_ITEM ( '' )  );
#16426 = CARTESIAN_POINT ( 'NONE',  ( -54.49999999999997868, 1.549999999999999600, 3.332135201338624952 ) ) ;
#16427 = AXIS2_PLACEMENT_3D ( 'NONE', #2757, #20022, #12717 ) ;
#16428 = CARTESIAN_POINT ( 'NONE',  ( -56.61042740578359656, 3.725040285533373741, -1.239922660687670986 ) ) ;
#16429 = DIRECTION ( 'NONE',  ( 1.189524669241239105E-14, 0.000000000000000000, 1.000000000000000000 ) ) ;
#16430 = AXIS2_PLACEMENT_3D ( 'NONE', #8920, #6561, #25870 ) ;
#16431 = EDGE_LOOP ( 'NONE', ( #19872, #12533, #15386, #7866 ) ) ;
#16432 = EDGE_CURVE ( 'NONE', #2467, #16145, #24058, .T. ) ;
#16433 = CARTESIAN_POINT ( 'NONE',  ( -54.39999999999999147, -1.557046979865776226, 3.273565289174688253 ) ) ;
#16434 = CARTESIAN_POINT ( 'NONE',  ( -36.58361892165972762, 0.1071614981651403398, 5.407381887150175537 ) ) ;
#16435 = CARTESIAN_POINT ( 'NONE',  ( 58.75000000000002132, 6.153735859711025284E-13, 3.111507638930570854E-58 ) ) ;
#16436 = ADVANCED_FACE ( 'NONE', ( #22589 ), #21766, .T. ) ;
#16437 = EDGE_LOOP ( 'NONE', ( #24481, #30030 ) ) ;
#16438 = CARTESIAN_POINT ( 'NONE',  ( -54.49999999999999289, -1.500000000000006661, 3.959797974644449603 ) ) ;
#16439 = VERTEX_POINT ( 'NONE', #8627 ) ;
#16440 = ADVANCED_FACE ( 'NONE', ( #3258 ), #25260, .F. ) ;
#16441 = CARTESIAN_POINT ( 'NONE',  ( 51.59739104186226655, 1.165722629542050415, 1.468576096419531352 ) ) ;
#16443 = DIRECTION ( 'NONE',  ( -1.000000000000000000, -0.000000000000000000, -0.000000000000000000 ) ) ;
#16442 = CARTESIAN_POINT ( 'NONE',  ( 51.80000000000001137, 6.475000000000062705, -2.050000000000180123 ) ) ;
#16444 = EDGE_LOOP ( 'NONE', ( #25113, #25468, #19062, #6872, #8759, #22993, #20285, #10883 ) ) ;
#16445 = VERTEX_POINT ( 'NONE', #1046 ) ;
#16446 = CARTESIAN_POINT ( 'NONE',  ( -59.33448904220814057, -2.516908228110002366, -1.027510759589413736 ) ) ;
#16447 = CARTESIAN_POINT ( 'NONE',  ( 41.48619405471883681, -151.3359592902621955, -2.050000000000163691 ) ) ;
#16449 = DIRECTION ( 'NONE',  ( -1.000000000000000000, -3.053848253006669023E-16, 2.042510438544995415E-16 ) ) ;
#16448 = CARTESIAN_POINT ( 'NONE',  ( 34.50000000000001421, 3.918869757271530460E-16, 3.200000000000000178 ) ) ;
#16450 = ORIENTED_EDGE ( 'NONE', *, *, #7232, .T. ) ;
#16451 = CARTESIAN_POINT ( 'NONE',  ( -56.81249999999997868, 4.108500314926513575, -1.367561758111407455 ) ) ;
#16452 = LINE ( 'NONE', #26109, #25656 ) ;
#16453 = CIRCLE ( 'NONE', #2789, 3.286176633967618166 ) ;
#16454 = CARTESIAN_POINT ( 'NONE',  ( -55.33155989232414385, -1.962990915244735790, 3.399999999999792522 ) ) ;
#16455 = CARTESIAN_POINT ( 'NONE',  ( 64.00000000000001421, 1.163569835200988601E-28, -2.234548056859606357E-13 ) ) ;
#16456 = DIRECTION ( 'NONE',  ( 0.000000000000000000, -0.2008964009354147484, 0.9796124928211139560 ) ) ;
#16457 = CARTESIAN_POINT ( 'NONE',  ( -54.45981523601835761, 1.500740478982482973, -4.030402907299741599 ) ) ;
#16458 = ORIENTED_EDGE ( 'NONE', *, *, #23887, .F. ) ;
#16459 = CIRCLE ( 'NONE', #2797, 4.000000000000000000 ) ;
#16460 = CARTESIAN_POINT ( 'NONE',  ( 58.65000000000001990, 6.143261415694495821E-13, 3.111507638930570854E-58 ) ) ;
#16461 =( BOUNDED_CURVE ( )  B_SPLINE_CURVE ( 3, ( #15298, #24944, #25745, #13694 ),
 .UNSPECIFIED., .F., .T. ) 
 B_SPLINE_CURVE_WITH_KNOTS ( ( 4, 4 ),
 ( 1.570796326794897890, 3.141592653589794448 ),
 .UNSPECIFIED. ) 
 CURVE ( )  GEOMETRIC_REPRESENTATION_ITEM ( )  RATIONAL_B_SPLINE_CURVE ( ( 1.000000000000000000, 0.8047378541243649375, 0.8047378541243649375, 1.000000000000000000 ) ) 
 REPRESENTATION_ITEM ( '' )  );
#16462 = CIRCLE ( 'NONE', #25034, 0.1499999999999999667 ) ;
#16463 = CARTESIAN_POINT ( 'NONE',  ( -36.22909104983231998, 3.722832355337073018, -3.938244298534259169 ) ) ;
#16464 = DIRECTION ( 'NONE',  ( 1.000000000000000000, 2.586136946169074517E-16, -0.000000000000000000 ) ) ;
#16465 = PLANE ( 'NONE',  #13920 ) ;
#16466 = DIRECTION ( 'NONE',  ( 1.000000000000000000, -1.219044193948983948E-29, 3.491481338843133355E-15 ) ) ;
#16468 = CARTESIAN_POINT ( 'NONE',  ( 50.30000000000001847, 1.409787217987196861, 3.850000000000022737 ) ) ;
#16467 = CARTESIAN_POINT ( 'NONE',  ( 51.45655683570191741, -0.9591657938390835136, 1.468576096419531574 ) ) ;
#16469 = B_SPLINE_CURVE_WITH_KNOTS ( 'NONE', 3,
 ( #31263, #6568, #21316, #16228, #25877, #1974 ),
 .UNSPECIFIED., .F., .F.,
 ( 4, 2, 4 ),
 ( 0.000000000000000000, 0.0001000270069600267081, 0.0002000540139200534162 ),
 .UNSPECIFIED. ) ;
#16470 = AXIS2_PLACEMENT_3D ( 'NONE', #1690, #6769, #4398 ) ;
#16471 = CARTESIAN_POINT ( 'NONE',  ( 47.11804492410362144, -4.249103233463815243, -1.767380283559819576 ) ) ;
#16473 = CARTESIAN_POINT ( 'NONE',  ( 61.00000000000001421, 0.8666666666673054076, -1.374595900215364930 ) ) ;
#16472 = DIRECTION ( 'NONE',  ( 0.000000000000000000, -1.000000000000000000, 0.000000000000000000 ) ) ;
#16474 = EDGE_CURVE ( 'NONE', #24391, #29070, #792, .T. ) ;
#16475 = AXIS2_PLACEMENT_3D ( 'NONE', #24372, #12042, #14853 ) ;
#16476 = ORIENTED_EDGE ( 'NONE', *, *, #62, .T. ) ;
#16477 = CARTESIAN_POINT ( 'NONE',  ( -62.05403641351750821, -2.672098272234639804, -0.3800858690569366982 ) ) ;
#16478 = EDGE_CURVE ( 'NONE', #26980, #709, #11010, .T. ) ;
#16479 = DIRECTION ( 'NONE',  ( 1.000000000000000000, 3.053848253006669023E-16, -2.042510438544995415E-16 ) ) ;
#16481 = CARTESIAN_POINT ( 'NONE',  ( -36.39645873810229659, 5.286410563980371791, 1.167394352644176569 ) ) ;
#16480 = CARTESIAN_POINT ( 'NONE',  ( -73.89999999999997726, 1.259609229504275341, 0.03137816036100692790 ) ) ;
#16482 = FACE_OUTER_BOUND ( 'NONE', #28920, .T. ) ;
#16483 = AXIS2_PLACEMENT_3D ( 'NONE', #2996, #2686, #24518 ) ;
#16484 = ORIENTED_EDGE ( 'NONE', *, *, #2856, .T. ) ;
#16485 = ORIENTED_EDGE ( 'NONE', *, *, #1139, .T. ) ;
#16486 = CARTESIAN_POINT ( 'NONE',  ( -36.63359589171323449, -4.847650360853545948, 2.396424556482879442 ) ) ;
#16487 = DIRECTION ( 'NONE',  ( 1.000000000000000000, 1.786976680021873984E-16, 2.459562394685737870E-16 ) ) ;
#16488 = CIRCLE ( 'NONE', #23066, 0.1000000000000002554 ) ;
#16489 = VERTEX_POINT ( 'NONE', #9430 ) ;
#16490 = AXIS2_PLACEMENT_3D ( 'NONE', #23816, #60, #2436 ) ;
#16491 = CARTESIAN_POINT ( 'NONE',  ( -56.52900635094607651, -1.737685414808518347, 3.471684241605561994 ) ) ;
#16492 = B_SPLINE_CURVE_WITH_KNOTS ( 'NONE', 3,
 ( #19428, #21819, #9764, #21351, #2316, #7383 ),
 .UNSPECIFIED., .F., .F.,
 ( 4, 2, 4 ),
 ( 0.000000000000000000, 0.0001000270069598671678, 0.0002000540139197343355 ),
 .UNSPECIFIED. ) ;
#16493 = VERTEX_POINT ( 'NONE', #26207 ) ;
#16494 = CARTESIAN_POINT ( 'NONE',  ( -56.67499999999996874, 3.131991715727200307E-15, -1.107867533772800737E-16 ) ) ;
#16495 = ORIENTED_EDGE ( 'NONE', *, *, #24105, .F. ) ;
#16496 =( NAMED_UNIT ( * ) PLANE_ANGLE_UNIT ( ) SI_UNIT ( $, .RADIAN. ) );
#16497 = EDGE_CURVE ( 'NONE', #8913, #25822, #23540, .T. ) ;
#16498 = AXIS2_PLACEMENT_3D ( 'NONE', #9113, #13534, #23513 ) ;
#16499 = DIRECTION ( 'NONE',  ( 0.000000000000000000, -1.000000000000000000, -4.336808689942015369E-15 ) ) ;
#16500 = VERTEX_POINT ( 'NONE', #7059 ) ;
#16501 =( LENGTH_UNIT ( ) NAMED_UNIT ( * ) SI_UNIT ( .MILLI., .METRE. ) );
#16502 = ORIENTED_EDGE ( 'NONE', *, *, #4399, .F. ) ;
#16503 = CIRCLE ( 'NONE', #1818, 0.1500000000000001887 ) ;
#16504 = ORIENTED_EDGE ( 'NONE', *, *, #21109, .F. ) ;
#16505 = CARTESIAN_POINT ( 'NONE',  ( -60.24999999999997158, 2.944486372867092250, 1.699999999999797673 ) ) ;
#16506 = CARTESIAN_POINT ( 'NONE',  ( 56.98981708175836758, -0.7951539052630037796, 2.475425269917271187 ) ) ;
#16507 = DIRECTION ( 'NONE',  ( -1.000000000000000000, 0.000000000000000000, -0.000000000000000000 ) ) ;
#16508 = DIRECTION ( 'NONE',  ( 1.000000000000000000, 1.047444401652940007E-14, -0.000000000000000000 ) ) ;
#16509 = AXIS2_PLACEMENT_3D ( 'NONE', #26974, #5761, #7669 ) ;
#16510 = DIRECTION ( 'NONE',  ( 1.163827112947710658E-15, 0.9428090415820645775, -0.3333333333333299286 ) ) ;
#16511 = AXIS2_PLACEMENT_3D ( 'NONE', #6617, #21036, #23404 ) ;
#16512 = VECTOR ( 'NONE', #5882, 999.9999999999998863 ) ;
#16513 = AXIS2_PLACEMENT_3D ( 'NONE', #29631, #22068, #12691 ) ;
#16515 = CARTESIAN_POINT ( 'NONE',  ( 51.70000000000000995, 4.174380580618773706, -1.932497546739578631 ) ) ;
#16514 = CARTESIAN_POINT ( 'NONE',  ( -36.81959771849335539, 5.295593823078808882, -1.114646847977579069 ) ) ;
#16516 = DIRECTION ( 'NONE',  ( 3.384826294588897856E-15, 0.000000000000000000, 1.000000000000000000 ) ) ;
#16517 = CARTESIAN_POINT ( 'NONE',  ( -37.18272003341174781, -1.653865106024005792E-14, 0.000000000000000000 ) ) ;
#16518 = DIRECTION ( 'NONE',  ( 0.000000000000000000, -1.000000000000000000, 0.000000000000000000 ) ) ;
#16519 = EDGE_CURVE ( 'NONE', #28370, #4182, #13904, .T. ) ;
#16520 = ORIENTED_EDGE ( 'NONE', *, *, #15834, .T. ) ;
#16521 = LINE ( 'NONE', #23191, #6341 ) ;
#16522 = VECTOR ( 'NONE', #9906, 1000.000000000000114 ) ;
#16523 = CARTESIAN_POINT ( 'NONE',  ( 53.74845224966695412, 7.732683774216504879, 2.049999999999811973 ) ) ;
#16524 = ORIENTED_EDGE ( 'NONE', *, *, #22731, .F. ) ;
#16526 = DIRECTION ( 'NONE',  ( 1.000000000000000000, 1.047444401652940007E-14, 0.000000000000000000 ) ) ;
#16525 = CARTESIAN_POINT ( 'NONE',  ( 48.39081772275599747, -1.198378070452209121, 3.921585382223973681 ) ) ;
#16527 = CARTESIAN_POINT ( 'NONE',  ( 54.36194317780777396, 6.362460706117157194, -2.050000000000189004 ) ) ;
#16528 = CIRCLE ( 'NONE', #27637, 1.875000000000001776 ) ;
#16529 = CARTESIAN_POINT ( 'NONE',  ( -71.49999999999998579, 0.4118376219175989839, -2.008205610283281040 ) ) ;
#16530 = AXIS2_PLACEMENT_3D ( 'NONE', #13764, #1274, #25819 ) ;
#16531 = AXIS2_PLACEMENT_3D ( 'NONE', #3653, #10481, #8101 ) ;
#16532 = ORIENTED_EDGE ( 'NONE', *, *, #26426, .T. ) ;
#16533 = CARTESIAN_POINT ( 'NONE',  ( 22.72662675107780927, 7.272876594663812533, -1.425000000000078870 ) ) ;
#16534 = CARTESIAN_POINT ( 'NONE',  ( 30.08242191457677706, 7.215531071606934965, 1.424999999999895239 ) ) ;
#16535 = CARTESIAN_POINT ( 'NONE',  ( -59.68749999999995737, 1.962990915244749557, -3.400000000000203304 ) ) ;
#16536 = ORIENTED_EDGE ( 'NONE', *, *, #23367, .T. ) ;
#16537 = AXIS2_PLACEMENT_3D ( 'NONE', #2580, #12228, #16516 ) ;
#16538 = ORIENTED_EDGE ( 'NONE', *, *, #12565, .T. ) ;
#16539 = CARTESIAN_POINT ( 'NONE',  ( 51.80000000000000426, 2.478823385132571090E-14, -4.100000000000173728 ) ) ;
#16540 = EDGE_LOOP ( 'NONE', ( #25660, #4364, #6364, #2630 ) ) ;
#16541 = AXIS2_PLACEMENT_3D ( 'NONE', #16795, #22323, #9674 ) ;
#16542 = CYLINDRICAL_SURFACE ( 'NONE', #29817, 0.1500000000000001887 ) ;
#16543 = EDGE_CURVE ( 'NONE', #6673, #20943, #6727, .T. ) ;
#16544 = CARTESIAN_POINT ( 'NONE',  ( -57.69702994616206126, -2.078460969082657872, 3.599999999999786926 ) ) ;
#16545 = VERTEX_POINT ( 'NONE', #31103 ) ;
#16546 = CARTESIAN_POINT ( 'NONE',  ( -62.14999999999998437, -2.749147127886318653, -0.06848408015297871576 ) ) ;
#16547 = CIRCLE ( 'NONE', #6937, 4.800000000000000711 ) ;
#16548 = AXIS2_PLACEMENT_3D ( 'NONE', #685, #22251, #10344 ) ;
#16549 = CARTESIAN_POINT ( 'NONE',  ( -60.59999999999997300, 1.626093840209163176E-15, 1.891350188320046374E-15 ) ) ;
#16550 = CARTESIAN_POINT ( 'NONE',  ( 31.90749320720292559, 7.645246318246651462, 2.049999999999888356 ) ) ;
#16551 = VERTEX_POINT ( 'NONE', #9599 ) ;
#16552 = VERTEX_POINT ( 'NONE', #19097 ) ;
#16553 = B_SPLINE_CURVE_WITH_KNOTS ( 'NONE', 3,
 ( #8102, #17770, #27410, #25021, #3352, #13002, #30086, #6506, #6659, #6991, #4271, #4122, #26295, #31202, #16653, #7142 ),
 .UNSPECIFIED., .F., .F.,
 ( 4, 3, 3, 3, 3, 4 ),
 ( 0.000000000000000000, 3.350201058276301074E-05, 6.696995785605353631E-05, 0.0001009523001788503553, 0.0001220103457549332620, 0.0001251189910046208303 ),
 .UNSPECIFIED. ) ;
#16554 = CYLINDRICAL_SURFACE ( 'NONE', #11416, 0.09999999999999972800 ) ;
#16555 = CARTESIAN_POINT ( 'NONE',  ( 61.20026580823483187, 0.7453886133013672977, -1.660366360129213348 ) ) ;
#16556 = ORIENTED_EDGE ( 'NONE', *, *, #14820, .F. ) ;
#16557 = AXIS2_PLACEMENT_3D ( 'NONE', #29302, #12808, #24538 ) ;
#16558 = CARTESIAN_POINT ( 'NONE',  ( -58.03335481156722864, 0.7533615035077975142, -3.673546848079180638 ) ) ;
#16559 = DIRECTION ( 'NONE',  ( 1.000000000000000000, 1.047444401652940007E-14, 0.000000000000000000 ) ) ;
#16560 = CIRCLE ( 'NONE', #11990, 1.474464970144730991 ) ;
#16561 = FACE_OUTER_BOUND ( 'NONE', #16706, .T. ) ;
#16562 = CIRCLE ( 'NONE', #15531, 1.000000000000000000 ) ;
#16563 = CARTESIAN_POINT ( 'NONE',  ( 58.65000000000004121, -1.782657835994308604, 0.5811678240972268927 ) ) ;
#16565 = DIRECTION ( 'NONE',  ( 1.000000000000000000, 1.047444401652940007E-14, 0.000000000000000000 ) ) ;
#16564 = CARTESIAN_POINT ( 'NONE',  ( -36.04518387042615046, -2.525801254963603526, 4.794550361020572637 ) ) ;
#16566 = CARTESIAN_POINT ( 'NONE',  ( 50.95599726996783829, 0.9532299437236954054, 1.316046228059489120 ) ) ;
#16567 = CARTESIAN_POINT ( 'NONE',  ( -67.97846802697301882, -0.6530782982312804963, 3.184545152421074388 ) ) ;
#16568 = CIRCLE ( 'NONE', #9501, 0.01000000000000001929 ) ;
#16569 = ADVANCED_FACE ( 'NONE', ( #28747 ), #19506, .T. ) ;
#16570 = DIRECTION ( 'NONE',  ( -1.000000000000000000, -0.000000000000000000, -0.000000000000000000 ) ) ;
#16571 = AXIS2_PLACEMENT_3D ( 'NONE', #22434, #22600, #10235 ) ;
#16572 = VECTOR ( 'NONE', #5195, 1000.000000000000000 ) ;
#16573 = ORIENTED_EDGE ( 'NONE', *, *, #23952, .F. ) ;
#16574 = EDGE_CURVE ( 'NONE', #15271, #28412, #4346, .T. ) ;
#16575 = ORIENTED_EDGE ( 'NONE', *, *, #25114, .F. ) ;
#16576 = CARTESIAN_POINT ( 'NONE',  ( 31.35411506839069062, 7.935106539330317510, -1.425000000000109068 ) ) ;
#16577 = ORIENTED_EDGE ( 'NONE', *, *, #2933, .T. ) ;
#16578 = CARTESIAN_POINT ( 'NONE',  ( 53.66827364943468126, 4.678978782231800082, 2.049999999999812861 ) ) ;
#16579 = CARTESIAN_POINT ( 'NONE',  ( -59.78335481156722864, -4.108500314926510022, 1.367561758111408121 ) ) ;
#16581 = CARTESIAN_POINT ( 'NONE',  ( -36.25997906085253675, 3.232943006030361666, 4.078682900256771937 ) ) ;
#16580 = CARTESIAN_POINT ( 'NONE',  ( 50.87477060347373481, 8.633605004118185988, -2.008578643762867433 ) ) ;
#16582 = VECTOR ( 'NONE', #22158, 1000.000000000000000 ) ;
#16583 = ORIENTED_EDGE ( 'NONE', *, *, #25661, .F. ) ;
#16584 = EDGE_LOOP ( 'NONE', ( #20515, #3054, #30617, #22138 ) ) ;
#16585 = DIRECTION ( 'NONE',  ( 0.000000000000000000, -8.881784197001054122E-16, 1.000000000000000000 ) ) ;
#16586 = VECTOR ( 'NONE', #22309, 1000.000000000000000 ) ;
#16587 = EDGE_LOOP ( 'NONE', ( #27576, #14109 ) ) ;
#16588 = DIRECTION ( 'NONE',  ( 0.000000000000000000, -1.000000000000000000, -3.491481338843133355E-15 ) ) ;
#16589 = EDGE_CURVE ( 'NONE', #24092, #21049, #14238, .T. ) ;
#16590 = AXIS2_PLACEMENT_3D ( 'NONE', #14683, #21978, #22142 ) ;
#16591 = ORIENTED_EDGE ( 'NONE', *, *, #15428, .F. ) ;
#16593 = DIRECTION ( 'NONE',  ( 3.246618580117018983E-15, -0.3099561728520988102, -0.9507508458638782578 ) ) ;
#16592 = CARTESIAN_POINT ( 'NONE',  ( 50.49731436448253419, 0.9333771270347341886, 3.994943142064453667 ) ) ;
#16594 = VERTEX_POINT ( 'NONE', #16082 ) ;
#16595 = CARTESIAN_POINT ( 'NONE',  ( 53.61178743402152946, 7.592121589695717709, 1.856625336930636250 ) ) ;
#16596 = FACE_OUTER_BOUND ( 'NONE', #4718, .T. ) ;
#16597 = CIRCLE ( 'NONE', #18110, 2.700000000000000178 ) ;
#16598 = CARTESIAN_POINT ( 'NONE',  ( -54.49646078629579193, -1.531523113441620731, -3.320331042554033552 ) ) ;
#16599 = CARTESIAN_POINT ( 'NONE',  ( -58.94702994616203284, -2.078460969082631227, -3.600000000000215472 ) ) ;
#16600 = EDGE_CURVE ( 'NONE', #355, #28086, #17981, .T. ) ;
#16601 = DIRECTION ( 'NONE',  ( 1.000000000000000000, -0.000000000000000000, 0.000000000000000000 ) ) ;
#16602 = CARTESIAN_POINT ( 'NONE',  ( 24.05318950685000701, 5.396204383593524057, 1.549999999999915890 ) ) ;
#16603 = FACE_OUTER_BOUND ( 'NONE', #7749, .T. ) ;
#16604 = CIRCLE ( 'NONE', #28741, 0.05000000000000012768 ) ;
#16605 = CARTESIAN_POINT ( 'NONE',  ( -56.23542740578359656, -3.725040285533366191, 1.239922660687671652 ) ) ;
#16606 = ADVANCED_FACE ( 'NONE', ( #2133 ), #26065, .T. ) ;
#16607 = CARTESIAN_POINT ( 'NONE',  ( 58.75000000000002132, -0.6373668173463985509, -1.895722432252557432 ) ) ;
#16608 = EDGE_CURVE ( 'NONE', #14417, #4801, #16459, .T. ) ;
#16609 = ORIENTED_EDGE ( 'NONE', *, *, #17593, .T. ) ;
#16610 = ADVANCED_FACE ( 'NONE', ( #13997 ), #11305, .F. ) ;
#16611 = DIRECTION ( 'NONE',  ( 3.489354422748178582E-15, -1.218509414717996338E-16, 1.000000000000000000 ) ) ;
#16612 = CARTESIAN_POINT ( 'NONE',  ( 52.69133855403836009, 4.542743498088711362, 1.570391066185332196 ) ) ;
#16613 = CARTESIAN_POINT ( 'NONE',  ( 58.75000000000003553, -1.470078920827206925, -1.470078920827526892 ) ) ;
#16614 = EDGE_LOOP ( 'NONE', ( #12652, #17460, #17416, #27017 ) ) ;
#16615 = B_SPLINE_CURVE_WITH_KNOTS ( 'NONE', 3,
 ( #11837, #31151, #28786, #4864, #7100, #16761, #2338, #19298, #28933, #24195, #2500, #15456, #22907, #3267, #22763, #3438 ),
 .UNSPECIFIED., .F., .F.,
 ( 4, 2, 2, 2, 2, 2, 2, 4 ),
 ( 0.000000000000000000, 0.0004351083927046413432, 0.0008702167854092826864, 0.001740433570818565373, 0.002175541963523206553, 0.002610650356227847951, 0.003045758748932489348, 0.003480867141637130745 ),
 .UNSPECIFIED. ) ;
#16616 = CARTESIAN_POINT ( 'NONE',  ( -54.47710365256552478, 1.507983431629474014, 4.035431478432993657 ) ) ;
#16617 = ORIENTED_EDGE ( 'NONE', *, *, #12156, .F. ) ;
#16618 = LINE ( 'NONE', #14214, #28382 ) ;
#16620 = CARTESIAN_POINT ( 'NONE',  ( 51.70000000000001705, -3.726179070414207928, 1.000000000000000444 ) ) ;
#16619 = CARTESIAN_POINT ( 'NONE',  ( -71.44781903063172024, -1.379665415900875831E-15, 2.906523147574707464E-15 ) ) ;
#16621 = ORIENTED_EDGE ( 'NONE', *, *, #21381, .F. ) ;
#16622 = ORIENTED_EDGE ( 'NONE', *, *, #16787, .F. ) ;
#16623 = CARTESIAN_POINT ( 'NONE',  ( 58.65000000000001279, 0.8948927608039191073, -1.760622601996761460 ) ) ;
#16624 = LINE ( 'NONE', #26268, #27795 ) ;
#16626 = DIRECTION ( 'NONE',  ( 3.491481338843133355E-15, 3.491481338843133355E-15, -1.000000000000000000 ) ) ;
#16625 = DIRECTION ( 'NONE',  ( 1.000000000000000000, 0.000000000000000000, -0.000000000000000000 ) ) ;
#16627 = ORIENTED_EDGE ( 'NONE', *, *, #29026, .F. ) ;
#16628 = CARTESIAN_POINT ( 'NONE',  ( -59.86042740578359656, -2.936324665650201116, -2.606018187048497303 ) ) ;
#16629 = CARTESIAN_POINT ( 'NONE',  ( 15.97944027357901398, 3.614202567156016954, -4.024415706308015928 ) ) ;
#16630 = DIRECTION ( 'NONE',  ( 0.000000000000000000, -0.2008964009354147762, 0.9796124928211139560 ) ) ;
#16631 = CIRCLE ( 'NONE', #8022, 0.1000000000000001166 ) ;
#16632 = DIRECTION ( 'NONE',  ( -1.000000000000000000, -3.054027077731387480E-16, 2.042479963029832083E-16 ) ) ;
#16633 = MECHANICAL_DESIGN_GEOMETRIC_PRESENTATION_REPRESENTATION (  '', ( #21708 ), #1945 ) ;
#16634 = B_SPLINE_CURVE_WITH_KNOTS ( 'NONE', 3,
 ( #10127, #14571, #12489, #22016 ),
 .UNSPECIFIED., .F., .F.,
 ( 4, 4 ),
 ( 0.000000000000000000, 0.0003408895603972702908 ),
 .UNSPECIFIED. ) ;
#16635 = CARTESIAN_POINT ( 'NONE',  ( -61.37588895521345478, -2.622661570964761157, -0.6163042711484312264 ) ) ;
#16636 = DIRECTION ( 'NONE',  ( 0.000000000000000000, 0.000000000000000000, -1.000000000000000000 ) ) ;
#16637 =( BOUNDED_CURVE ( )  B_SPLINE_CURVE ( 2, ( #14432, #11909, #44, #31235, #9562, #1944, #14599, #21287, #9707 ),
 .UNSPECIFIED., .F., .T. ) 
 B_SPLINE_CURVE_WITH_KNOTS ( ( 3, 2, 2, 2, 3 ),
 ( 0.5833333333333333703, 0.5925925925925925597, 0.6111111111111111605, 0.6296296296296296502, 0.6388888888888889506 ),
 .UNSPECIFIED. ) 
 CURVE ( )  GEOMETRIC_REPRESENTATION_ITEM ( )  RATIONAL_B_SPLINE_CURVE ( ( 0.9330127018922194093, 0.9330127018922197424, 1.000000000000000000, 0.8660254037844387076, 1.000000000000000000, 0.8660254037844387076, 1.000000000000000000, 0.9330127018922189652, 0.9330127018922194093 ) ) 
 REPRESENTATION_ITEM ( '' )  );
#16638 = B_SPLINE_CURVE_WITH_KNOTS ( 'NONE', 3,
 ( #26943, #17000, #17449, #2729, #24729, #29465, #19835, #29017, #22221, #9718 ),
 .UNSPECIFIED., .F., .F.,
 ( 4, 2, 2, 2, 4 ),
 ( 0.000000000000000000, 0.0001518620921315108662, 0.0002277931381972662993, 0.0002657586612301437176, 0.0003037241842630211902 ),
 .UNSPECIFIED. ) ;
#16639 = FACE_OUTER_BOUND ( 'NONE', #12726, .T. ) ;
#16640 = EDGE_CURVE ( 'NONE', #27693, #18790, #11755, .T. ) ;
#16641 = ORIENTED_EDGE ( 'NONE', *, *, #20492, .T. ) ;
#16642 = CARTESIAN_POINT ( 'NONE',  ( -56.97099364905386665, -0.2309624077928983110, -3.875409454552788624 ) ) ;
#16643 = EDGE_CURVE ( 'NONE', #12544, #16052, #11485, .T. ) ;
#16644 = CARTESIAN_POINT ( 'NONE',  ( -36.92362342067259107, 3.046685255238509971, -4.470266847516099595 ) ) ;
#16645 = CARTESIAN_POINT ( 'NONE',  ( 48.40115653635459125, 0.8930148142854623661, 3.925689827643446428 ) ) ;
#16646 = FACE_OUTER_BOUND ( 'NONE', #28116, .T. ) ;
#16647 = DIRECTION ( 'NONE',  ( 0.000000000000000000, 3.552713678800500929E-15, 1.000000000000000000 ) ) ;
#16649 = CARTESIAN_POINT ( 'NONE',  ( -35.85663232820584767, 5.377732432866621615, 0.5657657256216177544 ) ) ;
#16648 = FACE_OUTER_BOUND ( 'NONE', #2394, .T. ) ;
#16650 = EDGE_CURVE ( 'NONE', #30639, #17367, #8938, .T. ) ;
#16651 = CARTESIAN_POINT ( 'NONE',  ( -62.04999999999998295, -2.671081280896084653, -0.3941126626315447634 ) ) ;
#16653 = CARTESIAN_POINT ( 'NONE',  ( -59.60101405528192942, 2.022629942802355973, 1.712153077242869470 ) ) ;
#16652 = CARTESIAN_POINT ( 'NONE',  ( 69.05000000000005400, 4.557543281186736018E-17, 3.020710678117922932 ) ) ;
#16654 = ORIENTED_EDGE ( 'NONE', *, *, #541, .F. ) ;
#16655 = VECTOR ( 'NONE', #31074, 1000.000000000000000 ) ;
#16656 = CARTESIAN_POINT ( 'NONE',  ( 58.66133336607637716, 0.9092995659220839411, -1.640092727267648876 ) ) ;
#16657 = CARTESIAN_POINT ( 'NONE',  ( 51.80000000000001847, 2.428612866367529932E-14, -1.808587333520743709E-13 ) ) ;
#16659 = CARTESIAN_POINT ( 'NONE',  ( -36.31440869660546156, 4.928592478219054662, 1.658905555082685668 ) ) ;
#16658 = FACE_OUTER_BOUND ( 'NONE', #1127, .T. ) ;
#16660 = CARTESIAN_POINT ( 'NONE',  ( 15.41170998834821226, -4.895911367890834143, 2.323639554370769300 ) ) ;
#16661 = VERTEX_POINT ( 'NONE', #6576 ) ;
#16662 = ORIENTED_EDGE ( 'NONE', *, *, #22032, .F. ) ;
#16663 = CARTESIAN_POINT ( 'NONE',  ( 51.25834959657160539, -0.9980676081275761113, -1.403333189220955068 ) ) ;
#16664 = ORIENTED_EDGE ( 'NONE', *, *, #19942, .F. ) ;
#16665 = PLANE ( 'NONE',  #20607 ) ;
#16666 = DIRECTION ( 'NONE',  ( 0.000000000000000000, 0.000000000000000000, -1.000000000000000000 ) ) ;
#16667 = CIRCLE ( 'NONE', #25752, 2.600000000000000089 ) ;
#16668 = ORIENTED_EDGE ( 'NONE', *, *, #12914, .T. ) ;
#16669 = CARTESIAN_POINT ( 'NONE',  ( 58.65844932252359456, 1.874781853997842251, 0.03312599131522728224 ) ) ;
#16670 = ORIENTED_EDGE ( 'NONE', *, *, #2634, .F. ) ;
#16671 = DIRECTION ( 'NONE',  ( 0.000000000000000000, 0.000000000000000000, 1.000000000000000000 ) ) ;
#16672 = DIRECTION ( 'NONE',  ( 9.188425696205898615E-15, 0.000000000000000000, 1.000000000000000000 ) ) ;
#16673 = ADVANCED_FACE ( 'NONE', ( #4187 ), #13825, .T. ) ;
#16674 = EDGE_LOOP ( 'NONE', ( #5914, #11003, #20547, #6169 ) ) ;
#16675 = AXIS2_PLACEMENT_3D ( 'NONE', #2861, #20139, #15524 ) ;
#16676 = EDGE_CURVE ( 'NONE', #1750, #13697, #17483, .T. ) ;
#16677 = AXIS2_PLACEMENT_3D ( 'NONE', #7456, #5219, #14867 ) ;
#16678 = CARTESIAN_POINT ( 'NONE',  ( -55.07202994616204705, 2.078460969082674747, -3.600000000000187494 ) ) ;
#16679 = EDGE_CURVE ( 'NONE', #22168, #28767, #810, .T. ) ;
#16680 = DIRECTION ( 'NONE',  ( -1.000000000000000000, -1.047444401652940007E-14, -0.000000000000000000 ) ) ;
#16681 = CARTESIAN_POINT ( 'NONE',  ( -44.49999999999999289, 1.499999999999999556, 4.029888335921975262 ) ) ;
#16682 = LINE ( 'NONE', #1610, #10915 ) ;
#16683 = CYLINDRICAL_SURFACE ( 'NONE', #30705, 4.600000000000036948 ) ;
#16685 = CARTESIAN_POINT ( 'NONE',  ( -57.87499999999997158, -3.673546848079170424, -0.7533615035078229383 ) ) ;
#16684 = DIRECTION ( 'NONE',  ( 0.000000000000000000, -1.000000000000000000, -0.000000000000000000 ) ) ;
#16686 = DIRECTION ( 'NONE',  ( 1.000000000000000000, 0.000000000000000000, -3.491481338843133355E-15 ) ) ;
#16687 = FACE_OUTER_BOUND ( 'NONE', #7949, .T. ) ;
#16688 = DIRECTION ( 'NONE',  ( -3.489354422748178582E-15, 1.218509414717996338E-16, -1.000000000000000000 ) ) ;
#16689 = EDGE_CURVE ( 'NONE', #31001, #3318, #1802, .T. ) ;
#16690 = ORIENTED_EDGE ( 'NONE', *, *, #25578, .T. ) ;
#16691 = DIRECTION ( 'NONE',  ( -1.000000000000000000, -3.054025858079668409E-16, 2.042474015755241579E-16 ) ) ;
#16692 = DIRECTION ( 'NONE',  ( 1.000000000000000000, -1.219044193948983948E-29, 3.491481338843133355E-15 ) ) ;
#16694 = DIRECTION ( 'NONE',  ( 1.000000000000000000, 1.047444401652940007E-14, 0.000000000000000000 ) ) ;
#16693 = CARTESIAN_POINT ( 'NONE',  ( 48.43920370478603843, -1.278211010209444387, 3.870212229389975445 ) ) ;
#16695 = CARTESIAN_POINT ( 'NONE',  ( 54.18857836506865056, 5.673639474816032369, -2.050000000000188116 ) ) ;
#16696 = CARTESIAN_POINT ( 'NONE',  ( 51.70000000000000284, -3.609862487194767766, -1.947526779791158624 ) ) ;
#16697 = AXIS2_PLACEMENT_3D ( 'NONE', #29910, #27857, #6168 ) ;
#16698 = CIRCLE ( 'NONE', #3023, 0.1499999999999998557 ) ;
#16699 = VERTEX_POINT ( 'NONE', #17477 ) ;
#16700 = CARTESIAN_POINT ( 'NONE',  ( 36.50000000000002132, 0.000000000000000000, 0.000000000000000000 ) ) ;
#16701 = CARTESIAN_POINT ( 'NONE',  ( 22.58314801556725371, 7.622751244490532763, 1.424999999999921663 ) ) ;
#16702 = CARTESIAN_POINT ( 'NONE',  ( -55.44702994616206126, -2.078460969082657872, 3.599999999999794920 ) ) ;
#16703 = ORIENTED_EDGE ( 'NONE', *, *, #23282, .F. ) ;
#16704 = ORIENTED_EDGE ( 'NONE', *, *, #30959, .F. ) ;
#16705 = FACE_OUTER_BOUND ( 'NONE', #19620, .T. ) ;
#16706 = EDGE_LOOP ( 'NONE', ( #17641, #27490, #2343, #3094 ) ) ;
#16707 = CIRCLE ( 'NONE', #3030, 0.09999999999999997780 ) ;
#16708 = CARTESIAN_POINT ( 'NONE',  ( 52.08333333333335702, 4.368973594129894167, 1.439468559502539824 ) ) ;
#16709 = CARTESIAN_POINT ( 'NONE',  ( -56.38452994616205416, 3.117691453623979481, 1.799999999999811751 ) ) ;
#16710 = ORIENTED_EDGE ( 'NONE', *, *, #1829, .T. ) ;
#16711 = DIRECTION ( 'NONE',  ( 0.000000000000000000, -0.000000000000000000, -1.000000000000000000 ) ) ;
#16712 = CARTESIAN_POINT ( 'NONE',  ( -35.85663232820584057, -3.275050215668913189, -2.949461045527344893 ) ) ;
#16713 = CARTESIAN_POINT ( 'NONE',  ( 61.25000000000004263, -1.895722432252919809, 0.6373668173470157239 ) ) ;
#16714 = VERTEX_POINT ( 'NONE', #7664 ) ;
#16715 = EDGE_CURVE ( 'NONE', #20326, #26621, #13932, .T. ) ;
#16716 = FACE_OUTER_BOUND ( 'NONE', #3056, .T. ) ;
#16717 = EDGE_CURVE ( 'NONE', #20395, #22807, #27090, .T. ) ;
#16718 = LINE ( 'NONE', #21467, #9889 ) ;
#16719 = CARTESIAN_POINT ( 'NONE',  ( 58.74999999305997278, -0.9867593359911132067, -1.657788420845575983 ) ) ;
#16720 = VERTEX_POINT ( 'NONE', #3068 ) ;
#16721 = CARTESIAN_POINT ( 'NONE',  ( 59.35000000000002984, 1.401298464324817071E-42, -6.216582523810200043E-13 ) ) ;
#16722 = CARTESIAN_POINT ( 'NONE',  ( 58.65000000000001279, 0.5811678240991626776, -1.782657835994492457 ) ) ;
#16723 = CARTESIAN_POINT ( 'NONE',  ( 59.00000000000002132, 1.401298464324817071E-42, -6.179921969752347932E-13 ) ) ;
#16725 = CARTESIAN_POINT ( 'NONE',  ( 47.09453520915243985, 9.265918505097243241, 1.949999999999835865 ) ) ;
#16724 = CARTESIAN_POINT ( 'NONE',  ( 58.65000076404083273, -0.5493821916573800035, -1.793020333199547123 ) ) ;
#16726 = PRODUCT ( 'Twister Head', 'Twister Head', '', ( #18688 ) ) ;
#16727 = AXIS2_PLACEMENT_3D ( 'NONE', #7051, #30789, #14311 ) ;
#16728 = CARTESIAN_POINT ( 'NONE',  ( 58.70142274306405028, -0.4999999999993853805, 1.816042500835558959 ) ) ;
#16729 = DIRECTION ( 'NONE',  ( 3.491481338843133355E-15, 3.491481338843133355E-15, -1.000000000000000000 ) ) ;
#16730 = ADVANCED_FACE ( 'NONE', ( #684 ), #225, .T. ) ;
#16731 = DIRECTION ( 'NONE',  ( -1.000000000000000000, -1.018631342913014973E-14, -0.000000000000000000 ) ) ;
#16732 = VERTEX_POINT ( 'NONE', #12561 ) ;
#16733 = CARTESIAN_POINT ( 'NONE',  ( -59.10192033946857748, -2.331623134809623465, 1.259417044000318286 ) ) ;
#16734 = ORIENTED_EDGE ( 'NONE', *, *, #30775, .F. ) ;
#16735 = CARTESIAN_POINT ( 'NONE',  ( 53.25639650609797116, 8.250950595073881288, 2.049999999999814193 ) ) ;
#16736 = CARTESIAN_POINT ( 'NONE',  ( -54.67292740578360366, -3.330682475591782765, -0.6830477631804114935 ) ) ;
#16738 = CARTESIAN_POINT ( 'NONE',  ( 31.17557021199490919, 8.263885728205480063, -1.575000000000108535 ) ) ;
#16737 = CARTESIAN_POINT ( 'NONE',  ( 50.85906935218976344, 8.675599908283860628, -2.050000000000176570 ) ) ;
#16739 = ORIENTED_EDGE ( 'NONE', *, *, #29024, .T. ) ;
#16740 = ORIENTED_EDGE ( 'NONE', *, *, #5001, .F. ) ;
#16741 = DIRECTION ( 'NONE',  ( -1.000000000000000000, -3.054025858079668409E-16, 2.042474015755241579E-16 ) ) ;
#16742 = ORIENTED_EDGE ( 'NONE', *, *, #24213, .T. ) ;
#16743 = DIRECTION ( 'NONE',  ( 9.754918421198724481E-16, -0.9601771338024399638, 0.2793919678926571892 ) ) ;
#16744 = ORIENTED_EDGE ( 'NONE', *, *, #17993, .F. ) ;
#16745 = CARTESIAN_POINT ( 'NONE',  ( 50.41431699104522579, 1.130504494894959411, 3.941663789486498537 ) ) ;
#16746 = EDGE_LOOP ( 'NONE', ( #1801, #14457, #12341, #14951 ) ) ;
#16747 = DIRECTION ( 'NONE',  ( 3.002035892788117459E-16, -0.9996898646859343485, -0.02490330187381123786 ) ) ;
#16748 = CARTESIAN_POINT ( 'NONE',  ( 57.00381193298470350, 0.7199075706197948232, 1.804244861858284255 ) ) ;
#16749 = VECTOR ( 'NONE', #5444, 1000.000000000000000 ) ;
#16750 = EDGE_CURVE ( 'NONE', #25510, #24537, #31148, .T. ) ;
#16751 = CARTESIAN_POINT ( 'NONE',  ( -54.45996984137642727, -1.500763111530253990, -3.300586169551323668 ) ) ;
#16752 = CARTESIAN_POINT ( 'NONE',  ( -59.51024032614731851, 3.088598804228899652, 1.421463128792039843 ) ) ;
#16753 = CARTESIAN_POINT ( 'NONE',  ( -56.20655989232413674, 1.962990915244722245, 3.399999999999807621 ) ) ;
#16754 = CARTESIAN_POINT ( 'NONE',  ( -59.17998499521433331, -2.518779524791931124, -0.9443209727575352375 ) ) ;
#16755 = SHAPE_REPRESENTATION ( 'Tip', ( #9018 ), #18147 ) ;
#16756 = DIRECTION ( 'NONE',  ( -1.000000000000000000, -0.000000000000000000, 3.491481338843133355E-15 ) ) ;
#16757 = DIRECTION ( 'NONE',  ( -3.489354422748178977E-15, 1.218509414717996338E-16, -1.000000000000000000 ) ) ;
#16758 = PRESENTATION_STYLE_ASSIGNMENT (( #7098 ) ) ;
#16760 = ORIENTED_EDGE ( 'NONE', *, *, #27808, .T. ) ;
#16759 = EDGE_CURVE ( 'NONE', #616, #21818, #18002, .T. ) ;
#16761 = CARTESIAN_POINT ( 'NONE',  ( -36.81959771849334828, -0.5763363385013906548, 5.380853831843025681 ) ) ;
#16762 = VERTEX_POINT ( 'NONE', #14930 ) ;
#16763 = CARTESIAN_POINT ( 'NONE',  ( 22.07280086217094350, 8.086143481909241260, 1.949999999999922906 ) ) ;
#16764 = CARTESIAN_POINT ( 'NONE',  ( 53.44675224545779457, 5.128498479132437282, 1.627483882363299772 ) ) ;
#16765 = CARTESIAN_POINT ( 'NONE',  ( 53.93368094605000351, 6.673923850743078034, 1.889910665294559422 ) ) ;
#16766 = ORIENTED_EDGE ( 'NONE', *, *, #31267, .F. ) ;
#16767 = CARTESIAN_POINT ( 'NONE',  ( -36.00201293083839715, -4.683225679163161459, 2.703237727951724345 ) ) ;
#16768 = ORIENTED_EDGE ( 'NONE', *, *, #6255, .T. ) ;
#16769 = CARTESIAN_POINT ( 'NONE',  ( 16.10705563471230661, -0.1565107631087817031, -5.407502298984290690 ) ) ;
#16771 = CARTESIAN_POINT ( 'NONE',  ( 58.75000018803721247, -1.403930843796483696, 1.333992738917427978 ) ) ;
#16770 = CARTESIAN_POINT ( 'NONE',  ( 58.75000018595669360, 0.9248597378499668897, -1.701752411747084581 ) ) ;
#16772 = ADVANCED_FACE ( 'NONE', ( #24599 ), #22249, .T. ) ;
#16773 = EDGE_LOOP ( 'NONE', ( #19349, #13664, #26952, #3051, #9763, #9253 ) ) ;
#16774 = CARTESIAN_POINT ( 'NONE',  ( 50.87477060347373481, 8.633605004118187765, -1.950000000000176925 ) ) ;
#16775 = DIRECTION ( 'NONE',  ( 1.000000000000000000, 0.000000000000000000, 0.000000000000000000 ) ) ;
#16777 = CARTESIAN_POINT ( 'NONE',  ( 58.66133336607565241, -1.302803168107663945, 1.348863877412472156 ) ) ;
#16776 = CARTESIAN_POINT ( 'NONE',  ( 33.47623932017462778, -1.123735532908268331, 5.289358697221549832 ) ) ;
#16778 = EDGE_LOOP ( 'NONE', ( #7149, #20040, #26345, #6944 ) ) ;
#16779 = CARTESIAN_POINT ( 'NONE',  ( -54.74999999999997868, -1.184343223768585140, -3.558065644182724085 ) ) ;
#16780 = DIRECTION ( 'NONE',  ( 3.491481338843133355E-15, 3.491481338843133355E-15, -1.000000000000000000 ) ) ;
#16781 = DIRECTION ( 'NONE',  ( 2.586136946169074517E-16, -1.000000000000000000, 0.000000000000000000 ) ) ;
#16782 = DIRECTION ( 'NONE',  ( 1.738188194345512309E-16, 0.09652874004297619381, 0.9953301976458442946 ) ) ;
#16783 = CIRCLE ( 'NONE', #9205, 1.240000000000000213 ) ;
#16784 = ADVANCED_FACE ( 'NONE', ( #19863 ), #29491, .T. ) ;
#16785 = CARTESIAN_POINT ( 'NONE',  ( -61.35212117932173470, -2.597517021324610820, -0.5932794490111470420 ) ) ;
#16786 = CARTESIAN_POINT ( 'NONE',  ( 52.06628335902946247, -0.5434431642975682264, 1.794517909405659806 ) ) ;
#16787 = EDGE_CURVE ( 'NONE', #27015, #26621, #7806, .T. ) ;
#16788 = CARTESIAN_POINT ( 'NONE',  ( -54.49409853110120139, 1.525884777627348088, -4.047834655405394777 ) ) ;
#16789 = EDGE_CURVE ( 'NONE', #5317, #5591, #26829, .T. ) ;
#16790 = ORIENTED_EDGE ( 'NONE', *, *, #10347, .T. ) ;
#16791 = FACE_BOUND ( 'NONE', #29474, .T. ) ;
#16792 = CARTESIAN_POINT ( 'NONE',  ( 64.00000000000001421, 1.683889348828776048E-16, 1.374999999999777955 ) ) ;
#16793 = DIRECTION ( 'NONE',  ( 1.000000000000000000, 0.000000000000000000, -3.469446951953611033E-15 ) ) ;
#16794 = CARTESIAN_POINT ( 'NONE',  ( 22.37589498084251716, 6.912581374120083666, -1.950000000000077893 ) ) ;
#16795 = CARTESIAN_POINT ( 'NONE',  ( 51.70000000000003126, -3.933368109459640660, 2.186004417992994497 ) ) ;
#16796 = ADVANCED_FACE ( 'NONE', ( #14479 ), #9742, .F. ) ;
#16797 = CIRCLE ( 'NONE', #20838, 0.1499999999999999667 ) ;
#16799 = CARTESIAN_POINT ( 'NONE',  ( -59.46420457061498865, 3.387909745995675959, -1.102402054833139466 ) ) ;
#16798 = CARTESIAN_POINT ( 'NONE',  ( -59.13463329438567229, 2.488830503680618200, -0.9121239897849973133 ) ) ;
#16800 = CIRCLE ( 'NONE', #26398, 0.1000000000000000472 ) ;
#16801 = CARTESIAN_POINT ( 'NONE',  ( 47.38185894056287140, -4.256263374916362530, -1.450017276182623105 ) ) ;
#16803 = CARTESIAN_POINT ( 'NONE',  ( 61.00000000000002842, -0.8666666666660278739, 1.374595900215364930 ) ) ;
#16802 = CARTESIAN_POINT ( 'NONE',  ( -44.59999999999998721, 1.499999999999998002, 3.363870538531281262 ) ) ;
#16804 = VERTEX_POINT ( 'NONE', #24151 ) ;
#16805 = VECTOR ( 'NONE', #6722, 1000.000000000000000 ) ;
#16806 = CARTESIAN_POINT ( 'NONE',  ( 58.65838214097806258, -1.802220213625042700, 0.5175938701870494985 ) ) ;
#16807 = UNCERTAINTY_MEASURE_WITH_UNIT (LENGTH_MEASURE( 1.000000000000000082E-05 ), #12517, 'distance_accuracy_value', 'NONE');
#16808 = DIRECTION ( 'NONE',  ( 0.000000000000000000, 0.000000000000000000, 1.000000000000000000 ) ) ;
#16810 = CARTESIAN_POINT ( 'NONE',  ( -36.50489844130380845, 5.244794032782563065, 1.329291831544308300 ) ) ;
#16809 = CARTESIAN_POINT ( 'NONE',  ( 15.22780280894127536, -2.525801254963333520, -4.794550361020474050 ) ) ;
#16811 = CARTESIAN_POINT ( 'NONE',  ( 15.87128154250933676, -4.872353571451259135, 2.347449169364598021 ) ) ;
#16812 = EDGE_CURVE ( 'NONE', #17785, #5500, #1112, .T. ) ;
#16813 = ORIENTED_EDGE ( 'NONE', *, *, #20982, .F. ) ;
#16814 = EDGE_LOOP ( 'NONE', ( #8977, #28737, #12583, #1105 ) ) ;
#16815 = CARTESIAN_POINT ( 'NONE',  ( -59.69999999999998153, 2.336591249775839430, 1.750136525132547360 ) ) ;
#16816 = ORIENTED_EDGE ( 'NONE', *, *, #11433, .F. ) ;
#16817 = ADVANCED_FACE ( 'NONE', ( #2612 ), #15491, .T. ) ;
#16818 = CARTESIAN_POINT ( 'NONE',  ( 57.03920447585827702, 0.8156862745098039102, -2.468735688885368429 ) ) ;
#16819 =( BOUNDED_CURVE ( )  B_SPLINE_CURVE ( 2, ( #24218, #29274, #2676, #2530, #29113, #24505, #12179, #12314, #21999 ),
 .UNSPECIFIED., .F., .T. ) 
 B_SPLINE_CURVE_WITH_KNOTS ( ( 3, 2, 2, 2, 3 ),
 ( 0.08333333333333332871, 0.09259259259259258745, 0.1111111111111111049, 0.1296296296296296224, 0.1388888888888888951 ),
 .UNSPECIFIED. ) 
 CURVE ( )  GEOMETRIC_REPRESENTATION_ITEM ( )  RATIONAL_B_SPLINE_CURVE ( ( 0.9330127018922194093, 0.9330127018922194093, 1.000000000000000000, 0.8660254037844387076, 1.000000000000000000, 0.8660254037844387076, 1.000000000000000000, 0.9330127018922191873, 0.9330127018922192983 ) ) 
 REPRESENTATION_ITEM ( '' )  );
#16820 = DIRECTION ( 'NONE',  ( 1.000000000000000000, -1.219044193948983948E-29, 3.491481338843133355E-15 ) ) ;
#16821 = EDGE_LOOP ( 'NONE', ( #6750, #4491, #13525, #2339 ) ) ;
#16822 = CARTESIAN_POINT ( 'NONE',  ( -59.69999999999997442, -3.237160264815294841, -1.238538609462289219 ) ) ;
#16823 = ORIENTED_EDGE ( 'NONE', *, *, #21609, .F. ) ;
#16824 = CARTESIAN_POINT ( 'NONE',  ( -60.70655989232412963, 1.962990915244722245, 3.399999999999792077 ) ) ;
#16825 = ORIENTED_EDGE ( 'NONE', *, *, #9634, .F. ) ;
#16826 = VERTEX_POINT ( 'NONE', #9887 ) ;
#16827 = EDGE_CURVE ( 'NONE', #25794, #1478, #29658, .T. ) ;
#16828 = EDGE_CURVE ( 'NONE', #10689, #3458, #4859, .T. ) ;
#16829 = EDGE_LOOP ( 'NONE', ( #10537, #15607, #13518, #29990 ) ) ;
#16830 = CARTESIAN_POINT ( 'NONE',  ( -55.25952994616203995, -3.117691453623963938, -1.800000000000207434 ) ) ;
#16831 = CARTESIAN_POINT ( 'NONE',  ( 54.23463818034553441, 5.946682447858800735, -2.050000000000189004 ) ) ;
#16832 = CARTESIAN_POINT ( 'NONE',  ( 51.70000000000000995, -3.933368109459640660, -2.186004417993355098 ) ) ;
#16833 = CARTESIAN_POINT ( 'NONE',  ( -54.49865678108456279, -1.537045020190658251, 3.323865043138457320 ) ) ;
#16834 = CARTESIAN_POINT ( 'NONE',  ( -44.49999999999997868, -1.500000000000000222, -3.300094695611020867 ) ) ;
#16836 = DIRECTION ( 'NONE',  ( 0.000000000000000000, 1.000000000000000000, 4.336808689942015369E-15 ) ) ;
#16835 = CARTESIAN_POINT ( 'NONE',  ( -54.54999999999998295, -0.9643027244899872175, 4.702139965541346278 ) ) ;
#16837 = CIRCLE ( 'NONE', #9309, 2.000000000000000000 ) ;
#16838 = CARTESIAN_POINT ( 'NONE',  ( 47.04676887726569134, -4.276948283761179859, 0.9210528638641409804 ) ) ;
#16839 = CARTESIAN_POINT ( 'NONE',  ( 51.12687253673781385, -0.9194130538815391551, -1.491219977510798600 ) ) ;
#16841 = CARTESIAN_POINT ( 'NONE',  ( 54.40000000000001990, 4.041334437186265510E-16, 3.299999999999999822 ) ) ;
#16840 = CARTESIAN_POINT ( 'NONE',  ( 15.03925126672132784, 4.804073783693472599, -2.042134687550301475 ) ) ;
#16842 = EDGE_LOOP ( 'NONE', ( #8198, #17099, #13903, #5226 ) ) ;
#16843 = DIRECTION ( 'NONE',  ( -1.000000000000000000, -0.000000000000000000, -0.000000000000000000 ) ) ;
#16844 = CARTESIAN_POINT ( 'NONE',  ( 69.00000000000001421, 1.401298464324817071E-42, -7.227366371405287181E-13 ) ) ;
#16846 = CARTESIAN_POINT ( 'NONE',  ( -60.44999999999996021, 1.979096954302128589E-15, 6.602471875703214707E-16 ) ) ;
#16845 = DIRECTION ( 'NONE',  ( 1.387778780781445676E-14, 8.673617379884035472E-16, 1.000000000000000000 ) ) ;
#16847 = DIRECTION ( 'NONE',  ( -1.000000000000000000, -1.018631342913014973E-14, -0.000000000000000000 ) ) ;
#16848 = EDGE_CURVE ( 'NONE', #28914, #560, #15976, .T. ) ;
#16849 = ORIENTED_EDGE ( 'NONE', *, *, #10977, .F. ) ;
#16850 = DIRECTION ( 'NONE',  ( 0.000000000000000000, 0.000000000000000000, 1.000000000000000000 ) ) ;
#16851 = EDGE_CURVE ( 'NONE', #26599, #7189, #22765, .T. ) ;
#16852 = ORIENTED_EDGE ( 'NONE', *, *, #13741, .T. ) ;
#16853 = EDGE_CURVE ( 'NONE', #29689, #18916, #3350, .T. ) ;
#16854 = CARTESIAN_POINT ( 'NONE',  ( 60.88854248453741747, 0.6773709096947286845, -1.477839832418263999 ) ) ;
#16855 = CARTESIAN_POINT ( 'NONE',  ( -55.07202994616204705, 2.078460969082674747, -3.600000000000187494 ) ) ;
#16856 = VERTEX_POINT ( 'NONE', #13487 ) ;
#16857 = VERTEX_POINT ( 'NONE', #15579 ) ;
#16858 = CARTESIAN_POINT ( 'NONE',  ( 61.25000000000004263, -1.666164585742961890, 1.106298139390331947 ) ) ;
#16859 = ORIENTED_EDGE ( 'NONE', *, *, #30332, .T. ) ;
#16860 = CARTESIAN_POINT ( 'NONE',  ( -54.49999999999996447, -1.499999999999981126, -3.363870538531692045 ) ) ;
#16861 = CARTESIAN_POINT ( 'NONE',  ( -55.82202994616203995, 2.078460969082674747, -3.600000000000189715 ) ) ;
#16862 = ORIENTED_EDGE ( 'NONE', *, *, #29660, .T. ) ;
#16863 = CARTESIAN_POINT ( 'NONE',  ( 48.50000000000002132, 1.391941090707534023, -3.850000000000022737 ) ) ;
#16864 = FACE_OUTER_BOUND ( 'NONE', #24576, .T. ) ;
#16865 = CARTESIAN_POINT ( 'NONE',  ( 32.27289361194385720, 7.909974131750026061, 2.049999999999887468 ) ) ;
#16866 = ORIENTED_EDGE ( 'NONE', *, *, #28233, .F. ) ;
#16867 = DIRECTION ( 'NONE',  ( 1.000000000000000000, 0.000000000000000000, 0.000000000000000000 ) ) ;
#16868 = CARTESIAN_POINT ( 'NONE',  ( 61.00000000000002132, 6.389410850082937196E-13, 3.111507638930570854E-58 ) ) ;
#16869 = CARTESIAN_POINT ( 'NONE',  ( 58.66118217212513031, -0.9521303665436844366, -1.615348343402082110 ) ) ;
#16870 = VERTEX_POINT ( 'NONE', #3837 ) ;
#16871 = CARTESIAN_POINT ( 'NONE',  ( -59.19999999999996732, -3.264622394567714192, -0.9498634748674711359 ) ) ;
#16872 = CARTESIAN_POINT ( 'NONE',  ( 57.00914817631336717, 0.7715555436188452632, 1.736293111776144205 ) ) ;
#16874 = DIRECTION ( 'NONE',  ( 1.000000000000000000, 0.000000000000000000, 0.000000000000000000 ) ) ;
#16873 = FILL_AREA_STYLE ('',( #14642 ) ) ;
#16875 = DIRECTION ( 'NONE',  ( -2.581436205204234499E-16, 0.9796124928211140670, 0.2008964009354147762 ) ) ;
#16876 = CARTESIAN_POINT ( 'NONE',  ( 53.74478519188839698, 7.379842749953417602, 2.049999999999939426 ) ) ;
#16877 = CIRCLE ( 'NONE', #8748, 4.100000000000022737 ) ;
#16878 = EDGE_LOOP ( 'NONE', ( #28698, #9265, #16532, #29374 ) ) ;
#16879 = AXIS2_PLACEMENT_3D ( 'NONE', #21441, #2256, #1775 ) ;
#16880 = EDGE_CURVE ( 'NONE', #4682, #17943, #22577, .T. ) ;
#16881 = ORIENTED_EDGE ( 'NONE', *, *, #11244, .T. ) ;
#16882 = DIRECTION ( 'NONE',  ( -1.000000000000000000, 1.219044193948983948E-29, -3.491481338843133355E-15 ) ) ;
#16883 = ORIENTED_EDGE ( 'NONE', *, *, #10176, .T. ) ;
#16884 = FACE_OUTER_BOUND ( 'NONE', #18016, .T. ) ;
#16885 = CARTESIAN_POINT ( 'NONE',  ( -60.03335481156722864, 3.238593381231847257, 2.874284765127023356 ) ) ;
#16887 = LINE ( 'NONE', #241, #16522 ) ;
#16886 = DIRECTION ( 'NONE',  ( 0.000000000000000000, 0.000000000000000000, 1.000000000000000000 ) ) ;
#16888 = ORIENTED_EDGE ( 'NONE', *, *, #21365, .F. ) ;
#16889 = ORIENTED_EDGE ( 'NONE', *, *, #14247, .F. ) ;
#16890 = DIRECTION ( 'NONE',  ( 0.000000000000000000, -0.9996898646859343485, -0.02490330187381124133 ) ) ;
#16891 = ORIENTED_EDGE ( 'NONE', *, *, #23699, .F. ) ;
#16892 = CARTESIAN_POINT ( 'NONE',  ( 33.05069135236685440, 8.148093138862860130, 1.949999999999884270 ) ) ;
#16893 = ORIENTED_EDGE ( 'NONE', *, *, #13, .F. ) ;
#16894 = CARTESIAN_POINT ( 'NONE',  ( 50.35370852371426764, 1.309359793766484925, 3.864871860988134955 ) ) ;
#16895 = ORIENTED_EDGE ( 'NONE', *, *, #12404, .F. ) ;
#16896 = CARTESIAN_POINT ( 'NONE',  ( 57.02114622761336449, -0.7499999999999982236, 1.778341845356538498 ) ) ;
#16897 = CARTESIAN_POINT ( 'NONE',  ( 57.00965563974653350, 0.7295352771400042124, 1.796193723857490321 ) ) ;
#16898 = ADVANCED_FACE ( 'NONE', ( #29821 ), #10972, .F. ) ;
#16899 = CARTESIAN_POINT ( 'NONE',  ( 56.95000076968187130, 0.7321971888534951622, -1.754073505128400878 ) ) ;
#16901 = CARTESIAN_POINT ( 'NONE',  ( -54.39405989232412253, -2.944486372867076263, -1.700000000000203793 ) ) ;
#16900 = VECTOR ( 'NONE', #6351, 1000.000000000000000 ) ;
#16902 = CARTESIAN_POINT ( 'NONE',  ( -59.29999999999997584, -2.208048483361063852, 2.585444235547710967 ) ) ;
#16903 = FACE_OUTER_BOUND ( 'NONE', #8884, .T. ) ;
#16904 = CARTESIAN_POINT ( 'NONE',  ( -44.59999999999998010, 2.750000000000007994, -1.493937157852515840E-13 ) ) ;
#16905 = CIRCLE ( 'NONE', #3244, 2.800000000000000266 ) ;
#16906 = DIRECTION ( 'NONE',  ( 0.000000000000000000, 0.2008964009354147762, -0.9796124928211140670 ) ) ;
#16907 = CARTESIAN_POINT ( 'NONE',  ( 54.28867365409861634, 5.640057820322912363, 1.949999999999809885 ) ) ;
#16908 = ORIENTED_EDGE ( 'NONE', *, *, #1862, .T. ) ;
#16909 = DIRECTION ( 'NONE',  ( 1.000000000000000000, 0.000000000000000000, -1.047444401652940007E-14 ) ) ;
#16910 = CARTESIAN_POINT ( 'NONE',  ( 53.81457038914302871, 5.799118248596165870, 1.689328270749656191 ) ) ;
#16911 = CARTESIAN_POINT ( 'NONE',  ( 53.91582462592153746, 6.672259099522125148, 1.484311102127795712 ) ) ;
#16912 = AXIS2_PLACEMENT_3D ( 'NONE', #148, #26576, #7725 ) ;
#16913 = ORIENTED_EDGE ( 'NONE', *, *, #30042, .T. ) ;
#16914 = ADVANCED_FACE ( 'NONE', ( #25226, #27760 ), #3544, .T. ) ;
#16915 = CARTESIAN_POINT ( 'NONE',  ( -67.33025350686975230, -2.149980434289362918, -0.05355822207391593842 ) ) ;
#16916 = ORIENTED_EDGE ( 'NONE', *, *, #26456, .F. ) ;
#16917 = EDGE_CURVE ( 'NONE', #7081, #20639, #15729, .T. ) ;
#16918 = CARTESIAN_POINT ( 'NONE',  ( 16.07512358269906372, -0.3169205264062066596, -5.400007398663871250 ) ) ;
#16919 = CIRCLE ( 'NONE', #3256, 1.875000000000000000 ) ;
#16921 = CARTESIAN_POINT ( 'NONE',  ( 47.54826167791131297, -3.873874536552758041, -1.343508358799555991 ) ) ;
#16920 = CARTESIAN_POINT ( 'NONE',  ( -57.56249999999995737, -1.962990915244702039, -3.400000000000213962 ) ) ;
#16922 = ORIENTED_EDGE ( 'NONE', *, *, #28236, .T. ) ;
#16923 = DIRECTION ( 'NONE',  ( -0.000000000000000000, -0.000000000000000000, -1.000000000000000000 ) ) ;
#16924 = CARTESIAN_POINT ( 'NONE',  ( 51.01608411450971658, 0.7569233679480920074, -1.030722644926826082 ) ) ;
#16926 = CARTESIAN_POINT ( 'NONE',  ( 58.72200624034175576, 0.9185080301422264837, 1.634766674884828852 ) ) ;
#16925 = DIRECTION ( 'NONE',  ( -1.000000000000000000, -2.586136946169074517E-16, 0.000000000000000000 ) ) ;
#16927 = ORIENTED_EDGE ( 'NONE', *, *, #25707, .F. ) ;
#16928 = CARTESIAN_POINT ( 'NONE',  ( -60.86042740578358945, -0.7887156198831608567, 3.845940847736174728 ) ) ;
#16929 = AXIS2_PLACEMENT_3D ( 'NONE', #20835, #14165, #26205 ) ;
#16930 = CARTESIAN_POINT ( 'NONE',  ( 36.50000000000002132, 0.000000000000000000, -1.850000000000000089 ) ) ;
#16931 = CARTESIAN_POINT ( 'NONE',  ( 46.92012738450930698, -4.254270342444942621, -1.021450466989925587 ) ) ;
#16932 = CARTESIAN_POINT ( 'NONE',  ( 15.71019289815287934, -2.413203405699221094, -4.840238007535771381 ) ) ;
#16933 = ADVANCED_FACE ( 'NONE', ( #15870 ), #29144, .F. ) ;
#16934 = CARTESIAN_POINT ( 'NONE',  ( -59.51260631243411581, 2.329131096718564553, 1.425561137250796362 ) ) ;
#16935 =( BOUNDED_SURFACE ( )  B_SPLINE_SURFACE ( 1, 2, ( 
 ( #22445, #22916, #3452, #13088, #29548, #22774, #18009, #27658, #13231, #5655, #5986, #5502, #15637, #1205, #587, #10246, #741, #10402, #20083, #29722, #8034, #17701, #11663, #13701, #3734, #23383, #30817, #1834, #11507, #28285, #9134, #18798, #6744, #13551, #6131, #27962, #15923, #4207, #26057, #3902, #11325, #21187, #11183, #6597, #6442, #23233, #28441, #1522, #21011, #4367, #30184, #8499, #13377, #28119, #27822, #8961, #23707, #20857, #8645, #30485, #25902, #13845, #14016, #1666, #1997, #16405, #18180, #8788, #15783, #25432, #23073, #30649, #6276, #18641, #16255, #23534, #1369, #16103, #11035, #20710, #30340, #18325, #25584, #18480, #25751, #4058, #28763, #7221, #7073, #2767, #19274, #16579, #24168, #26526, #2305, #16885, #21809, #30970, #19418, #4834, #9904, #6914, #28910, #2477, #5148, #29223, #12270, #26702, #21487 ),
 ( #21954, #7538, #14181, #2626, #24318, #18951, #16736, #28597, #14498, #239, #14334, #9755, #26378, #31120, #9453, #12131, #26224, #9288, #4530, #21341, #9616, #19585, #24004, #17198, #98, #4679, #4997, #11972, #26842, #14798, #29063, #23856, #2149, #24458, #7371, #21659, #11812, #19118, #14655, #31287, #17052, #17498, #24919, #3412, #24775, #10534, #20037, #5467, #1031, #27153, #3238, #8298, #12417, #22114, #26985, #10360, #10064, #22568, #5943, #15117, #22266, #3084, #8150, #27457, #27615, #27310, #17966, #22735, #15424, #12732, #10680, #13052, #15597, #15273, #10209, #12880, #875, #20208, #25243, #29681, #17821, #29838, #5291, #5623, #20364, #5772, #25076, #29987, #19878, #8000, #29508, #404, #17663, #7679, #19738, #29367, #22409, #17339, #14948, #24618, #2935, #12579, #552, #7822, #700, #6396, #18760, #11461, #25865 ) ),
 .UNSPECIFIED., .F., .F., .F. ) 
 B_SPLINE_SURFACE_WITH_KNOTS ( ( 2, 2 ),
 ( 3, 2, 2, 2, 2, 2, 2, 2, 2, 2, 2, 2, 2, 2, 2, 2, 2, 2, 2, 2, 2, 2, 2, 2, 2, 2, 2, 2, 2, 2, 2, 2, 2, 2, 2, 2, 2, 2, 2, 2, 2, 2, 2, 2, 2, 2, 2, 2, 2, 2, 2, 2, 2, 2, 3 ),
 ( 0.000000000000000000, 1.000000000000000000 ),
 ( 0.000000000000000000, 0.01851851851851851749, 0.03703703703703703498, 0.05555555555555555247, 0.07407407407407406996, 0.09259259259259258745, 0.1111111111111111049, 0.1296296296296296224, 0.1481481481481481399, 0.1666666666666666574, 0.1851851851851851749, 0.2037037037037036924, 0.2222222222222222099, 0.2407407407407407274, 0.2592592592592592449, 0.2777777777777777901, 0.2962962962962962798, 0.3148148148148148251, 0.3333333333333333148, 0.3518518518518518601, 0.3703703703703703498, 0.3888888888888888951, 0.4074074074074073848, 0.4259259259259259300, 0.4444444444444444198, 0.4629629629629629650, 0.4814814814814814548, 0.5000000000000000000, 0.5185185185185184897, 0.5370370370370370905, 0.5555555555555555802, 0.5740740740740740700, 0.5925925925925925597, 0.6111111111111111605, 0.6296296296296296502, 0.6481481481481481399, 0.6666666666666666297, 0.6851851851851852304, 0.7037037037037037202, 0.7222222222222222099, 0.7407407407407406996, 0.7592592592592593004, 0.7777777777777777901, 0.7962962962962962798, 0.8148148148148147696, 0.8333333333333333703, 0.8518518518518518601, 0.8703703703703703498, 0.8888888888888888395, 0.9074074074074074403, 0.9259259259259259300, 0.9444444444444444198, 0.9629629629629629095, 0.9814814814814815103, 1.000000000000000000 ),
 .UNSPECIFIED. ) 
 GEOMETRIC_REPRESENTATION_ITEM ( )  RATIONAL_B_SPLINE_SURFACE ( (
 ( 1.000000000000000000, 0.8660254037844387076, 1.000000000000000000, 0.8660254037844387076, 1.000000000000000000, 0.8660254037844387076, 1.000000000000000000, 0.8660254037844387076, 1.000000000000000000, 0.8660254037844387076, 1.000000000000000000, 0.8660254037844387076, 1.000000000000000000, 0.8660254037844387076, 1.000000000000000000, 0.8660254037844387076, 1.000000000000000000, 0.8660254037844387076, 1.000000000000000000, 0.8660254037844387076, 1.000000000000000000, 0.8660254037844387076, 1.000000000000000000, 0.8660254037844387076, 1.000000000000000000, 0.8660254037844387076, 1.000000000000000000, 0.8660254037844387076, 1.000000000000000000, 0.8660254037844387076, 1.000000000000000000, 0.8660254037844387076, 1.000000000000000000, 0.8660254037844387076, 1.000000000000000000, 0.8660254037844387076, 1.000000000000000000, 0.8660254037844387076, 1.000000000000000000, 0.8660254037844387076, 1.000000000000000000, 0.8660254037844387076, 1.000000000000000000, 0.8660254037844387076, 1.000000000000000000, 0.8660254037844387076, 1.000000000000000000, 0.8660254037844387076, 1.000000000000000000, 0.8660254037844387076, 1.000000000000000000, 0.8660254037844387076, 1.000000000000000000, 0.8660254037844387076, 1.000000000000000000, 0.8660254037844387076, 1.000000000000000000, 0.8660254037844387076, 1.000000000000000000, 0.8660254037844387076, 1.000000000000000000, 0.8660254037844387076, 1.000000000000000000, 0.8660254037844387076, 1.000000000000000000, 0.8660254037844387076, 1.000000000000000000, 0.8660254037844387076, 1.000000000000000000, 0.8660254037844387076, 1.000000000000000000, 0.8660254037844387076, 1.000000000000000000, 0.8660254037844387076, 1.000000000000000000, 0.8660254037844387076, 1.000000000000000000, 0.8660254037844387076, 1.000000000000000000, 0.8660254037844387076, 1.000000000000000000, 0.8660254037844387076, 1.000000000000000000, 0.8660254037844387076, 1.000000000000000000, 0.8660254037844387076, 1.000000000000000000, 0.8660254037844387076, 1.000000000000000000, 0.8660254037844387076, 1.000000000000000000, 0.8660254037844387076, 1.000000000000000000, 0.8660254037844387076, 1.000000000000000000, 0.8660254037844387076, 1.000000000000000000, 0.8660254037844387076, 1.000000000000000000, 0.8660254037844387076, 1.000000000000000000, 0.8660254037844387076, 1.000000000000000000, 0.8660254037844387076, 1.000000000000000000, 0.8660254037844387076, 1.000000000000000000, 0.8660254037844387076, 1.000000000000000000),
 ( 1.000000000000000000, 0.8660254037844387076, 1.000000000000000000, 0.8660254037844387076, 1.000000000000000000, 0.8660254037844387076, 1.000000000000000000, 0.8660254037844387076, 1.000000000000000000, 0.8660254037844387076, 1.000000000000000000, 0.8660254037844387076, 1.000000000000000000, 0.8660254037844387076, 1.000000000000000000, 0.8660254037844387076, 1.000000000000000000, 0.8660254037844387076, 1.000000000000000000, 0.8660254037844387076, 1.000000000000000000, 0.8660254037844387076, 1.000000000000000000, 0.8660254037844387076, 1.000000000000000000, 0.8660254037844387076, 1.000000000000000000, 0.8660254037844387076, 1.000000000000000000, 0.8660254037844387076, 1.000000000000000000, 0.8660254037844387076, 1.000000000000000000, 0.8660254037844387076, 1.000000000000000000, 0.8660254037844387076, 1.000000000000000000, 0.8660254037844387076, 1.000000000000000000, 0.8660254037844387076, 1.000000000000000000, 0.8660254037844387076, 1.000000000000000000, 0.8660254037844387076, 1.000000000000000000, 0.8660254037844387076, 1.000000000000000000, 0.8660254037844387076, 1.000000000000000000, 0.8660254037844387076, 1.000000000000000000, 0.8660254037844387076, 1.000000000000000000, 0.8660254037844387076, 1.000000000000000000, 0.8660254037844387076, 1.000000000000000000, 0.8660254037844387076, 1.000000000000000000, 0.8660254037844387076, 1.000000000000000000, 0.8660254037844387076, 1.000000000000000000, 0.8660254037844387076, 1.000000000000000000, 0.8660254037844387076, 1.000000000000000000, 0.8660254037844387076, 1.000000000000000000, 0.8660254037844387076, 1.000000000000000000, 0.8660254037844387076, 1.000000000000000000, 0.8660254037844387076, 1.000000000000000000, 0.8660254037844387076, 1.000000000000000000, 0.8660254037844387076, 1.000000000000000000, 0.8660254037844387076, 1.000000000000000000, 0.8660254037844387076, 1.000000000000000000, 0.8660254037844387076, 1.000000000000000000, 0.8660254037844387076, 1.000000000000000000, 0.8660254037844387076, 1.000000000000000000, 0.8660254037844387076, 1.000000000000000000, 0.8660254037844387076, 1.000000000000000000, 0.8660254037844387076, 1.000000000000000000, 0.8660254037844387076, 1.000000000000000000, 0.8660254037844387076, 1.000000000000000000, 0.8660254037844387076, 1.000000000000000000, 0.8660254037844387076, 1.000000000000000000, 0.8660254037844387076, 1.000000000000000000, 0.8660254037844387076, 1.000000000000000000, 0.8660254037844387076, 1.000000000000000000) ) ) 
 REPRESENTATION_ITEM ( '' )  SURFACE ( )  );
#16936 = CARTESIAN_POINT ( 'NONE',  ( 51.80000000000001137, 6.475000000000062705, -2.050000000000180123 ) ) ;
#16937 = CARTESIAN_POINT ( 'NONE',  ( 36.50000000000002132, 0.000000000000000000, 0.000000000000000000 ) ) ;
#16938 = VECTOR ( 'NONE', #1960, 1000.000000000000000 ) ;
#16940 = ORIENTED_EDGE ( 'NONE', *, *, #28015, .F. ) ;
#16939 = TOROIDAL_SURFACE ( 'NONE', #2279, 1.975000000000001865, 0.1000000000000000056 ) ;
#16941 = DIRECTION ( 'NONE',  ( 1.000000000000000000, 1.047444401652940007E-14, 0.000000000000000000 ) ) ;
#16942 = CARTESIAN_POINT ( 'NONE',  ( 15.66436536804551416, -3.496282614933964528, 4.130238739723520958 ) ) ;
#16943 = DIRECTION ( 'NONE',  ( -3.051840300662039141E-15, -0.4857787595540328796, -0.8740818021021516948 ) ) ;
#16944 = AXIS2_PLACEMENT_3D ( 'NONE', #29104, #2352, #7419 ) ;
#16945 = CARTESIAN_POINT ( 'NONE',  ( 33.37799870938437863, 8.120802762572234101, -1.950000000000116529 ) ) ;
#16946 = EDGE_CURVE ( 'NONE', #2594, #30944, #30641, .T. ) ;
#16947 = CARTESIAN_POINT ( 'NONE',  ( -62.05677242593181120, -2.685607875047633541, 0.2368181935235877944 ) ) ;
#16948 = CIRCLE ( 'NONE', #5821, 0.04999999999999988481 ) ;
#16950 = CARTESIAN_POINT ( 'NONE',  ( 51.80000000000001847, 1.734723475976807094E-15, 0.000000000000000000 ) ) ;
#16949 = CARTESIAN_POINT ( 'NONE',  ( 58.64999999999999858, 1.278133834460348783, 1.372267738821557836 ) ) ;
#16951 = CARTESIAN_POINT ( 'NONE',  ( 61.24179192282288398, -0.9092026280833716001, 1.724287941705032523 ) ) ;
#16952 = CARTESIAN_POINT ( 'NONE',  ( 50.38154193469294739, -1.153441674035701636, -3.890342980189690270 ) ) ;
#16953 = ORIENTED_EDGE ( 'NONE', *, *, #16245, .T. ) ;
#16954 = ADVANCED_FACE ( 'NONE', ( #1013 ), #20655, .F. ) ;
#16955 = DIRECTION ( 'NONE',  ( -1.000000000000000000, 1.219044193948984088E-29, -3.491481338843133750E-15 ) ) ;
#16956 = ADVANCED_FACE ( 'NONE', ( #28533 ), #23562, .T. ) ;
#16957 = DIRECTION ( 'NONE',  ( 1.000000000000000000, -1.219044193948983948E-29, 3.491481338843133355E-15 ) ) ;
#16959 = DIRECTION ( 'NONE',  ( 1.000000000000000000, 2.586136946169074517E-16, -0.000000000000000000 ) ) ;
#16958 = CYLINDRICAL_SURFACE ( 'NONE', #9469, 4.375000000000000000 ) ;
#16961 = ADVANCED_FACE ( 'NONE', ( #1763 ), #6843, .F. ) ;
#16960 = LINE ( 'NONE', #17126, #25153 ) ;
#16962 = ORIENTED_EDGE ( 'NONE', *, *, #25707, .T. ) ;
#16963 = AXIS2_PLACEMENT_3D ( 'NONE', #23770, #30728, #30546 ) ;
#16964 = EDGE_LOOP ( 'NONE', ( #23893, #21527 ) ) ;
#16965 = CARTESIAN_POINT ( 'NONE',  ( 58.65000000000000568, 1.320082690054481755, -1.469015551796560182 ) ) ;
#16966 = EDGE_LOOP ( 'NONE', ( #6517, #28768, #8295, #18012 ) ) ;
#16967 = CARTESIAN_POINT ( 'NONE',  ( 47.19861448675352023, -4.191665075176588928, 1.623492990430730032 ) ) ;
#16968 = VECTOR ( 'NONE', #2598, 1000.000000000000000 ) ;
#16969 = CARTESIAN_POINT ( 'NONE',  ( -56.37499999999997158, -3.673546848079171756, -0.7533615035078148336 ) ) ;
#16970 = VERTEX_POINT ( 'NONE', #13950 ) ;
#16971 = CARTESIAN_POINT ( 'NONE',  ( -35.85663232820584057, -4.945493884734809775, 1.606888370749721684 ) ) ;
#16972 = ORIENTED_EDGE ( 'NONE', *, *, #19931, .F. ) ;
#16973 = EDGE_CURVE ( 'NONE', #26116, #21148, #6882, .T. ) ;
#16974 = CARTESIAN_POINT ( 'NONE',  ( -59.95655989232412963, 1.962990915244722245, 3.399999999999794742 ) ) ;
#16975 = VERTEX_POINT ( 'NONE', #23649 ) ;
#16976 = CIRCLE ( 'NONE', #11390, 0.1000000000000002554 ) ;
#16977 = EDGE_LOOP ( 'NONE', ( #30605, #4927, #11788, #27579 ) ) ;
#16978 = B_SPLINE_CURVE_WITH_KNOTS ( 'NONE', 3,
 ( #28143, #2020, #11683, #21362 ),
 .UNSPECIFIED., .F., .F.,
 ( 4, 4 ),
 ( 1.045245121249583768E-16, 0.0009258403723363874561 ),
 .UNSPECIFIED. ) ;
#16979 = ORIENTED_EDGE ( 'NONE', *, *, #26722, .F. ) ;
#16980 = CARTESIAN_POINT ( 'NONE',  ( -57.19702994616204705, 4.156921938165313080, -1.880369327726949834E-13 ) ) ;
#16981 = CARTESIAN_POINT ( 'NONE',  ( 54.23473434925103476, 6.620089622897159742, -2.050000000000189004 ) ) ;
#16982 = FACE_OUTER_BOUND ( 'NONE', #24041, .T. ) ;
#16983 = DIRECTION ( 'NONE',  ( 1.000000000000000000, -0.000000000000000000, -1.047444401652940007E-14 ) ) ;
#16984 = EDGE_CURVE ( 'NONE', #24287, #20326, #16682, .T. ) ;
#16985 = VECTOR ( 'NONE', #18040, 1000.000000000000000 ) ;
#16986 = DIRECTION ( 'NONE',  ( -0.1208805777273843918, 0.9926670569371656150, 0.000000000000000000 ) ) ;
#16987 = AXIS2_PLACEMENT_3D ( 'NONE', #2429, #22060, #356 ) ;
#16989 = CARTESIAN_POINT ( 'NONE',  ( -36.68866260399460799, 0.7269167730135268624, -5.359285300587757206 ) ) ;
#16988 = CARTESIAN_POINT ( 'NONE',  ( 51.13341687362843402, -0.9248174436445972812, -1.495576127288424040 ) ) ;
#16990 = CIRCLE ( 'NONE', #26082, 0.09999999999999986677 ) ;
#16991 = CARTESIAN_POINT ( 'NONE',  ( 47.00000000000002842, -4.131056160354152240, 1.100000000000000311 ) ) ;
#16992 = CARTESIAN_POINT ( 'NONE',  ( 48.50000000000002132, 1.391941090707534023, -3.850000000000022737 ) ) ;
#16993 = AXIS2_PLACEMENT_3D ( 'NONE', #15761, #3143, #29739 ) ;
#16995 = CARTESIAN_POINT ( 'NONE',  ( 51.24551381660811700, 1.093420264359095340, -1.202138525661323509 ) ) ;
#16994 = CARTESIAN_POINT ( 'NONE',  ( 15.44631504820159407, 4.878538113278890975, -1.812957040858052871 ) ) ;
#16996 = ORIENTED_EDGE ( 'NONE', *, *, #670, .T. ) ;
#16997 = EDGE_CURVE ( 'NONE', #704, #6604, #5350, .T. ) ;
#16998 = TOROIDAL_SURFACE ( 'NONE', #27073, 2.750000000000000000, 0.1000000000000000056 ) ;
#16999 = ADVANCED_FACE ( 'NONE', ( #4151 ), #9231, .T. ) ;
#17000 = CARTESIAN_POINT ( 'NONE',  ( 51.80000000000003268, 3.850000000000017408, 1.627168804780626088 ) ) ;
#17002 = CARTESIAN_POINT ( 'NONE',  ( 48.45343659158886851, -1.329326705022595645, -3.861343257506216098 ) ) ;
#17001 = CARTESIAN_POINT ( 'NONE',  ( 48.33019736648184050, -1.141995257496313476, 3.938405479918980490 ) ) ;
#17004 = EDGE_CURVE ( 'NONE', #624, #26230, #8892, .T. ) ;
#17003 = CARTESIAN_POINT ( 'NONE',  ( 47.76318363328993399, -4.380055612571977619, 1.406160842577559800 ) ) ;
#17005 = ORIENTED_EDGE ( 'NONE', *, *, #12146, .F. ) ;
#17006 = CARTESIAN_POINT ( 'NONE',  ( 33.47623932017462778, -1.123735532908292978, -5.289358697221544503 ) ) ;
#17007 = ORIENTED_EDGE ( 'NONE', *, *, #11006, .F. ) ;
#17008 = DIRECTION ( 'NONE',  ( 0.000000000000000000, 0.2008964009354147484, -0.9796124928211138450 ) ) ;
#17009 = CARTESIAN_POINT ( 'NONE',  ( -56.94702994616206126, -2.078460969082657872, 3.599999999999789591 ) ) ;
#17010 = ORIENTED_EDGE ( 'NONE', *, *, #31299, .T. ) ;
#17011 = ORIENTED_EDGE ( 'NONE', *, *, #29980, .T. ) ;
#17012 = CIRCLE ( 'NONE', #18543, 1.250000000000000222 ) ;
#17013 = CARTESIAN_POINT ( 'NONE',  ( -59.60604010435355349, 3.187076279294280390, -1.184290838417780600 ) ) ;
#17014 = ORIENTED_EDGE ( 'NONE', *, *, #1526, .F. ) ;
#17015 = TOROIDAL_SURFACE ( 'NONE', #6873, 3.950000000000000178, 0.05000000000000000278 ) ;
#17016 = PLANE ( 'NONE',  #30327 ) ;
#17017 = CARTESIAN_POINT ( 'NONE',  ( -55.94702994616203995, -2.078460969082631227, -3.600000000000205258 ) ) ;
#17018 = ORIENTED_EDGE ( 'NONE', *, *, #14716, .F. ) ;
#17019 = CIRCLE ( 'NONE', #7393, 0.04999999999999988481 ) ;
#17020 = FACE_OUTER_BOUND ( 'NONE', #14491, .T. ) ;
#17021 = DIRECTION ( 'NONE',  ( 3.002035892788117459E-16, -0.9996898646859343485, -0.02490330187381123786 ) ) ;
#17022 = CIRCLE ( 'NONE', #3347, 0.4576450603546999840 ) ;
#17023 = LINE ( 'NONE', #2750, #5064 ) ;
#17024 = EDGE_LOOP ( 'NONE', ( #23176, #21154, #1595, #27742, #7860, #11657, #27859, #21916, #28801, #23206 ) ) ;
#17025 = CIRCLE ( 'NONE', #5887, 4.199999999999993072 ) ;
#17026 = DIRECTION ( 'NONE',  ( -0.9993908270190957621, 0.03489949670250097613, 3.491481338843133355E-15 ) ) ;
#17027 =( GEOMETRIC_REPRESENTATION_CONTEXT ( 3 ) GLOBAL_UNCERTAINTY_ASSIGNED_CONTEXT ( ( #3480 ) ) GLOBAL_UNIT_ASSIGNED_CONTEXT ( ( #21645, #14004, #16393 ) ) REPRESENTATION_CONTEXT ( 'NONE', 'WORKASPACE' ) );
#17028 = CARTESIAN_POINT ( 'NONE',  ( -54.49983703358571319, -1.542636180423125225, 4.059406436927349482 ) ) ;
#17029 = CARTESIAN_POINT ( 'NONE',  ( 49.05000000000002558, 1.401298464324817071E-42, -5.137714790107672405E-13 ) ) ;
#17030 = CARTESIAN_POINT ( 'NONE',  ( -44.49999999999997868, 6.542789527549899840E-15, -1.397091617737396343E-15 ) ) ;
#17031 = EDGE_CURVE ( 'NONE', #8224, #11926, #4975, .T. ) ;
#17032 = CARTESIAN_POINT ( 'NONE',  ( 57.05000000000001847, -0.7500000000000000000, 2.421260002560649660 ) ) ;
#17033 = ADVANCED_FACE ( 'NONE', ( #4473 ), #22056, .T. ) ;
#17034 = AXIS2_PLACEMENT_3D ( 'NONE', #16792, #11868, #300 ) ;
#17036 = DIRECTION ( 'NONE',  ( 0.000000000000000000, 1.000000000000000000, 0.000000000000000000 ) ) ;
#17035 = CARTESIAN_POINT ( 'NONE',  ( -36.11780688638208403, -4.018128186975085114, 3.618665893506928910 ) ) ;
#17037 = CIRCLE ( 'NONE', #29157, 0.05000000000000012768 ) ;
#17038 = AXIS2_PLACEMENT_3D ( 'NONE', #26450, #2697, #19196 ) ;
#17039 = CARTESIAN_POINT ( 'NONE',  ( 51.49777277048503521, 1.059151787769027298, 1.232523824083105346 ) ) ;
#17040 = CARTESIAN_POINT ( 'NONE',  ( 68.00000000000004263, 1.401298464324817071E-42, 2.624999999999286793 ) ) ;
#17042 = CARTESIAN_POINT ( 'NONE',  ( 53.94440344817343913, 6.524635634306410914, 1.761196874214440378 ) ) ;
#17041 = CIRCLE ( 'NONE', #21085, 3.500000000000000444 ) ;
#17043 = ORIENTED_EDGE ( 'NONE', *, *, #14412, .T. ) ;
#17044 = B_SPLINE_CURVE_WITH_KNOTS ( 'NONE', 3,
 ( #24268, #21908, #12226, #2721, #22212, #500, #22358, #190, #7632, #17438, #7483, #24557, #12363, #3033, #2878, #29457, #24720, #648, #26475 ),
 .UNSPECIFIED., .F., .F.,
 ( 4, 3, 3, 3, 3, 3, 4 ),
 ( -1.476948988848390564E-06, 2.117582368135750848E-22, 2.236146517042047793E-05, 4.055096472349869428E-05, 5.611001533034534733E-05, 7.070124744307527942E-05, 8.536389545014277545E-05 ),
 .UNSPECIFIED. ) ;
#17045 = VECTOR ( 'NONE', #29938, 1000.000000000000000 ) ;
#17046 = ORIENTED_EDGE ( 'NONE', *, *, #10176, .F. ) ;
#17047 = CARTESIAN_POINT ( 'NONE',  ( 51.87241998857975744, 0.05807428590527900780, -4.370869202345071258 ) ) ;
#17048 = VERTEX_POINT ( 'NONE', #18419 ) ;
#17049 = AXIS2_PLACEMENT_3D ( 'NONE', #9848, #29008, #17437 ) ;
#17050 = VECTOR ( 'NONE', #16559, 1000.000000000000000 ) ;
#17051 = CYLINDRICAL_SURFACE ( 'NONE', #21831, 0.09999999999999982514 ) ;
#17052 = CARTESIAN_POINT ( 'NONE',  ( -56.79792740578360366, -1.073804522883517132, -3.225979517392335794 ) ) ;
#17054 = CARTESIAN_POINT ( 'NONE',  ( -35.98994760229917489, 2.686240678228295042, 4.475885392924250361 ) ) ;
#17053 = FACE_OUTER_BOUND ( 'NONE', #18864, .T. ) ;
#17055 = EDGE_LOOP ( 'NONE', ( #18433, #21877 ) ) ;
#17056 = ORIENTED_EDGE ( 'NONE', *, *, #15083, .T. ) ;
#17057 = CARTESIAN_POINT ( 'NONE',  ( 22.79310476198749313, 6.591203646873187161, -2.050000000000079758 ) ) ;
#17058 = VERTEX_POINT ( 'NONE', #4622 ) ;
#17059 = CARTESIAN_POINT ( 'NONE',  ( -44.59999999999999432, 1.433333333333330906, 4.054078878802660491 ) ) ;
#17060 = ORIENTED_EDGE ( 'NONE', *, *, #18532, .F. ) ;
#17061 = DIRECTION ( 'NONE',  ( 0.000000000000000000, 1.000000000000000000, -8.673617379884030739E-15 ) ) ;
#17062 = ORIENTED_EDGE ( 'NONE', *, *, #11260, .F. ) ;
#17063 = DIRECTION ( 'NONE',  ( -0.8023336663629152543, -0.5470456816110889076, -0.2387503090077617296 ) ) ;
#17064 = CARTESIAN_POINT ( 'NONE',  ( -57.22499999999997300, 2.964020293532818446E-15, 1.549317489258312010E-18 ) ) ;
#17065 = AXIS2_PLACEMENT_3D ( 'NONE', #27955, #5254, #29629 ) ;
#17066 = LINE ( 'NONE', #2492, #7173 ) ;
#17067 = CARTESIAN_POINT ( 'NONE',  ( -60.38452994616202574, 2.093608279459374244E-14, -3.600000000000214140 ) ) ;
#17068 = CARTESIAN_POINT ( 'NONE',  ( 51.87416143049281914, 8.598705507415685290, -2.050000000000179678 ) ) ;
#17069 = EDGE_CURVE ( 'NONE', #29879, #24689, #14126, .T. ) ;
#17070 = EDGE_CURVE ( 'NONE', #28721, #3863, #12425, .T. ) ;
#17071 = AXIS2_PLACEMENT_3D ( 'NONE', #31236, #4775, #12082 ) ;
#17072 = EDGE_CURVE ( 'NONE', #7548, #560, #16488, .T. ) ;
#17074 = AXIS2_PLACEMENT_3D ( 'NONE', #30866, #19002, #28811 ) ;
#17073 = CARTESIAN_POINT ( 'NONE',  ( 27.27214205000343483, 5.011961650406415281, 1.549999999999904565 ) ) ;
#17075 = DIRECTION ( 'NONE',  ( 1.000000000000000000, 1.047444401652940007E-14, 0.000000000000000000 ) ) ;
#17076 = CYLINDRICAL_SURFACE ( 'NONE', #10423, 4.299999999999954525 ) ;
#17077 = DIRECTION ( 'NONE',  ( -1.000000000000000000, -0.000000000000000000, -0.000000000000000000 ) ) ;
#17078 = ORIENTED_EDGE ( 'NONE', *, *, #529, .T. ) ;
#17079 = CARTESIAN_POINT ( 'NONE',  ( 51.45655683570189609, 0.9591657938401617622, 1.196087371390568643 ) ) ;
#17080 = AXIS2_PLACEMENT_3D ( 'NONE', #2355, #26745, #28806 ) ;
#17082 = LINE ( 'NONE', #2506, #15113 ) ;
#17081 = CARTESIAN_POINT ( 'NONE',  ( -36.38139716712352367, -2.291889356120137222, -4.901871067649458347 ) ) ;
#17083 = CARTESIAN_POINT ( 'NONE',  ( 50.25000000000000000, 1.470078920827345925, 1.470078920828533420 ) ) ;
#17084 = EDGE_LOOP ( 'NONE', ( #24883, #10242, #8616, #13677 ) ) ;
#17085 = EDGE_CURVE ( 'NONE', #30343, #13205, #8733, .T. ) ;
#17086 = CARTESIAN_POINT ( 'NONE',  ( -36.72207054450174013, -4.892019442464210499, 2.306425897666011693 ) ) ;
#17087 = CIRCLE ( 'NONE', #11489, 0.09999999999999993616 ) ;
#17088 = ORIENTED_EDGE ( 'NONE', *, *, #21367, .T. ) ;
#17089 = DIRECTION ( 'NONE',  ( 0.000000000000000000, 1.000000000000000000, 0.000000000000000000 ) ) ;
#17091 = CARTESIAN_POINT ( 'NONE',  ( 48.00000000000001421, -3.908336260473453727, -1.238913909466087482 ) ) ;
#17090 = DIRECTION ( 'NONE',  ( 0.000000000000000000, 0.000000000000000000, 1.000000000000000000 ) ) ;
#17092 = ORIENTED_EDGE ( 'NONE', *, *, #21542, .T. ) ;
#17093 = DIRECTION ( 'NONE',  ( 0.000000000000000000, -1.000000000000000000, -3.491481338843132961E-15 ) ) ;
#17094 = AXIS2_PLACEMENT_3D ( 'NONE', #15931, #3911, #11188 ) ;
#17095 = DIRECTION ( 'NONE',  ( 7.401486830834382195E-15, 0.000000000000000000, 1.000000000000000000 ) ) ;
#17096 = AXIS2_PLACEMENT_3D ( 'NONE', #1513, #11171, #18469 ) ;
#17098 = CARTESIAN_POINT ( 'NONE',  ( 47.09453520915242564, 9.265918505097243241, -1.950000000000163380 ) ) ;
#17097 = CARTESIAN_POINT ( 'NONE',  ( 47.09104525948218622, 9.165979422395331255, 1.949999999999836087 ) ) ;
#17099 = ORIENTED_EDGE ( 'NONE', *, *, #27958, .T. ) ;
#17100 = CARTESIAN_POINT ( 'NONE',  ( -60.62499999999997158, 2.489203624310590168, -2.804704140674917134 ) ) ;
#17101 = CYLINDRICAL_SURFACE ( 'NONE', #14285, 4.000000000000000000 ) ;
#17102 = CARTESIAN_POINT ( 'NONE',  ( 15.03925126672132961, -1.123735532908273216, 5.289358697221548944 ) ) ;
#17103 = CARTESIAN_POINT ( 'NONE',  ( 15.90468948301723273, -2.602043737612640406, -4.741394629686820572 ) ) ;
#17104 = CARTESIAN_POINT ( 'NONE',  ( -54.49999999999999289, -1.466116979365514217, -3.192719761242667431 ) ) ;
#17105 = DIRECTION ( 'NONE',  ( 1.000000000000000000, 9.742518634817534591E-17, 4.338815227941629246E-17 ) ) ;
#17106 = CARTESIAN_POINT ( 'NONE',  ( -71.49999999999998579, -1.395601618875910821E-15, 2.917180974979867506E-15 ) ) ;
#17107 = CIRCLE ( 'NONE', #5899, 3.300781342844381072 ) ;
#17108 = ORIENTED_EDGE ( 'NONE', *, *, #25233, .T. ) ;
#17109 = CIRCLE ( 'NONE', #2454, 0.09999999999999997780 ) ;
#17110 = EDGE_CURVE ( 'NONE', #10205, #12232, #803, .T. ) ;
#17111 = VECTOR ( 'NONE', #7457, 1000.000000000000000 ) ;
#17112 = CARTESIAN_POINT ( 'NONE',  ( 61.16862972101651508, 0.7079877303047974468, -1.871978752395131895 ) ) ;
#17113 = CARTESIAN_POINT ( 'NONE',  ( 27.42782126191618630, 5.342778649435317995, -1.950000000000095213 ) ) ;
#17114 = DIRECTION ( 'NONE',  ( -1.344447539785323523E-44, 1.000000000000000000, 3.491481338843137300E-15 ) ) ;
#17115 = CARTESIAN_POINT ( 'NONE',  ( -59.44266919280509143, 3.352788690741696609, -1.089968598657499177 ) ) ;
#17116 = CARTESIAN_POINT ( 'NONE',  ( 54.19386703870442545, 5.671865141453449333, -1.950000000000188694 ) ) ;
#17118 = DIRECTION ( 'NONE',  ( 0.000000000000000000, 0.5454670984329667016, -0.8381322357045577487 ) ) ;
#17117 = CARTESIAN_POINT ( 'NONE',  ( 58.75000000000001421, 0.5380862305915415922, -2.008165151417984351 ) ) ;
#17119 = ORIENTED_EDGE ( 'NONE', *, *, #26122, .F. ) ;
#17120 = EDGE_CURVE ( 'NONE', #8353, #28219, #6373, .T. ) ;
#17121 = CARTESIAN_POINT ( 'NONE',  ( 58.65000000000001279, 0.8495817349404606311, -1.671477153794393766 ) ) ;
#17122 = ORIENTED_EDGE ( 'NONE', *, *, #935, .T. ) ;
#17123 = CARTESIAN_POINT ( 'NONE',  ( 60.88048385701370080, 0.6732112958821407922, 1.479676701994273369 ) ) ;
#17125 = DIRECTION ( 'NONE',  ( 0.000000000000000000, -0.2793919678926574668, -0.9601771338024398528 ) ) ;
#17124 = DIRECTION ( 'NONE',  ( 0.000000000000000000, -1.000000000000000000, 0.000000000000000000 ) ) ;
#17126 = CARTESIAN_POINT ( 'NONE',  ( 69.25000000000004263, -0.5000000000000000000, 1.988246715072632620 ) ) ;
#17127 = VERTEX_POINT ( 'NONE', #3998 ) ;
#17128 = ORIENTED_EDGE ( 'NONE', *, *, #3960, .F. ) ;
#17129 = DIRECTION ( 'NONE',  ( 0.000000000000000000, 0.000000000000000000, 1.000000000000000000 ) ) ;
#17130 = COLOUR_RGB ( '', 0.40784314, 0.44705882, 0.49803922) ;
#17131 =( BOUNDED_CURVE ( )  B_SPLINE_CURVE ( 3, ( #3293, #29889, #18612, #22629 ),
 .UNSPECIFIED., .F., .T. ) 
 B_SPLINE_CURVE_WITH_KNOTS ( ( 4, 4 ),
 ( 4.050220903230332681, 4.465400561421049019 ),
 .UNSPECIFIED. ) 
 CURVE ( )  GEOMETRIC_REPRESENTATION_ITEM ( )  RATIONAL_B_SPLINE_CURVE ( ( 1.000000000000000000, 0.9856869983806462177, 0.9856869983806462177, 1.000000000000000000 ) ) 
 REPRESENTATION_ITEM ( '' )  );
#17132 = ORIENTED_EDGE ( 'NONE', *, *, #20695, .T. ) ;
#17133 = CARTESIAN_POINT ( 'NONE',  ( 61.25000000000001421, 0.5000000000006414869, -1.807104036850122109 ) ) ;
#17134 = CARTESIAN_POINT ( 'NONE',  ( -54.61042740578360366, -2.936324665650200672, -2.606018187048499080 ) ) ;
#17135 = ORIENTED_EDGE ( 'NONE', *, *, #11497, .F. ) ;
#17136 = CARTESIAN_POINT ( 'NONE',  ( -36.31414349454748702, -4.963067629822554672, -1.552801941062300628 ) ) ;
#17137 = ORIENTED_EDGE ( 'NONE', *, *, #25663, .F. ) ;
#17138 = CARTESIAN_POINT ( 'NONE',  ( 58.65000038048067665, -1.383507098107042088, -1.265626441015408998 ) ) ;
#17139 = ORIENTED_EDGE ( 'NONE', *, *, #16190, .F. ) ;
#17140 = ORIENTED_EDGE ( 'NONE', *, *, #30353, .F. ) ;
#17141 = EDGE_CURVE ( 'NONE', #1976, #7542, #31144, .T. ) ;
#17142 = CARTESIAN_POINT ( 'NONE',  ( -59.75952994616203284, -3.117691453623963938, -1.800000000000223199 ) ) ;
#17143 = DIRECTION ( 'NONE',  ( 0.000000000000000000, 0.2008964009354141933, -0.9796124928211140670 ) ) ;
#17144 = CARTESIAN_POINT ( 'NONE',  ( 48.00000000000002132, -3.936726248589973221, 1.145507068359725933 ) ) ;
#17145 = CARTESIAN_POINT ( 'NONE',  ( -57.22499999999997300, 2.964020293532818446E-15, 1.549317489258312010E-18 ) ) ;
#17146 = CARTESIAN_POINT ( 'NONE',  ( -67.36397038208805554, -4.395200732636863594E-16, 3.272898199462452353E-15 ) ) ;
#17147 = CIRCLE ( 'NONE', #19679, 0.04999999999999989175 ) ;
#17149 = FACE_OUTER_BOUND ( 'NONE', #27903, .T. ) ;
#17148 = CARTESIAN_POINT ( 'NONE',  ( 54.19030381964616083, 6.697848500921247172, -2.050000000000189004 ) ) ;
#17150 = CARTESIAN_POINT ( 'NONE',  ( 51.98855675296391610, 0.7791495708613139781, 1.432971607104406520 ) ) ;
#17151 = DIRECTION ( 'NONE',  ( 1.000000000000000000, -0.000000000000000000, -1.047444401652940007E-14 ) ) ;
#17153 = CARTESIAN_POINT ( 'NONE',  ( -73.89999999999997726, 1.349581317326009389, 0.03361945752964979467 ) ) ;
#17152 = CARTESIAN_POINT ( 'NONE',  ( 16.07512358269905661, 5.037778396015567317, -1.970103387723833865 ) ) ;
#17154 = ORIENTED_EDGE ( 'NONE', *, *, #18349, .F. ) ;
#17155 = EDGE_CURVE ( 'NONE', #26979, #21323, #23558, .T. ) ;
#17156 = CARTESIAN_POINT ( 'NONE',  ( 58.65000000000003411, -1.278133834460056795, -1.372267738820685423 ) ) ;
#17157 = CARTESIAN_POINT ( 'NONE',  ( 47.86735231835938009, -4.319730106884873244, -1.256953381662404334 ) ) ;
#17159 = PLANE ( 'NONE',  #29780 ) ;
#17158 = CARTESIAN_POINT ( 'NONE',  ( 33.47623932017462778, 4.683225679163371957, -2.703237727951181668 ) ) ;
#17160 = CARTESIAN_POINT ( 'NONE',  ( -58.06249999999996447, 3.400000000000007905, -1.844164440896605116E-13 ) ) ;
#17161 = ORIENTED_EDGE ( 'NONE', *, *, #11359, .T. ) ;
#17162 = PLANE ( 'NONE',  #11949 ) ;
#17163 = ORIENTED_EDGE ( 'NONE', *, *, #27008, .F. ) ;
#17164 = DIRECTION ( 'NONE',  ( 0.000000000000000000, 1.000000000000000000, 3.491481338843130594E-15 ) ) ;
#17165 = ORIENTED_EDGE ( 'NONE', *, *, #15982, .T. ) ;
#17166 = ADVANCED_FACE ( 'NONE', ( #12359 ), #5343, .T. ) ;
#17167 = ORIENTED_EDGE ( 'NONE', *, *, #21805, .T. ) ;
#17168 = CARTESIAN_POINT ( 'NONE',  ( 15.22842924604220016, 5.340403874105067672, 0.9205822089998703106 ) ) ;
#17169 = PRODUCT_DEFINITION_FORMATION_WITH_SPECIFIED_SOURCE ( 'ANY', '', #16191, .NOT_KNOWN. ) ;
#17170 = ORIENTED_EDGE ( 'NONE', *, *, #27843, .T. ) ;
#17171 = DIRECTION ( 'NONE',  ( -1.000000000000000000, 1.219044193948983948E-29, -3.491481338843133355E-15 ) ) ;
#17172 = TOROIDAL_SURFACE ( 'NONE', #18195, 3.950000000000000178, 0.05000000000000000278 ) ;
#17173 = CARTESIAN_POINT ( 'NONE',  ( -57.38452994616203284, 2.093608279459370457E-14, -3.600000000000203926 ) ) ;
#17174 = ORIENTED_EDGE ( 'NONE', *, *, #14323, .T. ) ;
#17175 = DIRECTION ( 'NONE',  ( 0.000000000000000000, -1.000000000000000000, 0.000000000000000000 ) ) ;
#17176 = LINE ( 'NONE', #7347, #8121 ) ;
#17177 = CARTESIAN_POINT ( 'NONE',  ( 31.77414890219473165, 7.582826004857921909, 1.949999999999889377 ) ) ;
#17178 = ORIENTED_EDGE ( 'NONE', *, *, #12134, .T. ) ;
#17179 = EDGE_CURVE ( 'NONE', #16493, #11263, #25571, .T. ) ;
#17180 = CARTESIAN_POINT ( 'NONE',  ( 51.74297196358455153, -4.175266387598156825, -1.009028806847065196 ) ) ;
#17181 = EDGE_CURVE ( 'NONE', #28219, #19112, #20540, .T. ) ;
#17182 = CARTESIAN_POINT ( 'NONE',  ( 51.87770073550463223, 8.700057942179277859, -2.050000000000180123 ) ) ;
#17183 = CARTESIAN_POINT ( 'NONE',  ( 58.75000018595671492, -1.011330950598887224, -1.651828233788867450 ) ) ;
#17185 = EDGE_CURVE ( 'NONE', #11967, #17261, #11410, .T. ) ;
#17184 = CARTESIAN_POINT ( 'NONE',  ( -60.49999999999997868, -2.624185894800576957, -0.06537116741875233228 ) ) ;
#17186 = DIRECTION ( 'NONE',  ( 1.282749433769087582E-30, 1.000000000000000000, 1.224646799147353207E-16 ) ) ;
#17187 = VECTOR ( 'NONE', #11774, 1000.000000000000000 ) ;
#17188 = CARTESIAN_POINT ( 'NONE',  ( 58.74154451056424620, -1.017012227664021662, 1.575232816092780652 ) ) ;
#17189 = CARTESIAN_POINT ( 'NONE',  ( -59.66878239164782372, 3.173439364805089813, -1.220515114876693064 ) ) ;
#17190 = PLANE ( 'NONE',  #6901 ) ;
#17191 = AXIS2_PLACEMENT_3D ( 'NONE', #16296, #6955, #23892 ) ;
#17192 = CARTESIAN_POINT ( 'NONE',  ( 61.25000000000003553, -0.9885922787754447549, -1.658880815145630239 ) ) ;
#17193 = ORIENTED_EDGE ( 'NONE', *, *, #2038, .F. ) ;
#17194 = CONICAL_SURFACE ( 'NONE', #4025, 1.875000000000001776, 0.7853981633974510546 ) ;
#17195 = VERTEX_POINT ( 'NONE', #24264 ) ;
#17196 = EDGE_LOOP ( 'NONE', ( #20743, #16641, #1332, #10602, #18559, #22272 ) ) ;
#17197 = DIRECTION ( 'NONE',  ( 1.000000000000000000, 0.000000000000000000, 0.000000000000000000 ) ) ;
#17198 = CARTESIAN_POINT ( 'NONE',  ( -55.73542740578360366, 2.936324665650206889, 2.606018187048498191 ) ) ;
#17200 = FACE_OUTER_BOUND ( 'NONE', #12370, .T. ) ;
#17199 = DIRECTION ( 'NONE',  ( 1.000000000000000000, 3.054025858079668409E-16, -2.042474015755241579E-16 ) ) ;
#17201 = VERTEX_POINT ( 'NONE', #495 ) ;
#17202 = EDGE_CURVE ( 'NONE', #13278, #27612, #12221, .T. ) ;
#17203 = ORIENTED_EDGE ( 'NONE', *, *, #30353, .T. ) ;
#17204 = CARTESIAN_POINT ( 'NONE',  ( -55.97085481156723574, -3.673546848079175309, -0.7533615035078069511 ) ) ;
#17205 = ORIENTED_EDGE ( 'NONE', *, *, #182, .F. ) ;
#17206 = DIRECTION ( 'NONE',  ( 3.384826294588897856E-15, 0.000000000000000000, 1.000000000000000000 ) ) ;
#17207 = ORIENTED_EDGE ( 'NONE', *, *, #25272, .T. ) ;
#17208 = CARTESIAN_POINT ( 'NONE',  ( 27.84544208433268153, 5.444976785341570924, -2.050000000000357314 ) ) ;
#17209 = ADVANCED_FACE ( 'NONE', ( #17286 ), #24104, .T. ) ;
#17210 = ORIENTED_EDGE ( 'NONE', *, *, #15436, .F. ) ;
#17211 = CARTESIAN_POINT ( 'NONE',  ( 51.23644008536124517, -1.080112125195908046, 1.214076932077873039 ) ) ;
#17212 = CYLINDRICAL_SURFACE ( 'NONE', #10726, 3.750000000000000444 ) ;
#17213 = CARTESIAN_POINT ( 'NONE',  ( 47.10000000000002274, 6.982261990806648555E-14, -1.632474749424821370E-13 ) ) ;
#17214 = AXIS2_PLACEMENT_3D ( 'NONE', #18452, #15899, #12109 ) ;
#17215 = CARTESIAN_POINT ( 'NONE',  ( -55.26905989232413674, -2.944486372867088697, 1.699999999999792344 ) ) ;
#17217 = ADVANCED_FACE ( 'NONE', ( #7768 ), #11906, .T. ) ;
#17216 = CARTESIAN_POINT ( 'NONE',  ( 51.39453088482484588, 4.389042235173731044, -2.050000000000179234 ) ) ;
#17218 = CIRCLE ( 'NONE', #11138, 3.200000000000000178 ) ;
#17219 = DIRECTION ( 'NONE',  ( 0.5633368246415177971, -0.8262273428075421755, 0.000000000000000000 ) ) ;
#17220 = CARTESIAN_POINT ( 'NONE',  ( 50.37823977475586190, 1.183413901109590105, -3.885761703493072261 ) ) ;
#17221 = CARTESIAN_POINT ( 'NONE',  ( 15.32752150720754258, -5.374748457514303190, -0.5963382560600449800 ) ) ;
#17222 = DIRECTION ( 'NONE',  ( 1.000000000000000000, 1.047444401652940007E-14, -0.000000000000000000 ) ) ;
#17223 = ORIENTED_EDGE ( 'NONE', *, *, #18029, .T. ) ;
#17224 = DIRECTION ( 'NONE',  ( 1.000000000000000000, 1.047444401652940007E-14, 0.000000000000000000 ) ) ;
#17225 = CARTESIAN_POINT ( 'NONE',  ( 51.44193764627956256, -0.9752197701239264660, -1.304631266258929889 ) ) ;
#17226 = CARTESIAN_POINT ( 'NONE',  ( 53.94287869493206244, 6.382073928939168361, 1.484311102127795490 ) ) ;
#17227 = VERTEX_POINT ( 'NONE', #12077 ) ;
#17228 = CYLINDRICAL_SURFACE ( 'NONE', #30006, 3.750000000000000444 ) ;
#17229 = VERTEX_POINT ( 'NONE', #17432 ) ;
#17230 = CYLINDRICAL_SURFACE ( 'NONE', #11709, 3.399999999999999911 ) ;
#17231 = CYLINDRICAL_SURFACE ( 'NONE', #1154, 0.2500000000000000000 ) ;
#17233 = CARTESIAN_POINT ( 'NONE',  ( -61.58548216437489486, -2.595212895210543991, -0.5020542520759796457 ) ) ;
#17232 = CARTESIAN_POINT ( 'NONE',  ( -59.29999999999997584, -0.6177564328763985868, 3.012308415424926444 ) ) ;
#17234 = ORIENTED_EDGE ( 'NONE', *, *, #10790, .T. ) ;
#17235 = ADVANCED_FACE ( 'NONE', ( #27082 ), #17015, .T. ) ;
#17236 = DIRECTION ( 'NONE',  ( 0.000000000000000000, 0.000000000000000000, -1.000000000000000000 ) ) ;
#17237 = TOROIDAL_SURFACE ( 'NONE', #29856, 4.349999999999997868, 0.05000000000000000278 ) ;
#17238 = EDGE_CURVE ( 'NONE', #26219, #20971, #2329, .T. ) ;
#17239 = DIRECTION ( 'NONE',  ( 0.000000000000000000, -0.9875000000000001554, -0.1576190026614806561 ) ) ;
#17241 = CARTESIAN_POINT ( 'NONE',  ( -54.45981523601835761, -1.500740478982482973, -4.030402907299741599 ) ) ;
#17240 = CARTESIAN_POINT ( 'NONE',  ( 52.42875048912549119, 4.000253242763575301, 2.045760939463020733 ) ) ;
#17242 = EDGE_CURVE ( 'NONE', #29758, #30573, #1820, .T. ) ;
#17243 = ORIENTED_EDGE ( 'NONE', *, *, #8482, .T. ) ;
#17244 = CARTESIAN_POINT ( 'NONE',  ( -59.24999999999997158, -1.184343223768586029, -3.558065644182723197 ) ) ;
#17245 = DIRECTION ( 'NONE',  ( 1.000000000000000000, 1.047444401652940007E-14, 0.000000000000000000 ) ) ;
#17246 = CARTESIAN_POINT ( 'NONE',  ( -55.81249999999997868, 3.400000000000007905, -1.865662262041272555E-13 ) ) ;
#17247 = DIRECTION ( 'NONE',  ( -1.000000000000000000, 0.000000000000000000, 1.047444401652940007E-14 ) ) ;
#17248 = DIRECTION ( 'NONE',  ( 2.468478480535042241E-12, -0.05332224631830475431, -0.9985773570673281974 ) ) ;
#17249 = DIRECTION ( 'NONE',  ( 0.000000000000000000, 0.000000000000000000, -1.000000000000000000 ) ) ;
#17250 = VERTEX_POINT ( 'NONE', #2416 ) ;
#17251 = ADVANCED_FACE ( 'NONE', ( #21754 ), #3832, .T. ) ;
#17252 = CARTESIAN_POINT ( 'NONE',  ( 58.65000000000001990, 6.143261415694495821E-13, 3.111507638930570854E-58 ) ) ;
#17253 = CARTESIAN_POINT ( 'NONE',  ( 23.81491379129848696, 5.755424080683373411, -1.950000000000082556 ) ) ;
#17254 = DIRECTION ( 'NONE',  ( 0.000000000000000000, 0.000000000000000000, -1.000000000000000000 ) ) ;
#17255 = LINE ( 'NONE', #24067, #17994 ) ;
#17256 = CARTESIAN_POINT ( 'NONE',  ( 61.24919886530821600, -0.9685650917400145943, 1.667277206152059987 ) ) ;
#17258 = CARTESIAN_POINT ( 'NONE',  ( 24.79176202108332205, 5.385922622694288897, 1.424999999999913669 ) ) ;
#17257 = DIRECTION ( 'NONE',  ( -2.614375865348240525E-16, 0.2008964009354147762, -0.9796124928211140670 ) ) ;
#17259 = ORIENTED_EDGE ( 'NONE', *, *, #29386, .F. ) ;
#17260 = CARTESIAN_POINT ( 'NONE',  ( 58.74999981196287280, -1.909245389981207408, 0.4235863532959572852 ) ) ;
#17261 = VERTEX_POINT ( 'NONE', #4941 ) ;
#17262 = DIRECTION ( 'NONE',  ( 1.000000000000000000, 1.047444401652940007E-14, 0.000000000000000000 ) ) ;
#17264 = CARTESIAN_POINT ( 'NONE',  ( 58.69321565534372809, -0.4999999999993854916, -1.812725888577163103 ) ) ;
#17263 = CARTESIAN_POINT ( 'NONE',  ( 57.00875904852982501, 0.7282698412063691729, -2.435189460583063514 ) ) ;
#17265 = CARTESIAN_POINT ( 'NONE',  ( 58.50000000000001421, -0.8000000000000000444, 2.421260002560649660 ) ) ;
#17266 = ORIENTED_EDGE ( 'NONE', *, *, #11136, .F. ) ;
#17267 = ORIENTED_EDGE ( 'NONE', *, *, #20718, .T. ) ;
#17268 = CARTESIAN_POINT ( 'NONE',  ( 51.98855675296393031, -0.7791495708602242942, -1.432971607104406297 ) ) ;
#17269 = ADVANCED_FACE ( 'NONE', ( #10768 ), #15534, .T. ) ;
#17270 = B_SPLINE_CURVE_WITH_KNOTS ( 'NONE', 3,
 ( #22146, #10096, #19766, #22299, #17538, #29397, #7859, #7709, #14987, #24654 ),
 .UNSPECIFIED., .F., .F.,
 ( 4, 2, 2, 2, 4 ),
 ( 0.000000000000000000, 0.0004363777631660865864, 0.0006545666447491310181, 0.0007636610855406569202, 0.0008727555263321828223 ),
 .UNSPECIFIED. ) ;
#17271 = VECTOR ( 'NONE', #1219, 1000.000000000000000 ) ;
#17272 = DIRECTION ( 'NONE',  ( -1.000000000000000000, -3.053848253006669023E-16, 2.042510438544995415E-16 ) ) ;
#17273 = ORIENTED_EDGE ( 'NONE', *, *, #2549, .F. ) ;
#17274 = CARTESIAN_POINT ( 'NONE',  ( 57.00000000000001421, -0.7256347085964565125, -1.800308733460772359 ) ) ;
#17275 = CARTESIAN_POINT ( 'NONE',  ( -55.29792740578360366, -1.073804522883516688, -3.225979517392336238 ) ) ;
#17276 = LINE ( 'NONE', #17422, #8136 ) ;
#17277 = ORIENTED_EDGE ( 'NONE', *, *, #7380, .F. ) ;
#17278 = CARTESIAN_POINT ( 'NONE',  ( 0.000000000000000000, 0.000000000000000000, 0.000000000000000000 ) ) ;
#17279 = CARTESIAN_POINT ( 'NONE',  ( 58.65266784251151222, -1.277991457600138991, -1.372094080476043310 ) ) ;
#17280 = ORIENTED_EDGE ( 'NONE', *, *, #29471, .F. ) ;
#17281 = ADVANCED_FACE ( 'NONE', ( #29776 ), #6572, .T. ) ;
#17282 = CIRCLE ( 'NONE', #17792, 0.2500000000000000000 ) ;
#17283 = CARTESIAN_POINT ( 'NONE',  ( -58.75952994616203284, 3.117691453623994580, -1.800000000000195000 ) ) ;
#17284 = CARTESIAN_POINT ( 'NONE',  ( 52.10591853744707436, 8.701414215152928122, -2.050000000000181455 ) ) ;
#17285 = CARTESIAN_POINT ( 'NONE',  ( 48.41523095594689607, -1.115727354199206323, -3.895947837398489266 ) ) ;
#17286 = FACE_OUTER_BOUND ( 'NONE', #27335, .T. ) ;
#17287 = CARTESIAN_POINT ( 'NONE',  ( 51.75297847264299378, -4.174452932061539556, -1.011256013762273920 ) ) ;
#17288 = CARTESIAN_POINT ( 'NONE',  ( 58.66107449606936086, -1.819875603893454485, 0.4525291603558602715 ) ) ;
#17289 = CIRCLE ( 'NONE', #15270, 0.2499999999999997780 ) ;
#17291 = CARTESIAN_POINT ( 'NONE',  ( -36.22818246778668083, -0.6967302926296108367, -5.374298406428810182 ) ) ;
#17290 = CARTESIAN_POINT ( 'NONE',  ( -59.69999999999998153, -3.031840806488110385, 1.538811659727342906 ) ) ;
#17292 = CARTESIAN_POINT ( 'NONE',  ( 58.65000000000001990, 6.143261415694495821E-13, 3.111507638930570854E-58 ) ) ;
#17293 = DIRECTION ( 'NONE',  ( 0.000000000000000000, -1.000000000000000000, -2.168404344971007685E-15 ) ) ;
#17295 = CARTESIAN_POINT ( 'NONE',  ( -62.09999999999997300, -2.634806471255679572, -0.2806920565413739133 ) ) ;
#17294 = CARTESIAN_POINT ( 'NONE',  ( 15.30042582489633318, 4.683225673666406408, -2.703237737474395441 ) ) ;
#17296 = VERTEX_POINT ( 'NONE', #20451 ) ;
#17297 =( BOUNDED_SURFACE ( )  B_SPLINE_SURFACE ( 3, 2, ( 
 ( #14525, #21210, #23728 ),
 ( #1687, #11350, #21038 ),
 ( #18662, #28311, #6618 ),
 ( #4228, #120, #7699 ),
 ( #17220, #12602, #19609 ),
 ( #424, #19440, #12152 ),
 ( #21830, #24645, #27004 ),
 ( #14975, #5641, #12287 ),
 ( #24477, #2498, #17357 ),
 ( #5167, #29388, #22431 ) ),
 .UNSPECIFIED., .F., .F., .T. ) 
 B_SPLINE_SURFACE_WITH_KNOTS ( ( 4, 2, 2, 2, 4 ),
 ( 3, 3 ),
 ( 0.0004005301535625022482, 0.0008279283193725973976, 0.001041627402277645054, 0.001148476943730168936, 0.001255326485182692601 ),
 ( 0.000000000000000000, 1.000000000000000000 ),
 .UNSPECIFIED. ) 
 GEOMETRIC_REPRESENTATION_ITEM ( )  RATIONAL_B_SPLINE_SURFACE ( (
 ( 1.000000000000000000, 0.7071067811865505703, 1.000000000000000000),
 ( 1.000000000000000000, 0.7463463187144504518, 1.000000000000000000),
 ( 1.000000000000000000, 0.7946150999565705364, 1.000000000000000000),
 ( 1.000000000000000000, 0.8720431506958310486, 1.000000000000000000),
 ( 1.000000000000000000, 0.8987780092778684393, 1.000000000000000000),
 ( 1.000000000000000000, 0.9375340664365204857, 1.000000000000000000),
 ( 1.000000000000000000, 0.9504270566176310497, 1.000000000000000000),
 ( 1.000000000000000000, 0.9732249474031181569, 1.000000000000000000),
 ( 1.000000000000000000, 0.9839441327696822892, 1.000000000000000000),
 ( 1.000000000000000000, 0.9842509842514762797, 1.000000000000000000) ) ) 
 REPRESENTATION_ITEM ( '' )  SURFACE ( )  );
#17298 = LINE ( 'NONE', #29015, #11910 ) ;
#17299 = DIRECTION ( 'NONE',  ( 1.000000000000000000, 1.047444401652940007E-14, 0.000000000000000000 ) ) ;
#17301 = DIRECTION ( 'NONE',  ( -0.9993908270190956511, 0.03489949670250096919, 3.491481338843132961E-15 ) ) ;
#17300 = CARTESIAN_POINT ( 'NONE',  ( 15.41080140630239192, 3.722599991951259124, -3.938370952810016590 ) ) ;
#17302 = CARTESIAN_POINT ( 'NONE',  ( 47.73687070013482270, -4.312041630646834989, 1.282098934412685187 ) ) ;
#17303 = EDGE_LOOP ( 'NONE', ( #6342, #13781, #30337, #13588 ) ) ;
#17304 = DIRECTION ( 'NONE',  ( -1.000000000000000000, 0.000000000000000000, 3.491481338843133355E-15 ) ) ;
#17305 = ADVANCED_FACE ( 'NONE', ( #8393 ), #22503, .T. ) ;
#17306 = ORIENTED_EDGE ( 'NONE', *, *, #30119, .F. ) ;
#17307 = ADVANCED_FACE ( 'NONE', ( #20150 ), #16465, .F. ) ;
#17308 = DIRECTION ( 'NONE',  ( 2.586136946169074517E-16, -1.000000000000000000, 0.000000000000000000 ) ) ;
#17309 = EDGE_LOOP ( 'NONE', ( #31203, #6555 ) ) ;
#17310 = ORIENTED_EDGE ( 'NONE', *, *, #3638, .T. ) ;
#17311 = CARTESIAN_POINT ( 'NONE',  ( 58.65817410504309493, -0.5270377936596636337, -1.799623063671780487 ) ) ;
#17312 = ORIENTED_EDGE ( 'NONE', *, *, #28787, .F. ) ;
#17313 = CARTESIAN_POINT ( 'NONE',  ( 51.41939584733315627, 0.9814691331449714173, -1.432192464238639884 ) ) ;
#17314 = CARTESIAN_POINT ( 'NONE',  ( -55.01905989232411542, 2.023778652682504950E-14, -3.400000000000195310 ) ) ;
#17315 = ORIENTED_EDGE ( 'NONE', *, *, #9699, .F. ) ;
#17316 = DIRECTION ( 'NONE',  ( 0.000000000000000000, -0.9996898646859344595, -0.02490330187381124480 ) ) ;
#17317 = CARTESIAN_POINT ( 'NONE',  ( 63.50000000000000000, 0.8382352941176473005, -2.222158093317947003 ) ) ;
#17318 = CARTESIAN_POINT ( 'NONE',  ( 23.38809389355778023, 6.107120497888718802, 2.049999999999917222 ) ) ;
#17319 = ORIENTED_EDGE ( 'NONE', *, *, #26681, .F. ) ;
#17320 = EDGE_CURVE ( 'NONE', #20124, #10732, #23060, .T. ) ;
#17321 = CARTESIAN_POINT ( 'NONE',  ( 68.00000000000000000, 0.6617647058823536987, -1.754335336830146641 ) ) ;
#17322 = CARTESIAN_POINT ( 'NONE',  ( -54.47328085509070661, -1.505517457405397996, 4.033720452520547894 ) ) ;
#17323 = CARTESIAN_POINT ( 'NONE',  ( 58.75000000000003553, -0.8495817349395312634, -1.671477153794241888 ) ) ;
#17324 = CARTESIAN_POINT ( 'NONE',  ( 58.50000000000001421, 0.000000000000000000, 0.000000000000000000 ) ) ;
#17325 = DIRECTION ( 'NONE',  ( -1.404304041445553711E-15, -0.9030524935654961061, 0.4295302013422803711 ) ) ;
#17327 = PLANE ( 'NONE',  #2773 ) ;
#17326 = CARTESIAN_POINT ( 'NONE',  ( -36.31414349454756518, -3.010474646410484123, 4.240315621469648910 ) ) ;
#17328 = EDGE_CURVE ( 'NONE', #10580, #6314, #9412, .T. ) ;
#17329 = DIRECTION ( 'NONE',  ( -1.000000000000000000, 1.219044193948983948E-29, -3.491481338843133355E-15 ) ) ;
#17330 = CARTESIAN_POINT ( 'NONE',  ( 58.66107449606985114, 1.874988011599642235, 0.03390886286986791870 ) ) ;
#17331 = DIRECTION ( 'NONE',  ( 0.000000000000000000, 0.9996898646859344595, 0.02490330187381124133 ) ) ;
#17332 = ORIENTED_EDGE ( 'NONE', *, *, #13887, .F. ) ;
#17333 = EDGE_LOOP ( 'NONE', ( #25986, #5740, #1316, #19147 ) ) ;
#17334 = EDGE_CURVE ( 'NONE', #22781, #11615, #3342, .T. ) ;
#17335 = VERTEX_POINT ( 'NONE', #6333 ) ;
#17336 = EDGE_CURVE ( 'NONE', #28086, #355, #13416, .T. ) ;
#17337 = CARTESIAN_POINT ( 'NONE',  ( -59.13147575765562181, 2.328089616296125985, 1.276504352643064388 ) ) ;
#17338 = AXIS2_PLACEMENT_3D ( 'NONE', #16368, #22882, #18605 ) ;
#17339 = CARTESIAN_POINT ( 'NONE',  ( -60.36042740578359656, 3.725040285533370632, -1.239922660687674982 ) ) ;
#17341 = DIRECTION ( 'NONE',  ( 0.03489949670250203084, 0.9993908270190957621, -3.673133589935336920E-30 ) ) ;
#17340 = CARTESIAN_POINT ( 'NONE',  ( 47.00000000000002132, 1.734723475976807094E-15, 0.000000000000000000 ) ) ;
#17342 = ADVANCED_FACE ( 'NONE', ( #18857 ), #31024, .F. ) ;
#17343 = ORIENTED_EDGE ( 'NONE', *, *, #7894, .F. ) ;
#17344 = EDGE_LOOP ( 'NONE', ( #9104, #14211, #8995, #22576 ) ) ;
#17345 = CARTESIAN_POINT ( 'NONE',  ( 54.02156746059516479, 6.375683097465850935, -1.975347834873397490 ) ) ;
#17346 = ORIENTED_EDGE ( 'NONE', *, *, #27872, .F. ) ;
#17347 = CARTESIAN_POINT ( 'NONE',  ( -71.44999999999998863, 0.4218824419643697476, -2.057186234924337054 ) ) ;
#17348 = EDGE_LOOP ( 'NONE', ( #23942, #19882, #25546, #29842 ) ) ;
#17349 = CARTESIAN_POINT ( 'NONE',  ( 30.23587923389752419, 6.713699166094404092, -1.950000000000105871 ) ) ;
#17350 = CARTESIAN_POINT ( 'NONE',  ( -58.40400635094607651, 1.737685414808531892, -3.471684241605561549 ) ) ;
#17351 = DIRECTION ( 'NONE',  ( -1.000000000000000000, 1.219044193948983948E-29, -3.491481338843133355E-15 ) ) ;
#17352 = EDGE_CURVE ( 'NONE', #5493, #20519, #21560, .T. ) ;
#17353 = CARTESIAN_POINT ( 'NONE',  ( 15.22842924604237780, -5.340403874104624471, -0.9205822090001011260 ) ) ;
#17354 = CARTESIAN_POINT ( 'NONE',  ( -60.19702994616203995, 4.156921938165313080, -1.985113767892243204E-13 ) ) ;
#17355 = CARTESIAN_POINT ( 'NONE',  ( 51.68129744678915927, 4.333300462208747206, -1.550000000000180123 ) ) ;
#17356 = CARTESIAN_POINT ( 'NONE',  ( 50.50000000000002132, 2.428612866367529932E-14, 0.000000000000000000 ) ) ;
#17357 = CARTESIAN_POINT ( 'NONE',  ( 50.33755732750839940, 1.426738769040801769, -3.843750315111145621 ) ) ;
#17358 = AXIS2_PLACEMENT_3D ( 'NONE', #17368, #5652, #19913 ) ;
#17359 = ADVANCED_FACE ( 'NONE', ( #8695 ), #17996, .T. ) ;
#17360 = CARTESIAN_POINT ( 'NONE',  ( 16.08093158123430655, -5.047763082740431173, -1.943828653492548630 ) ) ;
#17362 = ADVANCED_FACE ( 'NONE', ( #26121 ), #25649, .T. ) ;
#17361 = CARTESIAN_POINT ( 'NONE',  ( -62.39999999999998437, 1.076401154667962023E-15, 2.259002067258145746E-15 ) ) ;
#17363 = ORIENTED_EDGE ( 'NONE', *, *, #10907, .T. ) ;
#17364 = CARTESIAN_POINT ( 'NONE',  ( -59.29999999999998295, -2.024706599330198031, 2.760581573505366926 ) ) ;
#17365 = DIRECTION ( 'NONE',  ( 0.000000000000000000, 1.000000000000000000, 1.532429380227459806E-15 ) ) ;
#17366 = CARTESIAN_POINT ( 'NONE',  ( 54.20407287615058323, 5.668441115105648187, 2.049999999999810196 ) ) ;
#17367 = VERTEX_POINT ( 'NONE', #9347 ) ;
#17368 = CARTESIAN_POINT ( 'NONE',  ( -39.16187796471576377, -1.705048840508494473E-14, 0.000000000000000000 ) ) ;
#17369 = VERTEX_POINT ( 'NONE', #30392 ) ;
#17370 = EDGE_CURVE ( 'NONE', #14055, #26583, #23291, .T. ) ;
#17371 = DIRECTION ( 'NONE',  ( -1.000000000000000000, -0.000000000000000000, -0.000000000000000000 ) ) ;
#17372 = CARTESIAN_POINT ( 'NONE',  ( 58.45000000000001705, 0.7500000000000000000, -1.778341924377873751 ) ) ;
#17374 = CARTESIAN_POINT ( 'NONE',  ( 47.09999999999999432, -3.609867133138429995, -1.947518732153282306 ) ) ;
#17373 = PLANE ( 'NONE',  #22126 ) ;
#17375 = ADVANCED_FACE ( 'NONE', ( #23138 ), #1426, .T. ) ;
#17376 = ORIENTED_EDGE ( 'NONE', *, *, #25693, .T. ) ;
#17377 = DIRECTION ( 'NONE',  ( -1.047444401652940007E-14, 0.000000000000000000, -1.000000000000000000 ) ) ;
#17378 = CARTESIAN_POINT ( 'NONE',  ( 56.95000000000001705, 0.000000000000000000, 2.549999999999999822 ) ) ;
#17379 = ORIENTED_EDGE ( 'NONE', *, *, #16091, .T. ) ;
#17381 = CARTESIAN_POINT ( 'NONE',  ( -59.09999999999997300, 8.366749974758448157E-15, -2.099585467500611340E-13 ) ) ;
#17380 = CARTESIAN_POINT ( 'NONE',  ( -58.01905989232410832, 3.648081215184778998E-14, -3.400000000000205969 ) ) ;
#17382 = DIRECTION ( 'NONE',  ( -0.9993908270190956511, 0.03489949670250202390, 3.491481338843132961E-15 ) ) ;
#17383 = CARTESIAN_POINT ( 'NONE',  ( -58.49999999999997158, -1.184343223768586029, -3.558065644182723641 ) ) ;
#17384 = AXIS2_PLACEMENT_3D ( 'NONE', #20167, #3361, #25358 ) ;
#17385 = CARTESIAN_POINT ( 'NONE',  ( -58.06249999999996447, 3.400000000000007905, -1.844164440896605116E-13 ) ) ;
#17386 = AXIS2_PLACEMENT_3D ( 'NONE', #8951, #8361, #18042 ) ;
#17387 = CARTESIAN_POINT ( 'NONE',  ( 15.32766723174653478, -2.228024565339382868, -4.927420728799232208 ) ) ;
#17388 = DIRECTION ( 'NONE',  ( 0.000000000000000000, 0.000000000000000000, 1.000000000000000000 ) ) ;
#17389 = CARTESIAN_POINT ( 'NONE',  ( 57.05000000000001847, 0.7500000000000000000, 1.778341924377873751 ) ) ;
#17390 = PRODUCT_DEFINITION_SHAPE ( 'NONE', 'NONE',  #26371 ) ;
#17391 = DIRECTION ( 'NONE',  ( 0.000000000000000000, -1.000000000000000000, 0.000000000000000000 ) ) ;
#17392 = CARTESIAN_POINT ( 'NONE',  ( 16.10660252424457184, 0.2875137064282154986, 5.407399902318745788 ) ) ;
#17393 = ORIENTED_EDGE ( 'NONE', *, *, #3047, .T. ) ;
#17394 = CARTESIAN_POINT ( 'NONE',  ( 15.81621483022863117, -3.777141534544287804, 3.869853550719713375 ) ) ;
#17395 = B_SPLINE_CURVE_WITH_KNOTS ( 'NONE', 3,
 ( #16822, #13625, #1597, #20936, #30567, #6523 ),
 .UNSPECIFIED., .F., .F.,
 ( 4, 2, 4 ),
 ( 0.001078866813306119657, 0.002246630675358731073, 0.003414394537411343140 ),
 .UNSPECIFIED. ) ;
#17396 = EDGE_CURVE ( 'NONE', #14732, #125, #30632, .T. ) ;
#17397 = EDGE_CURVE ( 'NONE', #26101, #7915, #7960, .T. ) ;
#17398 = CARTESIAN_POINT ( 'NONE',  ( 15.18463186935388087, 1.123735532908831436, -5.289358697221507200 ) ) ;
#17400 = EDGE_CURVE ( 'NONE', #1198, #2938, #22561, .T. ) ;
#17399 = DIRECTION ( 'NONE',  ( 8.778969181338835100E-15, -0.8381322357048270888, -0.5454670984325526994 ) ) ;
#17401 = AXIS2_PLACEMENT_3D ( 'NONE', #15514, #8225, #22815 ) ;
#17402 = FACE_OUTER_BOUND ( 'NONE', #21655, .T. ) ;
#17404 = DIRECTION ( 'NONE',  ( 0.000000000000000000, 0.000000000000000000, 1.000000000000000000 ) ) ;
#17403 = CARTESIAN_POINT ( 'NONE',  ( 58.75000000000003553, -1.469015551795940233, -1.320082690053872465 ) ) ;
#17405 = ORIENTED_EDGE ( 'NONE', *, *, #26283, .T. ) ;
#17406 = CARTESIAN_POINT ( 'NONE',  ( 69.20000000000003126, 1.401298464324817071E-42, -7.248315259438346108E-13 ) ) ;
#17407 = EDGE_LOOP ( 'NONE', ( #3367, #19992, #14869, #22699 ) ) ;
#17408 = UNCERTAINTY_MEASURE_WITH_UNIT (LENGTH_MEASURE( 1.000000000000000082E-05 ), #5905, 'distance_accuracy_value', 'NONE');
#17409 = CARTESIAN_POINT ( 'NONE',  ( 61.00000000000001421, 0.8666666666673055186, 1.374595900215364930 ) ) ;
#17410 = CIRCLE ( 'NONE', #22976, 3.499999999999999556 ) ;
#17412 = DIRECTION ( 'NONE',  ( 0.000000000000000000, 0.000000000000000000, 1.000000000000000000 ) ) ;
#17411 = CARTESIAN_POINT ( 'NONE',  ( 15.29449157529458958, -3.378578820314290354, -3.972872285093437927 ) ) ;
#17413 = CYLINDRICAL_SURFACE ( 'NONE', #11517, 0.09999999999999886757 ) ;
#17414 = ORIENTED_EDGE ( 'NONE', *, *, #27046, .F. ) ;
#17415 = CIRCLE ( 'NONE', #8303, 4.350000000000019185 ) ;
#17416 = ORIENTED_EDGE ( 'NONE', *, *, #6509, .F. ) ;
#17417 = CARTESIAN_POINT ( 'NONE',  ( 68.00000000000004263, 0.5000000000000000000, 1.988246715072644166 ) ) ;
#17418 = CARTESIAN_POINT ( 'NONE',  ( 52.06628335902944826, 0.5434431642986600197, 1.718465885608439381 ) ) ;
#17419 = VERTEX_POINT ( 'NONE', #13753 ) ;
#17420 = CARTESIAN_POINT ( 'NONE',  ( 54.19048439011715601, 6.697865729247673983, 2.049999999999811084 ) ) ;
#17421 = CARTESIAN_POINT ( 'NONE',  ( -54.44999999999997442, -1.499999999999999556, -3.300094695611020867 ) ) ;
#17422 = CARTESIAN_POINT ( 'NONE',  ( 51.80000000000002558, -3.908336260473453727, 1.238913909465738872 ) ) ;
#17423 = EDGE_LOOP ( 'NONE', ( #28242, #20761, #23713, #8724 ) ) ;
#17424 = CARTESIAN_POINT ( 'NONE',  ( 0.000000000000000000, 0.000000000000000000, 0.000000000000000000 ) ) ;
#17425 = DIRECTION ( 'NONE',  ( 0.000000000000000000, -1.000000000000000000, 0.000000000000000000 ) ) ;
#17426 = CIRCLE ( 'NONE', #25508, 2.649999999999999911 ) ;
#17427 = ORIENTED_EDGE ( 'NONE', *, *, #18504, .F. ) ;
#17428 = CARTESIAN_POINT ( 'NONE',  ( -56.50952994616203995, 3.117691453623994580, -1.800000000000187006 ) ) ;
#17429 = AXIS2_PLACEMENT_3D ( 'NONE', #7646, #17458, #17308 ) ;
#17430 = CARTESIAN_POINT ( 'NONE',  ( -62.39999999999998437, 1.076401154667962023E-15, 2.259002067258145746E-15 ) ) ;
#17431 = DIRECTION ( 'NONE',  ( 1.000000000000000000, 3.054025858079668409E-16, -2.042474015755241579E-16 ) ) ;
#17432 = CARTESIAN_POINT ( 'NONE',  ( -54.44999999999997442, 0.000000000000000000, 4.700000000000000178 ) ) ;
#17433 = EDGE_CURVE ( 'NONE', #363, #30852, #30111, .T. ) ;
#17434 = CARTESIAN_POINT ( 'NONE',  ( 51.80595691730878372, -4.272100939101181716, -0.9440912809989533416 ) ) ;
#17435 = ADVANCED_FACE ( 'NONE', ( #15987 ), #11234, .T. ) ;
#17436 = DIRECTION ( 'NONE',  ( -1.000000000000000000, -3.053848253006669023E-16, 2.042510438544995415E-16 ) ) ;
#17439 = EDGE_CURVE ( 'NONE', #17195, #16857, #25380, .T. ) ;
#17438 = CARTESIAN_POINT ( 'NONE',  ( -61.36734273774667514, -2.561240237610082904, -0.8152598366033302346 ) ) ;
#17437 = DIRECTION ( 'NONE',  ( 0.000000000000000000, -0.9783524716136640098, -0.2069455031824436186 ) ) ;
#17440 =( BOUNDED_SURFACE ( )  B_SPLINE_SURFACE ( 3, 2, ( 
 ( #882, #30149, #27317 ),
 ( #17507, #8008, #5630 ),
 ( #24782, #3091, #15280 ),
 ( #3247, #30784, #23350 ),
 ( #1633, #4330, #28084 ),
 ( #4173, #30453, #9097 ),
 ( #13669, #20975, #23676 ),
 ( #6874, #13812, #3870 ) ),
 .UNSPECIFIED., .F., .F., .T. ) 
 B_SPLINE_SURFACE_WITH_KNOTS ( ( 4, 2, 2, 4 ),
 ( 3, 3 ),
 ( 0.001762834131042899420, 0.001945267826973971163, 0.002127701522905042688, 0.002492568914767185739 ),
 ( 0.000000000000000000, 1.000000000000000000 ),
 .UNSPECIFIED. ) 
 GEOMETRIC_REPRESENTATION_ITEM ( )  RATIONAL_B_SPLINE_SURFACE ( (
 ( 1.000000000000000000, 0.8699658093904929501, 1.000000000000000000),
 ( 1.000000000000000000, 0.8851796357839230023, 1.000000000000000000),
 ( 1.000000000000000000, 0.8977447492167212051, 1.000000000000000000),
 ( 1.000000000000000000, 0.9127836411835494879, 1.000000000000000000),
 ( 1.000000000000000000, 0.9151168517135812586, 1.000000000000000000),
 ( 1.000000000000000000, 0.9045976586032165034, 1.000000000000000000),
 ( 1.000000000000000000, 0.8745315534097246601, 1.000000000000000000),
 ( 1.000000000000000000, 0.8388746406931713029, 1.000000000000000000) ) ) 
 REPRESENTATION_ITEM ( '' )  SURFACE ( )  );
#17441 = AXIS2_PLACEMENT_3D ( 'NONE', #31109, #8945, #28751 ) ;
#17442 = FACE_OUTER_BOUND ( 'NONE', #19577, .T. ) ;
#17443 = CARTESIAN_POINT ( 'NONE',  ( 69.01464466094067518, 4.111760188415125337E-16, -2.985355339060038027 ) ) ;
#17445 = LINE ( 'NONE', #9714, #20566 ) ;
#17444 = CARTESIAN_POINT ( 'NONE',  ( 15.41170998834799022, 4.895911367890965593, -2.323639554370032112 ) ) ;
#17446 = ORIENTED_EDGE ( 'NONE', *, *, #30368, .T. ) ;
#17447 = CARTESIAN_POINT ( 'NONE',  ( 50.39865716130687190, -0.9106118309512859499, -3.923752762110600312 ) ) ;
#17448 = AXIS2_PLACEMENT_3D ( 'NONE', #5902, #27744, #30414 ) ;
#17449 = CARTESIAN_POINT ( 'NONE',  ( 51.79433046211416070, 3.849974775422116746, 1.576777095043395471 ) ) ;
#17451 = FACE_OUTER_BOUND ( 'NONE', #29014, .T. ) ;
#17450 = CARTESIAN_POINT ( 'NONE',  ( 15.66436536804550705, 3.496282614933925448, -4.130238739723488095 ) ) ;
#17452 = CARTESIAN_POINT ( 'NONE',  ( 47.27826922991183523, -4.267091652301661320, 1.720255306494459235 ) ) ;
#17453 = ORIENTED_EDGE ( 'NONE', *, *, #5756, .T. ) ;
#17454 = LINE ( 'NONE', #15235, #13955 ) ;
#17455 = ADVANCED_FACE ( 'NONE', ( #5204 ), #11936, .T. ) ;
#17456 = ORIENTED_EDGE ( 'NONE', *, *, #27046, .T. ) ;
#17457 = TOROIDAL_SURFACE ( 'NONE', #31106, 2.549999999999999822, 0.05000000000000000278 ) ;
#17458 = DIRECTION ( 'NONE',  ( -1.000000000000000000, -2.586136946169074517E-16, 0.000000000000000000 ) ) ;
#17459 = ORIENTED_EDGE ( 'NONE', *, *, #19545, .F. ) ;
#17460 = ORIENTED_EDGE ( 'NONE', *, *, #16543, .F. ) ;
#17461 = CARTESIAN_POINT ( 'NONE',  ( 15.95705409078463433, 5.298557911012508725, 1.088945631943511128 ) ) ;
#17462 = ORIENTED_EDGE ( 'NONE', *, *, #28147, .F. ) ;
#17463 = CARTESIAN_POINT ( 'NONE',  ( 31.71120695424772151, 7.553129896932145648, 1.949999999999888045 ) ) ;
#17464 = CARTESIAN_POINT ( 'NONE',  ( -60.07202994616204705, 2.078460969082646770, 3.599999999999794031 ) ) ;
#17465 = EDGE_LOOP ( 'NONE', ( #22888, #8466, #3286, #22712 ) ) ;
#17466 = CARTESIAN_POINT ( 'NONE',  ( 54.50000000000002132, -0.003244837758135472351, 4.274998768541100169 ) ) ;
#17467 = ORIENTED_EDGE ( 'NONE', *, *, #6157, .F. ) ;
#17468 = PRODUCT_DEFINITION ( 'UNKNOWN', '', #19727, #10442 ) ;
#17469 = CARTESIAN_POINT ( 'NONE',  ( 58.75000000000002132, 6.153735859711025284E-13, 3.111507638930570854E-58 ) ) ;
#17470 = VECTOR ( 'NONE', #21401, 1000.000000000000000 ) ;
#17471 = CARTESIAN_POINT ( 'NONE',  ( 22.41225425035782237, 6.886225699534909594, 1.949999999999887823 ) ) ;
#17472 = ORIENTED_EDGE ( 'NONE', *, *, #25702, .F. ) ;
#17473 = AXIS2_PLACEMENT_3D ( 'NONE', #15878, #4313, #6232 ) ;
#17474 = DIRECTION ( 'NONE',  ( -1.000000000000000000, -0.000000000000000000, 0.000000000000000000 ) ) ;
#17475 = CARTESIAN_POINT ( 'NONE',  ( 51.29777716379115304, 3.891287491069770788, -2.050000000000178790 ) ) ;
#17476 = CARTESIAN_POINT ( 'NONE',  ( 64.95000000000005969, 4.898587196589412829E-16, 3.999999999999320099 ) ) ;
#17477 = CARTESIAN_POINT ( 'NONE',  ( 69.20000000000005969, 0.8382352941176473005, 2.222158093316557004 ) ) ;
#17478 = B_SPLINE_CURVE_WITH_KNOTS ( 'NONE', 3,
 ( #18160, #24828, #18458, #759, #25411, #10422, #17392, #28096, #29420, #27036, #15016, #16080, #12634, #17562, #22318, #6110 ),
 .UNSPECIFIED., .F., .F.,
 ( 4, 2, 2, 2, 2, 2, 2, 4 ),
 ( 1.748223473168675632E-18, 0.0004351083927046447584, 0.0008702167854092877821, 0.001740433570818574263, 0.002175541963523217395, 0.002610650356227860094, 0.003045758748932503226, 0.003480867141637146792 ),
 .UNSPECIFIED. ) ;
#17479 = AXIS2_PLACEMENT_3D ( 'NONE', #26365, #14892, #5568 ) ;
#17480 = CARTESIAN_POINT ( 'NONE',  ( 57.01990854087920013, -0.7399312420039723115, 2.427820937803477630 ) ) ;
#17481 = TOROIDAL_SURFACE ( 'NONE', #30095, 4.199999999999954881, 0.1000000000000000056 ) ;
#17482 = EDGE_CURVE ( 'NONE', #7995, #28086, #9672, .T. ) ;
#17483 =( BOUNDED_CURVE ( )  B_SPLINE_CURVE ( 3, ( #16871, #21795, #24444, #387 ),
 .UNSPECIFIED., .F., .T. ) 
 B_SPLINE_CURVE_WITH_KNOTS ( ( 4, 4 ),
 ( 1.853935925778139149, 1.936702241689763682 ),
 .UNSPECIFIED. ) 
 CURVE ( )  GEOMETRIC_REPRESENTATION_ITEM ( )  RATIONAL_B_SPLINE_CURVE ( ( 1.000000000000000000, 0.9994292262101478475, 0.9994292262101478475, 1.000000000000000000 ) ) 
 REPRESENTATION_ITEM ( '' )  );
#17484 = CIRCLE ( 'NONE', #15464, 1.975000000000001865 ) ;
#17486 = CYLINDRICAL_SURFACE ( 'NONE', #21510, 0.1499999999999999667 ) ;
#17485 = CARTESIAN_POINT ( 'NONE',  ( -36.58413561666692715, -3.261791109367169206, 4.314133646218629714 ) ) ;
#17487 = DIRECTION ( 'NONE',  ( 1.000000000000000000, -1.219044193948983948E-29, 3.491481338843133355E-15 ) ) ;
#17488 = DIRECTION ( 'NONE',  ( -0.7313537016191670181, -0.6819983600625022513, 2.468850131082252327E-15 ) ) ;
#17489 = FACE_OUTER_BOUND ( 'NONE', #14594, .T. ) ;
#17490 = CARTESIAN_POINT ( 'NONE',  ( 61.24312156765952864, -0.9166010152742726236, -1.712896921565310260 ) ) ;
#17491 = ORIENTED_EDGE ( 'NONE', *, *, #10095, .T. ) ;
#17492 = CIRCLE ( 'NONE', #15963, 1.240000000000000213 ) ;
#17493 = AXIS2_PLACEMENT_3D ( 'NONE', #9846, #5238, #12523 ) ;
#17494 = ORIENTED_EDGE ( 'NONE', *, *, #1526, .T. ) ;
#17495 = ADVANCED_FACE ( 'NONE', ( #901 ), #10555, .T. ) ;
#17496 = ORIENTED_EDGE ( 'NONE', *, *, #21865, .T. ) ;
#17497 = CARTESIAN_POINT ( 'NONE',  ( -62.08111617280007266, -2.505022497657029223, -0.3170112821859903951 ) ) ;
#17498 = CARTESIAN_POINT ( 'NONE',  ( -56.86042740578360366, -2.936324665650200672, -2.606018187048497747 ) ) ;
#17500 = CARTESIAN_POINT ( 'NONE',  ( -61.36641165373034568, -2.598025853916357431, 0.6858830576151544456 ) ) ;
#17499 = DIRECTION ( 'NONE',  ( -1.000000000000000000, -3.053848253006669023E-16, 2.042510438544995169E-16 ) ) ;
#17501 = EDGE_LOOP ( 'NONE', ( #19989, #21275, #326, #22558 ) ) ;
#17502 = ORIENTED_EDGE ( 'NONE', *, *, #16363, .F. ) ;
#17503 = CARTESIAN_POINT ( 'NONE',  ( 51.41755241844363411, -4.256411467774983137, -1.449592950258013380 ) ) ;
#17504 = ORIENTED_EDGE ( 'NONE', *, *, #1348, .T. ) ;
#17505 = AXIS2_PLACEMENT_3D ( 'NONE', #14784, #7207, #26684 ) ;
#17507 = CARTESIAN_POINT ( 'NONE',  ( 51.55144386500324316, 1.037443573995146862, -1.251214392908886142 ) ) ;
#17506 = AXIS2_PLACEMENT_3D ( 'NONE', #6543, #28235, #11915 ) ;
#17508 = ORIENTED_EDGE ( 'NONE', *, *, #248, .F. ) ;
#17509 = CARTESIAN_POINT ( 'NONE',  ( 29.99460040655550941, 6.535150012678215603, -1.950000000000102984 ) ) ;
#17510 = CIRCLE ( 'NONE', #16513, 0.04999999999999987094 ) ;
#17511 = CARTESIAN_POINT ( 'NONE',  ( -57.08155989232412963, 3.400000000000007905, -1.873796572744660248E-13 ) ) ;
#17512 = CARTESIAN_POINT ( 'NONE',  ( -59.12499999999996447, -2.944486372867072266, -1.700000000000227995 ) ) ;
#17513 = AXIS2_PLACEMENT_3D ( 'NONE', #22704, #20788, #20173 ) ;
#17514 = CARTESIAN_POINT ( 'NONE',  ( 15.95705409078465564, -5.298557911012522936, -1.088945631943473602 ) ) ;
#17515 = CARTESIAN_POINT ( 'NONE',  ( -60.14405989232410832, 2.944486372867106461, -1.700000000000200684 ) ) ;
#17516 = CARTESIAN_POINT ( 'NONE',  ( 52.02275531408256626, 3.834498708141866885, -2.050000000000181455 ) ) ;
#17517 = DIRECTION ( 'NONE',  ( -1.000000000000000000, -0.000000000000000000, -0.000000000000000000 ) ) ;
#17518 = EDGE_CURVE ( 'NONE', #26028, #14388, #9809, .T. ) ;
#17519 = CARTESIAN_POINT ( 'NONE',  ( 58.75000000000002132, -0.5380862305903304499, -1.858165151418244010 ) ) ;
#17520 = CIRCLE ( 'NONE', #7902, 0.1500000000000001887 ) ;
#17521 = CARTESIAN_POINT ( 'NONE',  ( 50.25000000000004263, -1.800471618824803111, 1.039502773796719959 ) ) ;
#17523 = EDGE_CURVE ( 'NONE', #11981, #28401, #14944, .T. ) ;
#17522 = CARTESIAN_POINT ( 'NONE',  ( 51.23644008536121675, 1.080112125196981410, -1.214076932077873039 ) ) ;
#17524 = ADVANCED_FACE ( 'NONE', ( #16646 ), #14242, .F. ) ;
#17525 = MECHANICAL_DESIGN_GEOMETRIC_PRESENTATION_REPRESENTATION (  '', ( #7908 ), #15993 ) ;
#17526 = AXIS2_PLACEMENT_3D ( 'NONE', #1190, #30627, #28427 ) ;
#17527 = FACE_OUTER_BOUND ( 'NONE', #16258, .T. ) ;
#17528 = DIRECTION ( 'NONE',  ( 0.000000000000000000, 0.000000000000000000, -1.000000000000000000 ) ) ;
#17529 = AXIS2_PLACEMENT_3D ( 'NONE', #16460, #13905, #30873 ) ;
#17530 = STYLED_ITEM ( 'NONE', ( #26326 ), #26054 ) ;
#17531 = CARTESIAN_POINT ( 'NONE',  ( 51.11922224407864945, -0.9310536428529800901, 1.338077479437885131 ) ) ;
#17532 = ORIENTED_EDGE ( 'NONE', *, *, #14395, .F. ) ;
#17533 = DIRECTION ( 'NONE',  ( -1.000000000000000000, -3.053848253006669023E-16, 2.042510438544995415E-16 ) ) ;
#17534 = CARTESIAN_POINT ( 'NONE',  ( -35.85663232820597557, -2.525801270006294619, -4.794550352686338002 ) ) ;
#17535 = CARTESIAN_POINT ( 'NONE',  ( 54.41366571437521316, 6.718673005292165712, 1.624999999999810374 ) ) ;
#17536 = ORIENTED_EDGE ( 'NONE', *, *, #27308, .F. ) ;
#17537 = EDGE_CURVE ( 'NONE', #23786, #10712, #23912, .T. ) ;
#17538 = CARTESIAN_POINT ( 'NONE',  ( 50.45683212279337226, 1.211455355144567703, -3.917539841352833285 ) ) ;
#17539 = ORIENTED_EDGE ( 'NONE', *, *, #1261, .T. ) ;
#17540 = CARTESIAN_POINT ( 'NONE',  ( 51.45655683570191741, -0.9591657938390834026, 1.611094652690528095 ) ) ;
#17541 = FACE_OUTER_BOUND ( 'NONE', #19538, .T. ) ;
#17543 = CARTESIAN_POINT ( 'NONE',  ( -61.82074345547174232, -2.669507762876991208, -0.4182503418061432332 ) ) ;
#17542 = DIRECTION ( 'NONE',  ( 1.000000000000000000, 0.000000000000000000, -1.047444401652940007E-14 ) ) ;
#17544 = VERTEX_POINT ( 'NONE', #4731 ) ;
#17545 = AXIS2_PLACEMENT_3D ( 'NONE', #21876, #17, #19339 ) ;
#17546 = CARTESIAN_POINT ( 'NONE',  ( -57.51905989232412963, -2.944486372867094470, 1.699999999999774802 ) ) ;
#17547 = DIRECTION ( 'NONE',  ( 1.000000000000000000, 0.000000000000000000, 0.000000000000000000 ) ) ;
#17548 = ORIENTED_EDGE ( 'NONE', *, *, #25846, .F. ) ;
#17550 = DIRECTION ( 'NONE',  ( 1.000000000000000000, 1.047444401652940007E-14, -0.000000000000000000 ) ) ;
#17549 = CARTESIAN_POINT ( 'NONE',  ( 52.92035180444707976, 4.185175181814600798, 2.047053903428833976 ) ) ;
#17551 = DIRECTION ( 'NONE',  ( 1.000000000000000000, 1.047444401652940007E-14, 0.000000000000000000 ) ) ;
#17552 = CARTESIAN_POINT ( 'NONE',  ( -58.06249999999997158, -0.8699069336946626541, 4.241846523238428368 ) ) ;
#17553 = DIRECTION ( 'NONE',  ( -1.000000000000000000, -3.053848253006669023E-16, 2.042510438544995415E-16 ) ) ;
#17555 = EDGE_CURVE ( 'NONE', #31290, #29622, #6820, .T. ) ;
#17554 = AXIS2_PLACEMENT_3D ( 'NONE', #17915, #808, #17767 ) ;
#17556 = CARTESIAN_POINT ( 'NONE',  ( -54.70655989232413674, 1.962990915244722467, 3.399999999999812950 ) ) ;
#17557 = AXIS2_PLACEMENT_3D ( 'NONE', #16723, #3506, #27723 ) ;
#17558 = DIRECTION ( 'NONE',  ( 0.000000000000000000, -0.1576190026614809614, -0.9875000000000001554 ) ) ;
#17559 = TOROIDAL_SURFACE ( 'NONE', #30175, 1.975000000000001865, 0.1000000000000000056 ) ;
#17560 = CIRCLE ( 'NONE', #21630, 0.8749999999999990008 ) ;
#17561 = DIRECTION ( 'NONE',  ( 1.189524669241239263E-14, 0.000000000000000000, 1.000000000000000000 ) ) ;
#17562 = CARTESIAN_POINT ( 'NONE',  ( 15.32766723174653123, -1.093755498983960628, 5.295967089285813501 ) ) ;
#17563 = ORIENTED_EDGE ( 'NONE', *, *, #1150, .F. ) ;
#17564 = EDGE_CURVE ( 'NONE', #833, #17335, #14895, .T. ) ;
#17565 = CARTESIAN_POINT ( 'NONE',  ( 15.41170998834774686, -2.595074437874647533, 4.757608386865062045 ) ) ;
#17566 = ADVANCED_FACE ( 'NONE', ( #13073 ), #28104, .T. ) ;
#17567 = AXIS2_PLACEMENT_3D ( 'NONE', #13419, #20602, #3636 ) ;
#17568 = ADVANCED_FACE ( 'NONE', ( #18308 ), #19977, .T. ) ;
#17569 = AXIS2_PLACEMENT_3D ( 'NONE', #16442, #23577, #9653 ) ;
#17570 = DIRECTION ( 'NONE',  ( 0.000000000000000000, 0.000000000000000000, 1.000000000000000000 ) ) ;
#17571 = AXIS2_PLACEMENT_3D ( 'NONE', #15551, #11100, #5893 ) ;
#17572 = DIRECTION ( 'NONE',  ( 0.000000000000000000, 0.2008964009354147762, -0.9796124928211140670 ) ) ;
#17573 = CARTESIAN_POINT ( 'NONE',  ( -59.32202994616204705, 2.078460969082640108, 3.599999999999799805 ) ) ;
#17574 = DIRECTION ( 'NONE',  ( 0.000000000000000000, -0.2008964009354147762, 0.9796124928211139560 ) ) ;
#17575 = CARTESIAN_POINT ( 'NONE',  ( 24.78376069717984009, 5.502839434325734302, 2.049999999999912781 ) ) ;
#17576 = EDGE_LOOP ( 'NONE', ( #17062, #16690, #9411, #6707 ) ) ;
#17577 = AXIS2_PLACEMENT_3D ( 'NONE', #1070, #24816, #15643 ) ;
#17578 = VECTOR ( 'NONE', #27179, 1000.000000000000000 ) ;
#17579 = ORIENTED_EDGE ( 'NONE', *, *, #13333, .T. ) ;
#17580 = AXIS2_PLACEMENT_3D ( 'NONE', #29890, #29561, #24823 ) ;
#17581 = CARTESIAN_POINT ( 'NONE',  ( -59.12208601139542452, 2.471957471229930370, -0.9603292137297660958 ) ) ;
#17583 = DIRECTION ( 'NONE',  ( -1.000000000000000000, -2.586136946169074517E-16, 0.000000000000000000 ) ) ;
#17582 = CARTESIAN_POINT ( 'NONE',  ( -54.49999999999997158, -2.083909216633824890, -2.852996025551205683 ) ) ;
#17584 = ORIENTED_EDGE ( 'NONE', *, *, #12959, .T. ) ;
#17585 = ORIENTED_EDGE ( 'NONE', *, *, #1858, .F. ) ;
#17586 = CARTESIAN_POINT ( 'NONE',  ( -60.44999999999996021, 0.8596938233273155872, -4.192045280110956895 ) ) ;
#17587 = DIRECTION ( 'NONE',  ( 0.000000000000000000, 0.000000000000000000, -1.000000000000000000 ) ) ;
#17588 = ORIENTED_EDGE ( 'NONE', *, *, #17953, .T. ) ;
#17590 = DIRECTION ( 'NONE',  ( -0.9956821769042237813, -0.09282781153978682254, 3.493224332854920750E-15 ) ) ;
#17589 = CARTESIAN_POINT ( 'NONE',  ( -57.50952994616203995, -3.117691453623963938, -1.800000000000215206 ) ) ;
#17591 = CARTESIAN_POINT ( 'NONE',  ( -54.29792740578361077, 3.330682475591790315, 0.6830477631804100502 ) ) ;
#17592 = AXIS2_PLACEMENT_3D ( 'NONE', #1072, #1211, #30028 ) ;
#17593 = EDGE_CURVE ( 'NONE', #27011, #26152, #1510, .T. ) ;
#17594 = CARTESIAN_POINT ( 'NONE',  ( -36.26369610968610147, -4.878538113278866106, -1.812957040858122149 ) ) ;
#17595 = DIRECTION ( 'NONE',  ( 0.000000000000000000, 0.000000000000000000, 1.000000000000000000 ) ) ;
#17596 = CARTESIAN_POINT ( 'NONE',  ( 58.75000000000003553, -1.320082690053552499, -1.469015551796290175 ) ) ;
#17597 = CIRCLE ( 'NONE', #12039, 0.09999999999999982514 ) ;
#17598 = ADVANCED_FACE ( 'NONE', ( #13538 ), #3722, .T. ) ;
#17599 = ORIENTED_EDGE ( 'NONE', *, *, #28131, .T. ) ;
#17600 = CARTESIAN_POINT ( 'NONE',  ( -59.00952994616203284, -3.117691453623963938, -1.800000000000220757 ) ) ;
#17601 = CARTESIAN_POINT ( 'NONE',  ( -59.66183546925923764, -3.174920041538525251, -1.216504307364950854 ) ) ;
#17602 = FACE_OUTER_BOUND ( 'NONE', #13728, .T. ) ;
#17603 = B_SPLINE_CURVE_WITH_KNOTS ( 'NONE', 3,
 ( #13992, #31269, #2455, #9594 ),
 .UNSPECIFIED., .F., .F.,
 ( 4, 4 ),
 ( 1.084202172485504434E-19, 0.0001494103359351852626 ),
 .UNSPECIFIED. ) ;
#17604 = CARTESIAN_POINT ( 'NONE',  ( 15.98305126557428579, -0.5375162698822371077, 5.381098085087400840 ) ) ;
#17605 = CARTESIAN_POINT ( 'NONE',  ( 51.60173421008559558, -3.901954665936026245, 1.539656138810567398 ) ) ;
#17606 = CARTESIAN_POINT ( 'NONE',  ( -61.34999999999997300, 1.397055221233662433E-15, 2.044538471210920981E-15 ) ) ;
#17608 = CARTESIAN_POINT ( 'NONE',  ( 15.03925126672133139, -5.377732432866646484, -0.5657657256215582464 ) ) ;
#17607 = CARTESIAN_POINT ( 'NONE',  ( 22.54717926605044198, 7.740376438784147162, -1.425000000000078204 ) ) ;
#17609 = AXIS2_PLACEMENT_3D ( 'NONE', #20866, #6283, #10872 ) ;
#17610 = LINE ( 'NONE', #22359, #31198 ) ;
#17611 = CARTESIAN_POINT ( 'NONE',  ( 15.59140265158955962, -3.917459231545690646, 3.727878977586795095 ) ) ;
#17613 = DIRECTION ( 'NONE',  ( -1.000000000000000000, 0.000000000000000000, 1.047444401652940007E-14 ) ) ;
#17612 = DIRECTION ( 'NONE',  ( 1.000000000000000000, 1.047444401652940007E-14, 0.000000000000000000 ) ) ;
#17614 = ORIENTED_EDGE ( 'NONE', *, *, #2709, .T. ) ;
#17615 = CARTESIAN_POINT ( 'NONE',  ( 50.49731436448253419, -0.9333771270347004378, -3.994943142064449670 ) ) ;
#17616 = DIRECTION ( 'NONE',  ( -1.000000000000000000, -3.054025858079668409E-16, 2.042474015755241579E-16 ) ) ;
#17617 = B_SPLINE_CURVE_WITH_KNOTS ( 'NONE', 3,
 ( #15608, #3573, #13521, #27790, #22892, #1337 ),
 .UNSPECIFIED., .F., .F.,
 ( 4, 2, 4 ),
 ( 0.000000000000000000, 0.0001917282624435965362, 0.0003834565248871930725 ),
 .UNSPECIFIED. ) ;
#17619 = CARTESIAN_POINT ( 'NONE',  ( 69.20000000000003126, 4.557543281186736018E-17, -7.248315259438346108E-13 ) ) ;
#17618 = CARTESIAN_POINT ( 'NONE',  ( 15.76675455518197566, 3.095036031508724861, -4.435288302043498554 ) ) ;
#17620 = CARTESIAN_POINT ( 'NONE',  ( -58.43749999999997158, -3.399999999999991029, -2.253785087031484148E-13 ) ) ;
#17621 = ORIENTED_EDGE ( 'NONE', *, *, #5129, .T. ) ;
#17622 = DIRECTION ( 'NONE',  ( 0.000000000000000000, 1.000000000000000000, 3.491481338843130594E-15 ) ) ;
#17623 = CARTESIAN_POINT ( 'NONE',  ( 54.19386703870442545, 5.671865141453449333, -2.050000000000189004 ) ) ;
#17624 = B_SPLINE_CURVE_WITH_KNOTS ( 'NONE', 3,
 ( #28065, #6383, #16047, #25700, #20958, #19811, #24251, #9694, #24541, #29304, #7303, #7756, #32 ),
 .UNSPECIFIED., .F., .F.,
 ( 4, 3, 3, 3, 4 ),
 ( 3.529906531158615134E-18, 3.856107938921464966E-05, 7.311388640164024157E-05, 0.0001107339254823213112, 0.0001129379781057718247 ),
 .UNSPECIFIED. ) ;
#17625 = VERTEX_POINT ( 'NONE', #13365 ) ;
#17626 = DIRECTION ( 'NONE',  ( 1.000000000000000000, 0.000000000000000000, 0.000000000000000000 ) ) ;
#17627 = ORIENTED_EDGE ( 'NONE', *, *, #20575, .F. ) ;
#17628 = VERTEX_POINT ( 'NONE', #20537 ) ;
#17629 = ADVANCED_FACE ( 'NONE', ( #6427 ), #29574, .T. ) ;
#17630 = CARTESIAN_POINT ( 'NONE',  ( 15.32766723174652945, 5.374753047227047276, -0.5963205376973405025 ) ) ;
#17631 = ORIENTED_EDGE ( 'NONE', *, *, #1606, .F. ) ;
#17632 = ADVANCED_FACE ( 'NONE', ( #5970 ), #10849, .F. ) ;
#17633 = CARTESIAN_POINT ( 'NONE',  ( 36.50000000000002132, 0.000000000000000000, 0.000000000000000000 ) ) ;
#17634 = CARTESIAN_POINT ( 'NONE',  ( -55.20655989232412963, -3.925981830489445379, -2.103125626221096647E-13 ) ) ;
#17635 = ORIENTED_EDGE ( 'NONE', *, *, #28366, .F. ) ;
#17636 = FACE_OUTER_BOUND ( 'NONE', #27157, .T. ) ;
#17637 = ADVANCED_FACE ( 'NONE', ( #1192 ), #8488, .F. ) ;
#17638 = DIRECTION ( 'NONE',  ( 0.000000000000000000, 0.000000000000000000, 1.000000000000000000 ) ) ;
#17639 = AXIS2_PLACEMENT_3D ( 'NONE', #26907, #5216, #16808 ) ;
#17640 = CARTESIAN_POINT ( 'NONE',  ( 22.72181155690791954, 6.520914527883612699, 2.050000000000084199 ) ) ;
#17641 = ORIENTED_EDGE ( 'NONE', *, *, #4142, .F. ) ;
#17642 = VECTOR ( 'NONE', #5439, 999.9999999999998863 ) ;
#17643 = CARTESIAN_POINT ( 'NONE',  ( 50.87477060347373481, 8.633605004118187765, -1.550000000000176792 ) ) ;
#17644 =( BOUNDED_SURFACE ( )  B_SPLINE_SURFACE ( 3, 2, ( 
 ( #25521, #25377, #3679 ),
 ( #1300, #24899, #3386 ),
 ( #5919, #30428, #3834 ),
 ( #3220, #848, #10514 ) ),
 .UNSPECIFIED., .F., .F., .T. ) 
 B_SPLINE_SURFACE_WITH_KNOTS ( ( 4, 4 ),
 ( 3, 3 ),
 ( 0.0002753388251024970943, 0.0003797131536038330507 ),
 ( 0.000000000000000000, 1.000000000000000000 ),
 .UNSPECIFIED. ) 
 GEOMETRIC_REPRESENTATION_ITEM ( )  RATIONAL_B_SPLINE_SURFACE ( (
 ( 1.000000000000000000, 0.8543839308486376183, 1.000000000000000000),
 ( 1.000000000000000000, 0.8547349261770162965, 1.000000000000000000),
 ( 1.000000000000000000, 0.7665921203079560931, 1.000000000000000000),
 ( 1.000000000000000000, 0.7071067811865480168, 1.000000000000000000) ) ) 
 REPRESENTATION_ITEM ( '' )  SURFACE ( )  );
#17645 = CARTESIAN_POINT ( 'NONE',  ( 53.94065574304036659, 7.474792160838903854, -2.050000000000186784 ) ) ;
#17646 = CYLINDRICAL_SURFACE ( 'NONE', #6163, 0.1500000000000003830 ) ;
#17647 = DIRECTION ( 'NONE',  ( 1.000000000000000000, 1.047444401652940007E-14, 0.000000000000000000 ) ) ;
#17648 = DIRECTION ( 'NONE',  ( 1.000000000000000000, 1.047444401652940007E-14, 0.000000000000000000 ) ) ;
#17649 = EDGE_CURVE ( 'NONE', #24533, #26979, #12365, .T. ) ;
#17650 = B_SPLINE_CURVE_WITH_KNOTS ( 'NONE', 3,
 ( #13624, #3823, #23166, #20327, #10952, #3369, #22852, #29958, #8719, #16629, #1449, #8265, #18402, #25210, #1287, #6968 ),
 .UNSPECIFIED., .F., .F.,
 ( 4, 2, 2, 2, 2, 2, 2, 4 ),
 ( 1.734723475976807094E-18, 0.0004351083927046425358, 0.0008702167854092833369, 0.001740433570818564289, 0.002175541963523204819, 0.002610650356227844915, 0.003045758748932485445, 0.003480867141637125975 ),
 .UNSPECIFIED. ) ;
#17652 = FACE_OUTER_BOUND ( 'NONE', #7339, .T. ) ;
#17651 = CARTESIAN_POINT ( 'NONE',  ( -57.28335481156723574, 0.7533615035078095046, -3.673546848079178861 ) ) ;
#17653 = DIRECTION ( 'NONE',  ( 0.000000000000000000, 0.000000000000000000, -1.000000000000000000 ) ) ;
#17654 = DIRECTION ( 'NONE',  ( 1.000000000000000000, 0.000000000000000000, -1.047444401652940007E-14 ) ) ;
#17655 = CARTESIAN_POINT ( 'NONE',  ( 58.66118217212537900, 1.313877211064007344, -1.337770226786318295 ) ) ;
#17656 = CARTESIAN_POINT ( 'NONE',  ( 54.19030381964616083, 6.697848500921247172, -2.050000000000189004 ) ) ;
#17657 = EDGE_LOOP ( 'NONE', ( #28547, #1914, #1169, #12814 ) ) ;
#17658 = CARTESIAN_POINT ( 'NONE',  ( -59.69999999999997442, -2.455304892039217091, -1.238538609462283446 ) ) ;
#17659 = ORIENTED_EDGE ( 'NONE', *, *, #16234, .F. ) ;
#17660 = AXIS2_PLACEMENT_3D ( 'NONE', #28070, #22877, #8293 ) ;
#17661 = EDGE_LOOP ( 'NONE', ( #28281, #17771, #4288, #22891 ) ) ;
#17662 = CARTESIAN_POINT ( 'NONE',  ( -71.44999999999998863, -1.380331489585512972E-15, 2.906968604901091669E-15 ) ) ;
#17663 = CARTESIAN_POINT ( 'NONE',  ( -60.04792740578359656, -2.256877952708263635, 2.542931754211925188 ) ) ;
#17665 = CARTESIAN_POINT ( 'NONE',  ( -61.34999999999997300, -2.551764585593653489, 0.6636807913650824009 ) ) ;
#17664 = DIRECTION ( 'NONE',  ( 1.000000000000000000, -0.000000000000000000, -0.000000000000000000 ) ) ;
#17666 = VERTEX_POINT ( 'NONE', #23994 ) ;
#17667 = ORIENTED_EDGE ( 'NONE', *, *, #10619, .T. ) ;
#17668 = CARTESIAN_POINT ( 'NONE',  ( -56.15835481156722153, -0.7533615035077977362, 3.673546848079179750 ) ) ;
#17669 = ORIENTED_EDGE ( 'NONE', *, *, #11830, .F. ) ;
#17670 = ADVANCED_FACE ( 'NONE', ( #7210 ), #6896, .F. ) ;
#17671 = CARTESIAN_POINT ( 'NONE',  ( 51.79423677987253427, 3.849974365564825529, -1.576055568942727358 ) ) ;
#17672 = ORIENTED_EDGE ( 'NONE', *, *, #23017, .F. ) ;
#17673 = CARTESIAN_POINT ( 'NONE',  ( 25.68808851933666304, 5.234409799645237449, -1.950000000000088107 ) ) ;
#17674 = CARTESIAN_POINT ( 'NONE',  ( 58.75000000000000711, 1.895722432252915368, 0.6373668173479852816 ) ) ;
#17675 = VECTOR ( 'NONE', #18856, 1000.000000000000000 ) ;
#17676 = DIRECTION ( 'NONE',  ( 0.000000000000000000, 1.000000000000000000, 0.000000000000000000 ) ) ;
#17677 = B_SPLINE_CURVE_WITH_KNOTS ( 'NONE', 3,
 ( #15550, #20926, #18556, #25202, #10784, #20467, #18094, #8710, #18394, #28029 ),
 .UNSPECIFIED., .F., .F.,
 ( 4, 2, 2, 2, 4 ),
 ( 0.000000000000000000, 0.0003925703575136120483, 0.0007851407150272240966, 0.001177711072540836091, 0.001570281430054448193 ),
 .UNSPECIFIED. ) ;
#17678 =( BOUNDED_SURFACE ( )  B_SPLINE_SURFACE ( 3, 2, ( 
 ( #29320, #19829, #47 ),
 ( #5244, #12676, #9849 ),
 ( #26640, #17291, #9710 ),
 ( #14436, #7943, #14751 ),
 ( #19521, #5409, #26934 ),
 ( #7772, #29171, #5100 ),
 ( #15064, #10307, #29615 ),
 ( #4945, #12526, #19976 ),
 ( #4776, #14894, #24111 ),
 ( #2420, #12083, #19682 ),
 ( #24411, #2579, #22052 ),
 ( #21758, #29009, #7318 ),
 ( #16989, #349, #14603 ),
 ( #10018, #20620, #25489 ),
 ( #1429, #1123, #23144 ),
 ( #22834, #5715, #17911 ) ),
 .UNSPECIFIED., .F., .F., .T. ) 
 B_SPLINE_SURFACE_WITH_KNOTS ( ( 4, 2, 2, 2, 2, 2, 2, 4 ),
 ( 3, 3 ),
 ( 0.001780502285214246314, 0.002558945925323777206, 0.002753556835351159658, 0.002948167745378542544, 0.003337389565433307882, 0.003726611385488073219, 0.004115833205542838991, 0.004894276845652369666 ),
 ( 0.000000000000000000, 1.000000000000000000 ),
 .UNSPECIFIED. ) 
 GEOMETRIC_REPRESENTATION_ITEM ( )  RATIONAL_B_SPLINE_SURFACE ( (
 ( 1.000000000000000000, 0.9418517008537227175, 1.000000000000000000),
 ( 1.000000000000000000, 0.9417987965884626611, 1.000000000000000000),
 ( 1.000000000000000000, 0.9418198861734660143, 1.000000000000000000),
 ( 1.000000000000000000, 0.9434060303845427375, 1.000000000000000000),
 ( 1.000000000000000000, 0.9437939819947938069, 1.000000000000000000),
 ( 1.000000000000000000, 0.9445989566713008934, 1.000000000000000000),
 ( 1.000000000000000000, 0.9450169930049703293, 1.000000000000000000),
 ( 1.000000000000000000, 0.9461610507673812176, 1.000000000000000000),
 ( 1.000000000000000000, 0.9467217966427053932, 1.000000000000000000),
 ( 1.000000000000000000, 0.9467345476124492398, 1.000000000000000000),
 ( 1.000000000000000000, 0.9461964028053072573, 1.000000000000000000),
 ( 1.000000000000000000, 0.9446801822473688270, 1.000000000000000000),
 ( 1.000000000000000000, 0.9437582546536396055, 1.000000000000000000),
 ( 1.000000000000000000, 0.9418129560295979141, 1.000000000000000000),
 ( 1.000000000000000000, 0.9418016889777250933, 1.000000000000000000),
 ( 1.000000000000000000, 0.9418517008537231616, 1.000000000000000000) ) ) 
 REPRESENTATION_ITEM ( '' )  SURFACE ( )  );
#17679 = VECTOR ( 'NONE', #7116, 1000.000000000000000 ) ;
#17680 = CARTESIAN_POINT ( 'NONE',  ( 15.48609859788817289, -4.910307320510440832, -1.715181477143186806 ) ) ;
#17681 = CARTESIAN_POINT ( 'NONE',  ( -59.51905989232410121, 2.023778652682510314E-14, -3.400000000000210854 ) ) ;
#17682 = CARTESIAN_POINT ( 'NONE',  ( 53.91678946233204783, 6.821600947619695710, -2.050000000000123723 ) ) ;
#17683 =( GEOMETRIC_REPRESENTATION_CONTEXT ( 3 ) GLOBAL_UNCERTAINTY_ASSIGNED_CONTEXT ( ( #7904 ) ) GLOBAL_UNIT_ASSIGNED_CONTEXT ( ( #13777, #18405, #11258 ) ) REPRESENTATION_CONTEXT ( 'NONE', 'WORKASPACE' ) );
#17684 = CARTESIAN_POINT ( 'NONE',  ( 47.12365020756617895, -3.859233156638960160, -1.644927388241157473 ) ) ;
#17685 = AXIS2_PLACEMENT_3D ( 'NONE', #11099, #23304, #1587 ) ;
#17686 = ADVANCED_FACE ( 'NONE', ( #18786 ), #9363, .F. ) ;
#17687 = CARTESIAN_POINT ( 'NONE',  ( -62.09999999999997300, 1.168016602258162478E-15, 2.197726754101795588E-15 ) ) ;
#17688 = CARTESIAN_POINT ( 'NONE',  ( 60.67929986713514978, 1.401298464324817071E-42, -6.355819294205068152E-13 ) ) ;
#17689 = AXIS2_PLACEMENT_3D ( 'NONE', #29961, #14917, #27278 ) ;
#17690 = CARTESIAN_POINT ( 'NONE',  ( -59.33507117675159748, -2.361427661686895885, 1.328119905389837152 ) ) ;
#17691 = DIRECTION ( 'NONE',  ( -7.637891338979715149E-45, -1.000000000000000000, -3.491481338843131383E-15 ) ) ;
#17692 = ORIENTED_EDGE ( 'NONE', *, *, #9300, .F. ) ;
#17693 = CARTESIAN_POINT ( 'NONE',  ( 51.70000000000002416, 3.851905453475163110, 1.404572667215161053 ) ) ;
#17694 = CARTESIAN_POINT ( 'NONE',  ( -35.85663232820592583, -2.686240680702151273, -4.475885388010727439 ) ) ;
#17695 = CARTESIAN_POINT ( 'NONE',  ( 54.28867365409860923, 5.640057820322912363, 1.624999999999810152 ) ) ;
#17696 = VERTEX_POINT ( 'NONE', #12119 ) ;
#17697 = DIRECTION ( 'NONE',  ( 0.000000000000000000, 0.000000000000000000, 1.000000000000000000 ) ) ;
#17698 = ORIENTED_EDGE ( 'NONE', *, *, #5546, .T. ) ;
#17699 = APPLICATION_CONTEXT ( 'automotive_design' ) ;
#17700 = CARTESIAN_POINT ( 'NONE',  ( 15.03925126672132784, -0.7747498368337625285, -5.363501452440939232 ) ) ;
#17701 = CARTESIAN_POINT ( 'NONE',  ( -55.40835481156723574, -0.8699069336946626541, 4.241846523238430144 ) ) ;
#17703 = CARTESIAN_POINT ( 'NONE',  ( 51.80000000000001137, -3.637377585518695611, -2.099877210783217762 ) ) ;
#17702 = DIRECTION ( 'NONE',  ( -1.000000000000000000, -4.678365685400771632E-16, -1.520093157366894206E-16 ) ) ;
#17704 = VERTEX_POINT ( 'NONE', #21174 ) ;
#17705 = CARTESIAN_POINT ( 'NONE',  ( -60.64999999999998437, -2.458515422985869670, -1.116110171506649040 ) ) ;
#17706 = PRODUCT_DEFINITION_FORMATION_WITH_SPECIFIED_SOURCE ( 'ANY', '', #20207, .NOT_KNOWN. ) ;
#17707 = AXIS2_PLACEMENT_3D ( 'NONE', #2666, #12303, #25434 ) ;
#17708 = EDGE_CURVE ( 'NONE', #10186, #29981, #13868, .T. ) ;
#17709 = CARTESIAN_POINT ( 'NONE',  ( 58.50000000000001421, 0.000000000000000000, 2.600000000000000089 ) ) ;
#17710 = CIRCLE ( 'NONE', #8581, 2.700000000000000178 ) ;
#17711 = VERTEX_POINT ( 'NONE', #2292 ) ;
#17713 = FACE_OUTER_BOUND ( 'NONE', #654, .T. ) ;
#17712 = CARTESIAN_POINT ( 'NONE',  ( 52.43776296160012862, 4.002620649804632613, 2.045778211737469210 ) ) ;
#17714 = CARTESIAN_POINT ( 'NONE',  ( 61.25000000000000000, 1.996089927834556965, -0.1249999999989956784 ) ) ;
#17715 = VERTEX_POINT ( 'NONE', #16725 ) ;
#17716 = CARTESIAN_POINT ( 'NONE',  ( -54.57202994616205416, -4.156921938165296204, -2.089175772356712570E-13 ) ) ;
#17717 = CARTESIAN_POINT ( 'NONE',  ( -56.15400635094608361, -3.399999999999987477, -0.9110272542660342587 ) ) ;
#17718 = CARTESIAN_POINT ( 'NONE',  ( 58.65844932252359456, 1.640171707773803167, -0.9087029769942892576 ) ) ;
#17719 = AXIS2_PLACEMENT_3D ( 'NONE', #15612, #1638, #17832 ) ;
#17720 = CARTESIAN_POINT ( 'NONE',  ( -74.39999999999997726, 1.249612330857415632, 0.03112912734226876837 ) ) ;
#17721 = DIRECTION ( 'NONE',  ( 0.000000000000000000, -1.000000000000000000, 0.000000000000000000 ) ) ;
#17722 = DIRECTION ( 'NONE',  ( -3.002035892788117459E-16, 0.9996898646859344595, 0.02490330187381124133 ) ) ;
#17723 = EDGE_LOOP ( 'NONE', ( #21298, #10860, #22705, #26270 ) ) ;
#17724 = EDGE_CURVE ( 'NONE', #5429, #30315, #1251, .T. ) ;
#17725 = AXIS2_PLACEMENT_3D ( 'NONE', #30947, #27938, #25725 ) ;
#17726 = CARTESIAN_POINT ( 'NONE',  ( 15.67083574136752944, -2.849134329833925783, 4.601168830303218549 ) ) ;
#17727 = CARTESIAN_POINT ( 'NONE',  ( -60.64959257988790853, -2.511140837076556220, 0.9920543200944375029 ) ) ;
#17728 = DIRECTION ( 'NONE',  ( -1.000000000000000000, -3.054025858079668409E-16, 2.042474015755241579E-16 ) ) ;
#17729 = EDGE_CURVE ( 'NONE', #11854, #30900, #21204, .T. ) ;
#17730 = CARTESIAN_POINT ( 'NONE',  ( -57.82202994616204705, 2.078460969082641885, 3.599999999999803801 ) ) ;
#17732 = AXIS2_PLACEMENT_3D ( 'NONE', #2605, #27284, #10043 ) ;
#17731 = CARTESIAN_POINT ( 'NONE',  ( -35.98952425903319607, 0.4576450703117207475, 5.200000005133905923 ) ) ;
#17733 = CYLINDRICAL_SURFACE ( 'NONE', #13971, 0.1000000000000000472 ) ;
#17734 = ORIENTED_EDGE ( 'NONE', *, *, #19332, .T. ) ;
#17735 = CARTESIAN_POINT ( 'NONE',  ( -35.85663232820584057, 0.9159215771349434876, -4.311190327366002606 ) ) ;
#17736 = ORIENTED_EDGE ( 'NONE', *, *, #7992, .T. ) ;
#17737 = PRODUCT_DEFINITION_CONTEXT ( 'detailed design', #31246, 'design' ) ;
#17738 = CARTESIAN_POINT ( 'NONE',  ( 50.49739899587713410, -0.9326869175216284669, 3.995127421239668575 ) ) ;
#17740 = CARTESIAN_POINT ( 'NONE',  ( 50.80000000000001847, -4.319730106884873244, -1.256953381662414770 ) ) ;
#17739 = CARTESIAN_POINT ( 'NONE',  ( 15.49676243306307910, -3.010474646410361110, -4.240315621469747498 ) ) ;
#17741 = VERTEX_POINT ( 'NONE', #11650 ) ;
#17742 = ORIENTED_EDGE ( 'NONE', *, *, #28982, .F. ) ;
#17743 = DIRECTION ( 'NONE',  ( -3.489354422748178582E-15, 1.218509414717996338E-16, -1.000000000000000000 ) ) ;
#17744 = ADVANCED_FACE ( 'NONE', ( #4823 ), #14171, .F. ) ;
#17745 = CARTESIAN_POINT ( 'NONE',  ( 30.51261366513615059, 7.487866468533194819, 1.424999999999893019 ) ) ;
#17746 = ORIENTED_EDGE ( 'NONE', *, *, #7528, .F. ) ;
#17748 = CARTESIAN_POINT ( 'NONE',  ( -59.19162505689493514, 2.404119360129248761, 1.250136525132548693 ) ) ;
#17747 = CARTESIAN_POINT ( 'NONE',  ( -57.82202994616206126, 2.078460969082646770, 3.599999999999802025 ) ) ;
#17749 = ADVANCED_FACE ( 'NONE', ( #21473 ), #8971, .F. ) ;
#17750 = DIRECTION ( 'NONE',  ( 0.000000000000000000, 0.000000000000000000, 1.000000000000000000 ) ) ;
#17751 = EDGE_CURVE ( 'NONE', #10732, #3631, #24906, .T. ) ;
#17752 = DIRECTION ( 'NONE',  ( -1.000000000000000000, -0.000000000000000000, 3.491481338843133355E-15 ) ) ;
#17753 = DIRECTION ( 'NONE',  ( 0.000000000000000000, 0.000000000000000000, 1.000000000000000000 ) ) ;
#17754 = CARTESIAN_POINT ( 'NONE',  ( -59.30000000000042348, -2.541725022351402963, -2.757196748647571027 ) ) ;
#17755 =( NAMED_UNIT ( * ) SI_UNIT ( $, .STERADIAN. ) SOLID_ANGLE_UNIT ( ) );
#17756 = VERTEX_POINT ( 'NONE', #10198 ) ;
#17757 = AXIS2_PLACEMENT_3D ( 'NONE', #26889, #24675, #13103 ) ;
#17758 = EDGE_CURVE ( 'NONE', #6720, #28184, #3784, .T. ) ;
#17759 = DIRECTION ( 'NONE',  ( 0.000000000000000000, -1.000000000000000000, -3.491481338843133355E-15 ) ) ;
#17760 = CARTESIAN_POINT ( 'NONE',  ( 51.80000000000001137, 8.600000000000108002, -1.950000000000180256 ) ) ;
#17761 = CARTESIAN_POINT ( 'NONE',  ( -56.39405989232412253, 2.944486372867110013, -1.700000000000180922 ) ) ;
#17762 = CARTESIAN_POINT ( 'NONE',  ( 15.74504787372188730, -0.2143423494566188969, 5.404929114625703690 ) ) ;
#17763 = CARTESIAN_POINT ( 'NONE',  ( 49.00000000000000000, -0.7500000000000000000, -1.988246715073871185 ) ) ;
#17765 = CARTESIAN_POINT ( 'NONE',  ( 58.65000038048068376, -1.830965513784331034, -0.4043111005671602420 ) ) ;
#17764 = CARTESIAN_POINT ( 'NONE',  ( 29.29107486424064177, 6.659593085418572755, -1.425000000000101963 ) ) ;
#17766 = ADVANCED_FACE ( 'NONE', ( #2615, #12407 ), #17327, .T. ) ;
#17767 = DIRECTION ( 'NONE',  ( 9.297243531610763781E-15, 0.000000000000000000, 1.000000000000000000 ) ) ;
#17768 = CARTESIAN_POINT ( 'NONE',  ( 58.75000000000002132, 6.153735859711025284E-13, 3.111507638930570854E-58 ) ) ;
#17770 = CARTESIAN_POINT ( 'NONE',  ( -59.69104130886936588, 2.078408370926939863, 1.734619616925012986 ) ) ;
#17769 = LINE ( 'NONE', #15543, #24609 ) ;
#17771 = ORIENTED_EDGE ( 'NONE', *, *, #21900, .F. ) ;
#17772 = CARTESIAN_POINT ( 'NONE',  ( 50.36610310744725183, -1.399562922973020429, -3.853849143137397792 ) ) ;
#17773 = EDGE_CURVE ( 'NONE', #30639, #29589, #10054, .T. ) ;
#17774 = CARTESIAN_POINT ( 'NONE',  ( 69.20000000000004547, 0.4500000000000000111, 1.988246715072634396 ) ) ;
#17776 = DIRECTION ( 'NONE',  ( -1.189524669241239263E-14, 0.000000000000000000, -1.000000000000000000 ) ) ;
#17775 = CARTESIAN_POINT ( 'NONE',  ( 15.22842924604220194, 2.525801262578962536, -4.794550356816757564 ) ) ;
#17777 = CARTESIAN_POINT ( 'NONE',  ( 58.75000000000002132, 6.153735859711025284E-13, 3.111507638930570854E-58 ) ) ;
#17778 = ORIENTED_EDGE ( 'NONE', *, *, #9024, .T. ) ;
#17779 = CYLINDRICAL_SURFACE ( 'NONE', #5384, 3.399999999999999911 ) ;
#17780 = CARTESIAN_POINT ( 'NONE',  ( -60.62613029541262222, -2.459964683042519695, -1.098852628973487233 ) ) ;
#17781 = ORIENTED_EDGE ( 'NONE', *, *, #24512, .T. ) ;
#17782 = EDGE_CURVE ( 'NONE', #28026, #6108, #19472, .T. ) ;
#17783 = CARTESIAN_POINT ( 'NONE',  ( 15.97944027357902463, -5.289443499204827148, 1.131445731060769955 ) ) ;
#17784 = ORIENTED_EDGE ( 'NONE', *, *, #26278, .T. ) ;
#17785 = VERTEX_POINT ( 'NONE', #7810 ) ;
#17786 = ADVANCED_FACE ( 'NONE', ( #17652 ), #17486, .F. ) ;
#17787 = DIRECTION ( 'NONE',  ( 0.000000000000000000, 0.000000000000000000, -1.000000000000000000 ) ) ;
#17788 = DIRECTION ( 'NONE',  ( 0.000000000000000000, -5.942513678379226626E-16, -1.000000000000000000 ) ) ;
#17789 = ORIENTED_EDGE ( 'NONE', *, *, #23641, .F. ) ;
#17790 = SHAPE_REPRESENTATION_RELATIONSHIP ( 'NONE' , 'NONE' ,  #9258, #27074 ) ;
#17791 = CARTESIAN_POINT ( 'NONE',  ( 52.01814763855281143, 4.368239464846260134, -1.441698456444288290 ) ) ;
#17792 = AXIS2_PLACEMENT_3D ( 'NONE', #30429, #18418, #28055 ) ;
#17793 = CARTESIAN_POINT ( 'NONE',  ( -59.94702994616205416, -2.078460969082657872, 3.599999999999778932 ) ) ;
#17794 = ORIENTED_EDGE ( 'NONE', *, *, #30078, .F. ) ;
#17795 = CARTESIAN_POINT ( 'NONE',  ( 50.59602332238209499, -0.1408342061598471806, -0.8215393206232035617 ) ) ;
#17796 = ORIENTED_EDGE ( 'NONE', *, *, #24105, .T. ) ;
#17797 = CARTESIAN_POINT ( 'NONE',  ( 50.40000000000001990, 2.428612866367529932E-14, -4.000000000000022204 ) ) ;
#17798 = CARTESIAN_POINT ( 'NONE',  ( 25.06719628372391639, 5.330953183979298515, 1.949999999999910916 ) ) ;
#17799 = ORIENTED_EDGE ( 'NONE', *, *, #22179, .T. ) ;
#17800 = CIRCLE ( 'NONE', #3109, 2.525000000000001243 ) ;
#17801 = CARTESIAN_POINT ( 'NONE',  ( 51.80000000000835314, -4.135416958146860722, -1.091811499727122881 ) ) ;
#17802 = DIRECTION ( 'NONE',  ( 0.000000000000000000, -0.9996898646859343485, -0.02490330187381124133 ) ) ;
#17803 = DIRECTION ( 'NONE',  ( 0.000000000000000000, 2.818925648462304271E-14, -1.000000000000000000 ) ) ;
#17804 = CARTESIAN_POINT ( 'NONE',  ( 56.96931127949304141, -0.7396072067343685275, -1.750137474527811321 ) ) ;
#17805 = DIRECTION ( 'NONE',  ( 1.000000000000000000, 0.000000000000000000, -1.047444401652940007E-14 ) ) ;
#17806 = B_SPLINE_CURVE_WITH_KNOTS ( 'NONE', 3,
 ( #7813, #26836, #27139, #24310 ),
 .UNSPECIFIED., .F., .F.,
 ( 4, 4 ),
 ( 0.000000000000000000, 0.0001493943817025111917 ),
 .UNSPECIFIED. ) ;
#17808 = DIRECTION ( 'NONE',  ( 2.581436205204234499E-16, -0.9796124928211140670, -0.2008964009354146651 ) ) ;
#17807 = CARTESIAN_POINT ( 'NONE',  ( -57.24986116251334778, 1.737685414808521678, -3.471684241605565546 ) ) ;
#17809 = ADVANCED_FACE ( 'NONE', ( #3073 ), #12261, .F. ) ;
#17810 = DIRECTION ( 'NONE',  ( 1.000000000000000000, -1.219044193948983948E-29, 3.491481338843133355E-15 ) ) ;
#17811 = EDGE_CURVE ( 'NONE', #15656, #10936, #22492, .T. ) ;
#17812 = CARTESIAN_POINT ( 'NONE',  ( -59.69999999999998153, 2.121207708687718352, 1.750136525132546472 ) ) ;
#17813 = CARTESIAN_POINT ( 'NONE',  ( 58.72204580543383656, 1.309860786662855325, -1.341784641882255436 ) ) ;
#17814 = CARTESIAN_POINT ( 'NONE',  ( 53.85175331755100814, 5.786643218348696216, 1.878002189130716149 ) ) ;
#17815 = ADVANCED_FACE ( 'NONE', ( #5610 ), #9745, .T. ) ;
#17816 = ORIENTED_EDGE ( 'NONE', *, *, #8253, .F. ) ;
#17817 = CARTESIAN_POINT ( 'NONE',  ( 51.88812122917388336, 8.998461838224887543, -1.950000000000180256 ) ) ;
#17818 = ORIENTED_EDGE ( 'NONE', *, *, #8253, .T. ) ;
#17819 = ORIENTED_EDGE ( 'NONE', *, *, #9349, .F. ) ;
#17820 = DIRECTION ( 'NONE',  ( 3.491481338843133355E-15, -0.000000000000000000, 1.000000000000000000 ) ) ;
#17821 = CARTESIAN_POINT ( 'NONE',  ( -59.29792740578359656, -2.256877952708263635, 2.542931754211925188 ) ) ;
#17823 = CARTESIAN_POINT ( 'NONE',  ( -59.60820241427157384, 2.215761459564569602, 1.591138442638788453 ) ) ;
#17822 = CARTESIAN_POINT ( 'NONE',  ( -55.37499999999996447, -2.944486372867076707, -1.700000000000207345 ) ) ;
#17824 = VERTEX_POINT ( 'NONE', #86 ) ;
#17825 = ORIENTED_EDGE ( 'NONE', *, *, #6537, .T. ) ;
#17826 = CARTESIAN_POINT ( 'NONE',  ( 53.91582462592152325, 6.672259099522126036, -1.774223561664970861 ) ) ;
#17827 = ORIENTED_EDGE ( 'NONE', *, *, #21006, .F. ) ;
#17828 = CARTESIAN_POINT ( 'NONE',  ( 51.77480685185290099, 3.850112906364226095, -1.502155480406633270 ) ) ;
#17829 = ORIENTED_EDGE ( 'NONE', *, *, #12706, .T. ) ;
#17830 = CARTESIAN_POINT ( 'NONE',  ( 26.92903764427389035, 5.249711979587993405, -1.950000000000161604 ) ) ;
#17831 =( BOUNDED_SURFACE ( )  B_SPLINE_SURFACE ( 1, 2, ( 
 ( #13393, #27839, #15175, #25300, #3298, #8662, #20265, #29894, #24827, #12784, #18030, #13247, #22462, #758, #10421, #20414, #20104, #29738, #30036, #5831, #8055, #17873, #27364, #27507, #8351, #21506, #13567, #9307, #26241, #14199, #4225, #25920, #19139, #31141, #2165, #6293, #15942, #20874, #4552, #28307, #6464, #23874, #3925, #16275, #9473, #14037, #8807, #25602, #23724, #21030, #23254, #4079, #11828, #16422, #28617, #1541, #9154, #13719, #28460, #6933, #23402, #23553, #11201, #26076, #2016, #18815, #21359, #30501, #6763, #16120, #11681, #28139, #1684, #16599, #18496, #4388, #30985, #25770, #18970, #11345, #13863, #30670, #8985, #1854, #6613, #18658, #11527, #21203, #30836, #569, #12596, #4696, #421, #17354, #5307, #26723, #17067, #10227, #22281, #24637, #28778, #7091, #11993, #27000, #19435, #28925, #14968, #26396, #7389 ),
 ( #21678, #7237, #16901, #259, #31301, #22129, #29081, #29384, #2785, #14812, #7696, #19755, #5013, #14674, #5163, #26544, #17215, #24334, #4851, #2641, #12436, #14518, #12283, #21970, #9633, #26857, #9923, #19603, #2951, #29241, #2493, #16753, #24186, #7555, #2326, #24474, #10079, #19290, #14350, #24020, #12148, #21826, #114, #9770, #27324, #891, #29525, #20225, #29853, #8167, #13358, #24791, #17985, #5482, #17836, #27634, #20059, #22588, #15617, #1045, #25258, #25096, #27470, #3577, #5790, #12749, #19896, #22897, #23050, #1342, #15445, #22749, #30000, #24935, #10695, #8313, #30161, #5963, #6111, #13215, #1186, #22425, #10843, #15134, #17681, #3098, #20378, #20528, #5636, #10548, #7839, #3428, #13066, #8480, #17515, #717, #18161, #10377, #27798, #15762, #29696, #25412, #3715, #27170, #8016, #15287, #3257, #12899, #28265 ) ),
 .UNSPECIFIED., .F., .F., .F. ) 
 B_SPLINE_SURFACE_WITH_KNOTS ( ( 2, 2 ),
 ( 3, 2, 2, 2, 2, 2, 2, 2, 2, 2, 2, 2, 2, 2, 2, 2, 2, 2, 2, 2, 2, 2, 2, 2, 2, 2, 2, 2, 2, 2, 2, 2, 2, 2, 2, 2, 2, 2, 2, 2, 2, 2, 2, 2, 2, 2, 2, 2, 2, 2, 2, 2, 2, 2, 3 ),
 ( 0.000000000000000000, 1.000000000000000000 ),
 ( 0.000000000000000000, 0.01851851851851851749, 0.03703703703703703498, 0.05555555555555555247, 0.07407407407407406996, 0.09259259259259258745, 0.1111111111111111049, 0.1296296296296296224, 0.1481481481481481399, 0.1666666666666666574, 0.1851851851851851749, 0.2037037037037036924, 0.2222222222222222099, 0.2407407407407407274, 0.2592592592592592449, 0.2777777777777777901, 0.2962962962962962798, 0.3148148148148148251, 0.3333333333333333148, 0.3518518518518518601, 0.3703703703703703498, 0.3888888888888888951, 0.4074074074074073848, 0.4259259259259259300, 0.4444444444444444198, 0.4629629629629629650, 0.4814814814814814548, 0.5000000000000000000, 0.5185185185185184897, 0.5370370370370370905, 0.5555555555555555802, 0.5740740740740740700, 0.5925925925925925597, 0.6111111111111111605, 0.6296296296296296502, 0.6481481481481481399, 0.6666666666666666297, 0.6851851851851852304, 0.7037037037037037202, 0.7222222222222222099, 0.7407407407407406996, 0.7592592592592593004, 0.7777777777777777901, 0.7962962962962962798, 0.8148148148148147696, 0.8333333333333333703, 0.8518518518518518601, 0.8703703703703703498, 0.8888888888888888395, 0.9074074074074074403, 0.9259259259259259300, 0.9444444444444444198, 0.9629629629629629095, 0.9814814814814815103, 1.000000000000000000 ),
 .UNSPECIFIED. ) 
 GEOMETRIC_REPRESENTATION_ITEM ( )  RATIONAL_B_SPLINE_SURFACE ( (
 ( 1.000000000000000000, 0.8660254037844387076, 1.000000000000000000, 0.8660254037844387076, 1.000000000000000000, 0.8660254037844387076, 1.000000000000000000, 0.8660254037844387076, 1.000000000000000000, 0.8660254037844387076, 1.000000000000000000, 0.8660254037844387076, 1.000000000000000000, 0.8660254037844387076, 1.000000000000000000, 0.8660254037844387076, 1.000000000000000000, 0.8660254037844387076, 1.000000000000000000, 0.8660254037844387076, 1.000000000000000000, 0.8660254037844387076, 1.000000000000000000, 0.8660254037844387076, 1.000000000000000000, 0.8660254037844387076, 1.000000000000000000, 0.8660254037844387076, 1.000000000000000000, 0.8660254037844387076, 1.000000000000000000, 0.8660254037844387076, 1.000000000000000000, 0.8660254037844387076, 1.000000000000000000, 0.8660254037844387076, 1.000000000000000000, 0.8660254037844387076, 1.000000000000000000, 0.8660254037844387076, 1.000000000000000000, 0.8660254037844387076, 1.000000000000000000, 0.8660254037844387076, 1.000000000000000000, 0.8660254037844387076, 1.000000000000000000, 0.8660254037844387076, 1.000000000000000000, 0.8660254037844387076, 1.000000000000000000, 0.8660254037844387076, 1.000000000000000000, 0.8660254037844387076, 1.000000000000000000, 0.8660254037844387076, 1.000000000000000000, 0.8660254037844387076, 1.000000000000000000, 0.8660254037844387076, 1.000000000000000000, 0.8660254037844387076, 1.000000000000000000, 0.8660254037844387076, 1.000000000000000000, 0.8660254037844387076, 1.000000000000000000, 0.8660254037844387076, 1.000000000000000000, 0.8660254037844387076, 1.000000000000000000, 0.8660254037844387076, 1.000000000000000000, 0.8660254037844387076, 1.000000000000000000, 0.8660254037844387076, 1.000000000000000000, 0.8660254037844387076, 1.000000000000000000, 0.8660254037844387076, 1.000000000000000000, 0.8660254037844387076, 1.000000000000000000, 0.8660254037844387076, 1.000000000000000000, 0.8660254037844387076, 1.000000000000000000, 0.8660254037844387076, 1.000000000000000000, 0.8660254037844387076, 1.000000000000000000, 0.8660254037844387076, 1.000000000000000000, 0.8660254037844387076, 1.000000000000000000, 0.8660254037844387076, 1.000000000000000000, 0.8660254037844387076, 1.000000000000000000, 0.8660254037844387076, 1.000000000000000000, 0.8660254037844387076, 1.000000000000000000, 0.8660254037844387076, 1.000000000000000000, 0.8660254037844387076, 1.000000000000000000, 0.8660254037844387076, 1.000000000000000000),
 ( 1.000000000000000000, 0.8660254037844387076, 1.000000000000000000, 0.8660254037844387076, 1.000000000000000000, 0.8660254037844387076, 1.000000000000000000, 0.8660254037844387076, 1.000000000000000000, 0.8660254037844387076, 1.000000000000000000, 0.8660254037844387076, 1.000000000000000000, 0.8660254037844387076, 1.000000000000000000, 0.8660254037844387076, 1.000000000000000000, 0.8660254037844387076, 1.000000000000000000, 0.8660254037844387076, 1.000000000000000000, 0.8660254037844387076, 1.000000000000000000, 0.8660254037844387076, 1.000000000000000000, 0.8660254037844387076, 1.000000000000000000, 0.8660254037844387076, 1.000000000000000000, 0.8660254037844387076, 1.000000000000000000, 0.8660254037844387076, 1.000000000000000000, 0.8660254037844387076, 1.000000000000000000, 0.8660254037844387076, 1.000000000000000000, 0.8660254037844387076, 1.000000000000000000, 0.8660254037844387076, 1.000000000000000000, 0.8660254037844387076, 1.000000000000000000, 0.8660254037844387076, 1.000000000000000000, 0.8660254037844387076, 1.000000000000000000, 0.8660254037844387076, 1.000000000000000000, 0.8660254037844387076, 1.000000000000000000, 0.8660254037844387076, 1.000000000000000000, 0.8660254037844387076, 1.000000000000000000, 0.8660254037844387076, 1.000000000000000000, 0.8660254037844387076, 1.000000000000000000, 0.8660254037844387076, 1.000000000000000000, 0.8660254037844387076, 1.000000000000000000, 0.8660254037844387076, 1.000000000000000000, 0.8660254037844387076, 1.000000000000000000, 0.8660254037844387076, 1.000000000000000000, 0.8660254037844387076, 1.000000000000000000, 0.8660254037844387076, 1.000000000000000000, 0.8660254037844387076, 1.000000000000000000, 0.8660254037844387076, 1.000000000000000000, 0.8660254037844387076, 1.000000000000000000, 0.8660254037844387076, 1.000000000000000000, 0.8660254037844387076, 1.000000000000000000, 0.8660254037844387076, 1.000000000000000000, 0.8660254037844387076, 1.000000000000000000, 0.8660254037844387076, 1.000000000000000000, 0.8660254037844387076, 1.000000000000000000, 0.8660254037844387076, 1.000000000000000000, 0.8660254037844387076, 1.000000000000000000, 0.8660254037844387076, 1.000000000000000000, 0.8660254037844387076, 1.000000000000000000, 0.8660254037844387076, 1.000000000000000000, 0.8660254037844387076, 1.000000000000000000, 0.8660254037844387076, 1.000000000000000000, 0.8660254037844387076, 1.000000000000000000, 0.8660254037844387076, 1.000000000000000000) ) ) 
 REPRESENTATION_ITEM ( '' )  SURFACE ( )  );
#17832 = DIRECTION ( 'NONE',  ( 0.000000000000000000, -0.9996898646859344595, -0.02490330187381133153 ) ) ;
#17833 = LINE ( 'NONE', #24632, #9642 ) ;
#17834 = ORIENTED_EDGE ( 'NONE', *, *, #10121, .T. ) ;
#17835 = CARTESIAN_POINT ( 'NONE',  ( 15.17214319754844887, -4.804073785499189064, -2.042134698606595133 ) ) ;
#17836 = CARTESIAN_POINT ( 'NONE',  ( -57.64405989232413674, -3.920666489018320690E-15, 3.399999999999794298 ) ) ;
#17837 = CARTESIAN_POINT ( 'NONE',  ( 58.75000000000002132, 6.153735859711025284E-13, 3.111507638930570854E-58 ) ) ;
#17838 = CARTESIAN_POINT ( 'NONE',  ( 47.00000000000000711, -3.550773357292059007, -2.049880134335985371 ) ) ;
#17839 = CARTESIAN_POINT ( 'NONE',  ( -44.59999999999998010, 8.366749974758271452E-15, -1.593320673368357319E-13 ) ) ;
#17840 = DIRECTION ( 'NONE',  ( 1.000000000000000000, 1.047444401652940007E-14, 0.000000000000000000 ) ) ;
#17842 = CARTESIAN_POINT ( 'NONE',  ( 51.60243094284678023, -4.191177329985464439, 1.624749424009206411 ) ) ;
#17841 = CARTESIAN_POINT ( 'NONE',  ( -59.43714858239737708, 3.292580442886323233, 1.294864515003326444 ) ) ;
#17843 = CARTESIAN_POINT ( 'NONE',  ( -58.78335481156722864, 0.7533615035077975142, -3.673546848079180638 ) ) ;
#17844 = ADVANCED_FACE ( 'NONE', ( #19407 ), #29049, .F. ) ;
#17845 = CARTESIAN_POINT ( 'NONE',  ( 57.05000000000001847, -0.7500000000000000000, 1.778341924377873751 ) ) ;
#17846 = CARTESIAN_POINT ( 'NONE',  ( 51.31757909864148104, -1.004435980685438157, 1.391945786376508343 ) ) ;
#17847 = AXIS2_PLACEMENT_3D ( 'NONE', #28903, #233, #9895 ) ;
#17848 = ORIENTED_EDGE ( 'NONE', *, *, #13737, .T. ) ;
#17849 = DIRECTION ( 'NONE',  ( 9.329605248950888974E-15, -1.000000000000000000, 0.000000000000000000 ) ) ;
#17850 = CARTESIAN_POINT ( 'NONE',  ( 54.36194271933292299, 6.362460388746521645, 2.049999999999810196 ) ) ;
#17851 = ORIENTED_EDGE ( 'NONE', *, *, #17396, .F. ) ;
#17852 = DIRECTION ( 'NONE',  ( 2.471142467734912792E-12, -0.3099561728516428416, -0.9507508458640269167 ) ) ;
#17853 = EDGE_LOOP ( 'NONE', ( #4467, #7198, #19162, #5980 ) ) ;
#17854 = CARTESIAN_POINT ( 'NONE',  ( 51.78416995154975666, -0.8999235898776962728, 1.360374659026170496 ) ) ;
#17855 = CARTESIAN_POINT ( 'NONE',  ( -59.18749999999995737, -3.399999999999991029, -2.288065396424332102E-13 ) ) ;
#17857 = CARTESIAN_POINT ( 'NONE',  ( -59.69999999999997442, 3.400000000000007905, -2.001823990013003858E-13 ) ) ;
#17856 = CARTESIAN_POINT ( 'NONE',  ( 61.25000000000003553, -0.8813478542982779995, 1.623476567772350387 ) ) ;
#17858 = ORIENTED_EDGE ( 'NONE', *, *, #23017, .T. ) ;
#17859 = DIRECTION ( 'NONE',  ( 2.581436205204234006E-16, -0.9796124928211140670, -0.2008964009354148872 ) ) ;
#17860 = EDGE_CURVE ( 'NONE', #12058, #27852, #4988, .T. ) ;
#17861 = CARTESIAN_POINT ( 'NONE',  ( 57.03577985506672832, -0.7479400494557524315, -1.780189605359982608 ) ) ;
#17862 = ORIENTED_EDGE ( 'NONE', *, *, #27443, .F. ) ;
#17864 = CARTESIAN_POINT ( 'NONE',  ( 34.56702326949725546, 8.213851659285209550, 1.549999999999879696 ) ) ;
#17863 = FACE_OUTER_BOUND ( 'NONE', #23581, .T. ) ;
#17865 = FACE_OUTER_BOUND ( 'NONE', #31102, .T. ) ;
#17866 = EDGE_LOOP ( 'NONE', ( #30871, #30144, #28069, #3456 ) ) ;
#17867 = DIRECTION ( 'NONE',  ( 1.000000000000000000, 0.000000000000000000, -3.491481338843133750E-15 ) ) ;
#17868 = CARTESIAN_POINT ( 'NONE',  ( 56.98303665332567647, -0.7553445069156616842, 1.743428900644034885 ) ) ;
#17869 = CARTESIAN_POINT ( 'NONE',  ( -54.76905989232412963, 2.944486372867092250, 1.699999999999816769 ) ) ;
#17870 =( LENGTH_UNIT ( ) NAMED_UNIT ( * ) SI_UNIT ( .MILLI., .METRE. ) );
#17871 = DIRECTION ( 'NONE',  ( -1.000000000000000000, -1.047444401652940007E-14, -0.000000000000000000 ) ) ;
#17873 = CARTESIAN_POINT ( 'NONE',  ( -55.69702994616204705, 4.156921938165313080, -1.827997107644302771E-13 ) ) ;
#17872 = VECTOR ( 'NONE', #21258, 999.9999999999998863 ) ;
#17874 = EDGE_LOOP ( 'NONE', ( #18473, #2637 ) ) ;
#17875 = DIRECTION ( 'NONE',  ( -1.000000000000000000, 1.219044193948983948E-29, -3.491481338843133355E-15 ) ) ;
#17876 = CARTESIAN_POINT ( 'NONE',  ( -54.54792740578361077, -1.073804522883516688, -3.225979517392336238 ) ) ;
#17877 = EDGE_CURVE ( 'NONE', #30656, #5143, #24306, .T. ) ;
#17878 = CARTESIAN_POINT ( 'NONE',  ( -58.20655989232411542, -3.399999999999991029, -2.246812820714294660E-13 ) ) ;
#17879 = ADVANCED_FACE ( 'NONE', ( #21946 ), #16939, .F. ) ;
#17880 = CARTESIAN_POINT ( 'NONE',  ( -57.07202994616206126, 2.078460969082642773, 3.599999999999806022 ) ) ;
#17881 = CARTESIAN_POINT ( 'NONE',  ( 47.05963571244990362, 8.266527678078146479, -2.050000000000163691 ) ) ;
#17882 = CARTESIAN_POINT ( 'NONE',  ( 22.40781231897555870, 7.073106863806386535, 2.049999999999922107 ) ) ;
#17883 = VERTEX_POINT ( 'NONE', #5135 ) ;
#17884 = CYLINDRICAL_SURFACE ( 'NONE', #11805, 0.4600000000000000755 ) ;
#17885 = VERTEX_POINT ( 'NONE', #14789 ) ;
#17886 = CARTESIAN_POINT ( 'NONE',  ( 52.06628335902946247, -0.5434431642975682264, 1.794517909405659806 ) ) ;
#17887 = VECTOR ( 'NONE', #16882, 1000.000000000000000 ) ;
#17889 = FACE_OUTER_BOUND ( 'NONE', #26628, .T. ) ;
#17888 = CARTESIAN_POINT ( 'NONE',  ( 56.95000000000001705, -0.6999999999999999556, 2.452039967047845437 ) ) ;
#17890 = ORIENTED_EDGE ( 'NONE', *, *, #6018, .T. ) ;
#17891 = ORIENTED_EDGE ( 'NONE', *, *, #2967, .T. ) ;
#17892 = FACE_OUTER_BOUND ( 'NONE', #22656, .T. ) ;
#17893 = FACE_OUTER_BOUND ( 'NONE', #29927, .T. ) ;
#17894 = ORIENTED_EDGE ( 'NONE', *, *, #6956, .T. ) ;
#17896 = DIRECTION ( 'NONE',  ( -0.03489949670247565611, -0.9993908270190966503, 0.000000000000000000 ) ) ;
#17895 = CARTESIAN_POINT ( 'NONE',  ( -59.32202994616204705, 2.078460969082646770, 3.599999999999797140 ) ) ;
#17897 = CARTESIAN_POINT ( 'NONE',  ( -57.36042740578360366, 3.725040285533370632, -1.239922660687675871 ) ) ;
#17898 = CARTESIAN_POINT ( 'NONE',  ( -57.22499999999997300, -0.8236752438351979677, 4.016411220566568296 ) ) ;
#17899 = DIRECTION ( 'NONE',  ( 0.000000000000000000, 0.000000000000000000, 1.000000000000000000 ) ) ;
#17900 = CARTESIAN_POINT ( 'NONE',  ( -59.29999999999999716, -3.581647374645368309, -0.5069159045576940859 ) ) ;
#17901 = EDGE_CURVE ( 'NONE', #2745, #3817, #20981, .T. ) ;
#17902 = VERTEX_POINT ( 'NONE', #22552 ) ;
#17903 = CARTESIAN_POINT ( 'NONE',  ( 47.06312566212017146, 8.366466760780054912, 1.949999999999835865 ) ) ;
#17904 = CARTESIAN_POINT ( 'NONE',  ( 53.71283936284424954, 7.813984279442741432, -2.050000000000187228 ) ) ;
#17905 = DIRECTION ( 'NONE',  ( 1.000000000000000000, 3.054025858079668409E-16, -2.042474015755241579E-16 ) ) ;
#17906 = AXIS2_PLACEMENT_3D ( 'NONE', #26776, #26304, #23932 ) ;
#17907 = CARTESIAN_POINT ( 'NONE',  ( 16.07279755198631932, -0.3252614978954516678, 5.399488438498854848 ) ) ;
#17908 = CARTESIAN_POINT ( 'NONE',  ( 57.04126813003668417, -0.7492316407094400388, -2.421767203557310122 ) ) ;
#17909 = ADVANCED_FACE ( 'NONE', ( #10976 ), #3843, .T. ) ;
#17911 = CARTESIAN_POINT ( 'NONE',  ( -35.85663232820592583, 0.4576450603546802776, -5.200000000000000178 ) ) ;
#17910 = CARTESIAN_POINT ( 'NONE',  ( -56.74999999999995737, 2.273606599708567113E-14, -3.400000000000201972 ) ) ;
#17912 = ADVANCED_FACE ( 'NONE', ( #12868 ), #14409, .T. ) ;
#17913 = EDGE_CURVE ( 'NONE', #29917, #11630, #27535, .T. ) ;
#17914 = CIRCLE ( 'NONE', #2749, 1.474417381223824153 ) ;
#17915 = CARTESIAN_POINT ( 'NONE',  ( 69.01464466094070360, 4.557543281186736018E-17, -7.228900318216929560E-13 ) ) ;
#17916 = CARTESIAN_POINT ( 'NONE',  ( 17.21035195517768557, -2.471857751707525626E-15, 0.000000000000000000 ) ) ;
#17918 = CARTESIAN_POINT ( 'NONE',  ( -54.49999999999998579, 3.724034196517557405, 0.2473046399340681489 ) ) ;
#17917 = CARTESIAN_POINT ( 'NONE',  ( -59.23418654921033522, -3.153953023162030078, 1.269874138521803975 ) ) ;
#17919 = EDGE_LOOP ( 'NONE', ( #7425, #6286, #3955, #20437 ) ) ;
#17920 = CARTESIAN_POINT ( 'NONE',  ( -73.85208152723558328, -1.351577301140755472, -0.03366917953766473959 ) ) ;
#17921 = CARTESIAN_POINT ( 'NONE',  ( -54.49999999999999289, 1.399999999999995914, 3.959797974644419849 ) ) ;
#17923 = DIRECTION ( 'NONE',  ( 1.189524669241239263E-14, 0.000000000000000000, 1.000000000000000000 ) ) ;
#17922 = CARTESIAN_POINT ( 'NONE',  ( 15.03925126672132961, 2.686240680702205008, -4.475885388010691912 ) ) ;
#17924 = CARTESIAN_POINT ( 'NONE',  ( 58.75000000000002842, -0.8948927608041769011, 1.760622601996005177 ) ) ;
#17925 = ORIENTED_EDGE ( 'NONE', *, *, #23146, .T. ) ;
#17926 = CARTESIAN_POINT ( 'NONE',  ( 52.72388909185001893, 4.000582417204455510, 2.049999999999815969 ) ) ;
#17927 = CARTESIAN_POINT ( 'NONE',  ( 47.02229336006145388, -4.163003037071927537, 1.036150823695777934 ) ) ;
#17928 = AXIS2_PLACEMENT_3D ( 'NONE', #3295, #25139, #27205 ) ;
#17929 = ADVANCED_FACE ( 'NONE', ( #11128 ), #854, .T. ) ;
#17930 = ORIENTED_EDGE ( 'NONE', *, *, #2864, .T. ) ;
#17931 = CARTESIAN_POINT ( 'NONE',  ( 48.30000000000001847, 2.428612866367529932E-14, 0.000000000000000000 ) ) ;
#17932 = ORIENTED_EDGE ( 'NONE', *, *, #16717, .T. ) ;
#17933 = CARTESIAN_POINT ( 'NONE',  ( 54.19386703870443966, 5.671865141453451109, 2.049999999999810640 ) ) ;
#17934 = CARTESIAN_POINT ( 'NONE',  ( 58.65000000000000568, 1.656314228059722282, -0.8794134543718038488 ) ) ;
#17935 = ORIENTED_EDGE ( 'NONE', *, *, #17185, .T. ) ;
#17936 = DIRECTION ( 'NONE',  ( 0.000000000000000000, 0.000000000000000000, -1.000000000000000000 ) ) ;
#17937 = CARTESIAN_POINT ( 'NONE',  ( -59.38452994616203995, 3.117691453623979481, 1.799999999999801092 ) ) ;
#17938 = VERTEX_POINT ( 'NONE', #15874 ) ;
#17939 = DIRECTION ( 'NONE',  ( -1.000000000000000000, 0.000000000000000000, -3.491481338842906952E-15 ) ) ;
#17940 = DIRECTION ( 'NONE',  ( 1.520093157366863638E-16, -0.5877852522924685852, -0.8090169943749507819 ) ) ;
#17941 = ADVANCED_FACE ( 'NONE', ( #13323 ), #20660, .F. ) ;
#17942 = CARTESIAN_POINT ( 'NONE',  ( 22.18976255005305021, 7.481058471421467182, 2.049999999999922551 ) ) ;
#17943 = VERTEX_POINT ( 'NONE', #8135 ) ;
#17944 = CARTESIAN_POINT ( 'NONE',  ( -58.24999999999995737, 2.023778652682509052E-14, -3.400000000000207301 ) ) ;
#17945 = CARTESIAN_POINT ( 'NONE',  ( -57.34599364905385954, 0.2309624077929011976, 3.875409454552789956 ) ) ;
#17946 = CYLINDRICAL_SURFACE ( 'NONE', #89, 3.750000000000000444 ) ;
#17947 = CARTESIAN_POINT ( 'NONE',  ( 57.03951379057714632, -0.7794871794871794934, -1.732743413496389939 ) ) ;
#17948 = AXIS2_PLACEMENT_3D ( 'NONE', #22265, #17820, #27456 ) ;
#17949 = CARTESIAN_POINT ( 'NONE',  ( 68.05000000000006821, 1.401298464324817071E-42, 3.949999999999287414 ) ) ;
#17950 = ADVANCED_FACE ( 'NONE', ( #1308 ), #30285, .T. ) ;
#17952 = DIRECTION ( 'NONE',  ( -1.000000000000000000, -0.000000000000000000, 3.491481338843133355E-15 ) ) ;
#17951 = DIRECTION ( 'NONE',  ( 1.000000000000000000, 1.047444401652940007E-14, 0.000000000000000000 ) ) ;
#17953 = EDGE_CURVE ( 'NONE', #28678, #8829, #6381, .T. ) ;
#17954 = AXIS2_PLACEMENT_3D ( 'NONE', #21346, #9621, #30975 ) ;
#17955 = EDGE_CURVE ( 'NONE', #18759, #1827, #7321, .T. ) ;
#17956 = DIRECTION ( 'NONE',  ( -1.000000000000000000, -0.000000000000000000, 0.000000000000000000 ) ) ;
#17957 = CARTESIAN_POINT ( 'NONE',  ( -59.69934827995219706, 2.105468426063201282, 1.749007712897468814 ) ) ;
#17958 = CARTESIAN_POINT ( 'NONE',  ( 58.74999981196283727, 1.441661833136088866, -1.321459237640081330 ) ) ;
#17959 = DIRECTION ( 'NONE',  ( -1.000000000000000000, -3.054025858079668409E-16, 2.042474015755241579E-16 ) ) ;
#17960 = TOROIDAL_SURFACE ( 'NONE', #29558, 0.3000000000000000444, 0.05000000000000000278 ) ;
#17961 = ORIENTED_EDGE ( 'NONE', *, *, #14412, .F. ) ;
#17962 = CARTESIAN_POINT ( 'NONE',  ( 47.00000000000002132, -1.426739617975173013, -3.843750000000023093 ) ) ;
#17963 = VERTEX_POINT ( 'NONE', #30122 ) ;
#17964 = ORIENTED_EDGE ( 'NONE', *, *, #8547, .T. ) ;
#17965 = CARTESIAN_POINT ( 'NONE',  ( -67.89999999999997726, -6.032153844857049047E-16, 3.382382808457892732E-15 ) ) ;
#17966 = CARTESIAN_POINT ( 'NONE',  ( -58.42292740578360366, -3.330682475591783653, -0.6830477631804107164 ) ) ;
#17968 = DIRECTION ( 'NONE',  ( 1.000000000000000000, -0.000000000000000000, -0.000000000000000000 ) ) ;
#17967 = CARTESIAN_POINT ( 'NONE',  ( -58.24999999999995737, 2.023778652682509052E-14, -3.400000000000207301 ) ) ;
#17969 = ORIENTED_EDGE ( 'NONE', *, *, #15115, .T. ) ;
#17970 = EDGE_LOOP ( 'NONE', ( #2707, #30844, #9211, #12934 ) ) ;
#17971 = AXIS2_PLACEMENT_3D ( 'NONE', #26128, #18860, #4441 ) ;
#17972 = DIRECTION ( 'NONE',  ( 0.000000000000000000, 0.9507508458636236837, 0.3099561728528797966 ) ) ;
#17973 = ORIENTED_EDGE ( 'NONE', *, *, #17913, .F. ) ;
#17974 = VECTOR ( 'NONE', #15375, 1000.000000000000000 ) ;
#17975 = CARTESIAN_POINT ( 'NONE',  ( 47.00000000000002132, 6.982261990806648555E-14, -1.628983268085978048E-13 ) ) ;
#17976 = ORIENTED_EDGE ( 'NONE', *, *, #20650, .T. ) ;
#17977 = FACE_OUTER_BOUND ( 'NONE', #22628, .T. ) ;
#17978 = FACE_OUTER_BOUND ( 'NONE', #2944, .T. ) ;
#17979 = ADVANCED_FACE ( 'NONE', ( #23184, #5758 ), #13040, .T. ) ;
#17980 = CARTESIAN_POINT ( 'NONE',  ( 58.45000000000001705, 0.7794871794871796045, -1.732743413496389939 ) ) ;
#17981 = CIRCLE ( 'NONE', #22037, 0.2500000000000000555 ) ;
#17982 = CARTESIAN_POINT ( 'NONE',  ( 47.04711921876768344, -4.174487749534351089, -1.011178756798956524 ) ) ;
#17983 = AXIS2_PLACEMENT_3D ( 'NONE', #13592, #27865, #22963 ) ;
#17984 = EDGE_CURVE ( 'NONE', #22862, #18443, #26177, .T. ) ;
#17985 = CARTESIAN_POINT ( 'NONE',  ( -57.51905989232412963, -2.944486372867088697, 1.699999999999784350 ) ) ;
#17986 = CARTESIAN_POINT ( 'NONE',  ( -57.69184846062113081, 0.2309624077929080255, 3.875409454552792177 ) ) ;
#17987 = CARTESIAN_POINT ( 'NONE',  ( 47.19764788914726239, -3.901663320877392760, -1.540393549661939865 ) ) ;
#17988 = CARTESIAN_POINT ( 'NONE',  ( 48.41852494697948828, 1.153996415704716449, 3.890257736381618869 ) ) ;
#17989 = CARTESIAN_POINT ( 'NONE',  ( 49.00000000000000000, 0.6617647058823536987, -1.754335336829947467 ) ) ;
#17991 = CARTESIAN_POINT ( 'NONE',  ( 51.03825729975065428, -4.379902212273306006, 1.406632791261188897 ) ) ;
#17990 = CARTESIAN_POINT ( 'NONE',  ( 47.10000000000002274, -3.826179070414207573, 1.000000000000000222 ) ) ;
#17992 = AXIS2_PLACEMENT_3D ( 'NONE', #18651, #15647, #3604 ) ;
#17993 = EDGE_CURVE ( 'NONE', #19884, #25169, #1742, .T. ) ;
#17994 = VECTOR ( 'NONE', #2382, 1000.000000000000000 ) ;
#17995 = CARTESIAN_POINT ( 'NONE',  ( -54.39999999999997726, -1.399999999999992806, -1.984366583318788002E-13 ) ) ;
#17996 = TOROIDAL_SURFACE ( 'NONE', #4329, 0.2000000000000000111, 0.1000000000000000056 ) ;
#17997 = CARTESIAN_POINT ( 'NONE',  ( 67.94999999999998863, 4.959819536545755081E-16, -4.050000000000713030 ) ) ;
#17998 = CARTESIAN_POINT ( 'NONE',  ( 51.45655683570191741, -0.9591657938390837357, 1.468576096419531574 ) ) ;
#17999 = ORIENTED_EDGE ( 'NONE', *, *, #119, .F. ) ;
#18000 = CARTESIAN_POINT ( 'NONE',  ( 50.25000000000002842, -0.8897917884445627479, 1.791164585743103999 ) ) ;
#18001 = CARTESIAN_POINT ( 'NONE',  ( 54.16352682579100986, 5.682044187412361502, 2.049999999999811084 ) ) ;
#18002 = CIRCLE ( 'NONE', #10425, 4.275000000000000355 ) ;
#18003 = ORIENTED_EDGE ( 'NONE', *, *, #26514, .T. ) ;
#18004 = DIRECTION ( 'NONE',  ( 0.000000000000000000, 0.000000000000000000, 1.000000000000000000 ) ) ;
#18005 = ORIENTED_EDGE ( 'NONE', *, *, #24815, .T. ) ;
#18006 = VECTOR ( 'NONE', #756, 1000.000000000000000 ) ;
#18007 =( BOUNDED_SURFACE ( )  B_SPLINE_SURFACE ( 3, 2, ( 
 ( #1472, #23480, #4008 ),
 ( #18900, #21294, #1952 ),
 ( #15737, #20664, #26003 ),
 ( #6231, #4312, #3690 ),
 ( #9241, #13796, #8601 ),
 ( #1773, #20807, #6085 ),
 ( #13961, #16207, #28392 ),
 ( #8903, #3849, #28238 ),
 ( #13498, #23334, #23660 ),
 ( #11448, #25855, #18428 ) ),
 .UNSPECIFIED., .F., .F., .F. ) 
 B_SPLINE_SURFACE_WITH_KNOTS ( ( 4, 2, 2, 2, 4 ),
 ( 3, 3 ),
 ( 0.0001706658715699256265, 0.0002229276920781272985, 0.0002751895125863289705, 0.0003274513330945306154, 0.0003797131536027322602 ),
 ( 0.000000000000000000, 1.000000000000000000 ),
 .UNSPECIFIED. ) 
 GEOMETRIC_REPRESENTATION_ITEM ( )  RATIONAL_B_SPLINE_SURFACE ( (
 ( 1.000000000000000000, 0.7071067811873685827, 1.000000000000000000),
 ( 1.000000000000000000, 0.7375607040707305995, 1.000000000000000000),
 ( 1.000000000000000000, 0.7730431127433396998, 1.000000000000000000),
 ( 1.000000000000000000, 0.8321012486978203171, 1.000000000000000000),
 ( 1.000000000000000000, 0.8541932017396182131, 1.000000000000000000),
 ( 1.000000000000000000, 0.8545723906043213303, 1.000000000000000000),
 ( 1.000000000000000000, 0.8327032135035172811, 1.000000000000000000),
 ( 1.000000000000000000, 0.7734559727056840028, 1.000000000000000000),
 ( 1.000000000000000000, 0.7377766653993875767, 1.000000000000000000),
 ( 1.000000000000000000, 0.7071067811865514585, 1.000000000000000000) ) ) 
 REPRESENTATION_ITEM ( '' )  SURFACE ( )  );
#18008 = CARTESIAN_POINT ( 'NONE',  ( 15.29449157529457004, -0.3981319440501629447, -5.199999999410266582 ) ) ;
#18009 = CARTESIAN_POINT ( 'NONE',  ( -54.47085481156724285, -3.673546848079175309, -0.7533615035078072841 ) ) ;
#18011 = DIRECTION ( 'NONE',  ( 1.000000000000000000, -1.219044193948983948E-29, 3.491481338843133355E-15 ) ) ;
#18010 = CARTESIAN_POINT ( 'NONE',  ( 61.22030551133047993, -0.7785732690188782446, 1.430137637026189790 ) ) ;
#18012 = ORIENTED_EDGE ( 'NONE', *, *, #8640, .F. ) ;
#18013 = DIRECTION ( 'NONE',  ( 0.000000000000000000, 0.9996898646859343485, 0.02490330187381124133 ) ) ;
#18014 = CARTESIAN_POINT ( 'NONE',  ( 63.50000000000000000, 1.401298464324817071E-42, -2.375000000000663913 ) ) ;
#18015 = AXIS2_PLACEMENT_3D ( 'NONE', #11688, #18507, #6302 ) ;
#18016 = EDGE_LOOP ( 'NONE', ( #3160, #16365, #19741, #10238 ) ) ;
#18018 = FACE_OUTER_BOUND ( 'NONE', #14908, .T. ) ;
#18017 = CARTESIAN_POINT ( 'NONE',  ( -44.49999999999998579, 2.308634493194285486, 1.301040651491409239 ) ) ;
#18019 = DIRECTION ( 'NONE',  ( 1.000000000000000000, 4.678365685400771632E-16, 1.520093157366894206E-16 ) ) ;
#18020 = ORIENTED_EDGE ( 'NONE', *, *, #6526, .F. ) ;
#18021 = CARTESIAN_POINT ( 'NONE',  ( -61.34999999999997300, 1.397055221233662433E-15, 2.044538471210920981E-15 ) ) ;
#18022 = ADVANCED_FACE ( 'NONE', ( #25061 ), #10882, .T. ) ;
#18023 = AXIS2_PLACEMENT_3D ( 'NONE', #9643, #26405, #9777 ) ;
#18024 = CARTESIAN_POINT ( 'NONE',  ( 58.75000000000000711, 1.749295403806236049, -0.8980135333475087744 ) ) ;
#18025 = ADVANCED_FACE ( 'NONE', ( #10810 ), #15733, .F. ) ;
#18026 = LINE ( 'NONE', #13245, #20020 ) ;
#18027 = CIRCLE ( 'NONE', #6392, 0.2500000000000000000 ) ;
#18028 = DIRECTION ( 'NONE',  ( 0.000000000000000000, -0.3589743589743593088, 0.9333474217026304087 ) ) ;
#18029 = EDGE_CURVE ( 'NONE', #23231, #11632, #10808, .T. ) ;
#18030 = CARTESIAN_POINT ( 'NONE',  ( -55.00952994616204705, 3.117691453623994580, -1.800000000000181899 ) ) ;
#18031 = CIRCLE ( 'NONE', #14492, 0.7500000000000001110 ) ;
#18032 = ORIENTED_EDGE ( 'NONE', *, *, #1021, .T. ) ;
#18033 = AXIS2_PLACEMENT_3D ( 'NONE', #21209, #3757, #6465 ) ;
#18034 = CIRCLE ( 'NONE', #27623, 5.407411300779133789 ) ;
#18035 = CIRCLE ( 'NONE', #19056, 0.1500000000000001887 ) ;
#18036 = CARTESIAN_POINT ( 'NONE',  ( 16.10705563471229951, 3.305069970238123211, 4.282766538619565466 ) ) ;
#18037 = CARTESIAN_POINT ( 'NONE',  ( 46.90000000000001279, 2.270506450603774156E-15, 4.375000000000000000 ) ) ;
#18038 = EDGE_CURVE ( 'NONE', #21791, #21815, #5313, .T. ) ;
#18039 = B_SPLINE_CURVE_WITH_KNOTS ( 'NONE', 3,
 ( #22615, #2804, #7573, #5503, #15156, #24494 ),
 .UNSPECIFIED., .F., .F.,
 ( 4, 2, 4 ),
 ( 0.000000000000000000, 0.0001000270069603039115, 0.0002000540139206078230 ),
 .UNSPECIFIED. ) ;
#18040 = DIRECTION ( 'NONE',  ( 1.000000000000000000, 3.054025858079668409E-16, -2.042474015755241579E-16 ) ) ;
#18041 = AXIS2_PLACEMENT_3D ( 'NONE', #6082, #3294, #20653 ) ;
#18042 = DIRECTION ( 'NONE',  ( 0.000000000000000000, -1.000000000000000000, 0.000000000000000000 ) ) ;
#18043 = VECTOR ( 'NONE', #18551, 1000.000000000000000 ) ;
#18044 = CARTESIAN_POINT ( 'NONE',  ( -58.07202994616203995, 2.078460969082688070, -3.600000000000190603 ) ) ;
#18045 = VECTOR ( 'NONE', #22063, 1000.000000000000000 ) ;
#18046 = DIRECTION ( 'NONE',  ( -0.9480661539417394312, 0.3180732113053816867, 0.000000000000000000 ) ) ;
#18047 = CARTESIAN_POINT ( 'NONE',  ( 34.56269065792917417, 8.313757757582560970, 2.049999999999879474 ) ) ;
#18048 = ORIENTED_EDGE ( 'NONE', *, *, #30332, .F. ) ;
#18049 = CARTESIAN_POINT ( 'NONE',  ( -54.65400635094608361, -3.399999999999987477, -0.9110272542660231565 ) ) ;
#18050 = TOROIDAL_SURFACE ( 'NONE', #4386, 0.3000000000000000444, 0.05000000000000000278 ) ;
#18051 = VERTEX_POINT ( 'NONE', #23330 ) ;
#18052 = UNCERTAINTY_MEASURE_WITH_UNIT (LENGTH_MEASURE( 1.000000000000000082E-05 ), #15208, 'distance_accuracy_value', 'NONE');
#18053 = DIRECTION ( 'NONE',  ( 0.000000000000000000, 0.000000000000000000, 1.000000000000000000 ) ) ;
#18055 = DIRECTION ( 'NONE',  ( 1.000000000000000000, 1.047444401652940007E-14, -0.000000000000000000 ) ) ;
#18054 = CARTESIAN_POINT ( 'NONE',  ( 61.25000000000000711, 1.470078920828170821, -1.470078920826818125 ) ) ;
#18056 = ORIENTED_EDGE ( 'NONE', *, *, #8536, .F. ) ;
#18057 = EDGE_LOOP ( 'NONE', ( #20171, #27717, #14029, #25045 ) ) ;
#18058 = CARTESIAN_POINT ( 'NONE',  ( -62.09999999999997300, -2.720545749060828022, -0.4014110452728629763 ) ) ;
#18059 = TOROIDAL_SURFACE ( 'NONE', #31200, 2.050000000000000266, 0.05000000000000000278 ) ;
#18060 = CARTESIAN_POINT ( 'NONE',  ( 26.19155409318043226, 5.638511060912941630, -1.425000000000091305 ) ) ;
#18061 = ORIENTED_EDGE ( 'NONE', *, *, #22187, .F. ) ;
#18062 = CIRCLE ( 'NONE', #11473, 1.000000000000000000 ) ;
#18064 = DIRECTION ( 'NONE',  ( 1.000000000000000000, 1.293068473084537258E-16, 0.000000000000000000 ) ) ;
#18063 = CARTESIAN_POINT ( 'NONE',  ( 50.80000000000001847, -4.319730106884873244, -1.256953381662414770 ) ) ;
#18065 = CIRCLE ( 'NONE', #18580, 0.09999999999999992228 ) ;
#18066 = CARTESIAN_POINT ( 'NONE',  ( -59.36042740578360366, -0.7887156198831606346, 3.845940847736174284 ) ) ;
#18067 = CARTESIAN_POINT ( 'NONE',  ( -36.11780688638071268, -4.683225673667320343, -2.703237737472844238 ) ) ;
#18068 = APPLICATION_PROTOCOL_DEFINITION ( 'draft international standard', 'automotive_design', 1998, #25911 ) ;
#18069 = EDGE_CURVE ( 'NONE', #26071, #1323, #19492, .T. ) ;
#18070 = B_SPLINE_CURVE_WITH_KNOTS ( 'NONE', 3,
 ( #8859, #4596, #20921, #30551, #11240, #16803 ),
 .UNSPECIFIED., .F., .F.,
 ( 4, 2, 4 ),
 ( 0.000000000000000000, 0.0001966045864160470319, 0.0003932091728320940638 ),
 .UNSPECIFIED. ) ;
#18071 = CARTESIAN_POINT ( 'NONE',  ( 53.32659268230732152, 4.996744265006703323, -1.614825610218436625 ) ) ;
#18072 =( NAMED_UNIT ( * ) SI_UNIT ( $, .STERADIAN. ) SOLID_ANGLE_UNIT ( ) );
#18073 = AXIS2_PLACEMENT_3D ( 'NONE', #6243, #28689, #25544 ) ;
#18074 = ORIENTED_EDGE ( 'NONE', *, *, #17773, .F. ) ;
#18075 = AXIS2_PLACEMENT_3D ( 'NONE', #13884, #30855, #6780 ) ;
#18076 = CARTESIAN_POINT ( 'NONE',  ( 53.90340377275680339, 6.895264694547793560, -2.050000000000123723 ) ) ;
#18077 = CARTESIAN_POINT ( 'NONE',  ( 51.14630318392405428, 0.9364487020640391846, 1.503522130792586342 ) ) ;
#18078 = CARTESIAN_POINT ( 'NONE',  ( 15.94709373951305054, -0.6031025731807454493, 5.374022845360696188 ) ) ;
#18079 = CARTESIAN_POINT ( 'NONE',  ( -60.49999999999997868, -2.524216908331982978, -0.06288083723137102843 ) ) ;
#18080 = AXIS2_PLACEMENT_3D ( 'NONE', #9658, #12464, #7579 ) ;
#18081 = EDGE_CURVE ( 'NONE', #7189, #6093, #29085, .T. ) ;
#18082 = VECTOR ( 'NONE', #22681, 1000.000000000000000 ) ;
#18084 = CARTESIAN_POINT ( 'NONE',  ( -44.59999999999998721, 1.599999999999998090, 3.363870538531281706 ) ) ;
#18083 = CARTESIAN_POINT ( 'NONE',  ( 51.64837794009019234, 0.8283786772117797126, 1.688958810662478660 ) ) ;
#18085 = CIRCLE ( 'NONE', #22134, 2.249352573995730520 ) ;
#18086 = CARTESIAN_POINT ( 'NONE',  ( 50.50000000000002132, 0.6462379109120995890, 4.048750000000023164 ) ) ;
#18087 = DIRECTION ( 'NONE',  ( -3.491481338843133355E-15, -3.491481338843133355E-15, 1.000000000000000000 ) ) ;
#18088 = CARTESIAN_POINT ( 'NONE',  ( -62.09999999999997300, -2.682569912478698804, -0.3012640610164738497 ) ) ;
#18089 = ORIENTED_EDGE ( 'NONE', *, *, #19713, .T. ) ;
#18090 = CARTESIAN_POINT ( 'NONE',  ( 50.38719906715036245, -1.295960864328750128, -3.889961360030737669 ) ) ;
#18091 = CARTESIAN_POINT ( 'NONE',  ( 58.75000000000002842, -1.039502773796971091, 1.800471618824829756 ) ) ;
#18092 = CIRCLE ( 'NONE', #22139, 0.04999999999999969746 ) ;
#18094 = CARTESIAN_POINT ( 'NONE',  ( 47.12416679051325730, -3.859603212985637466, -1.644059474114685893 ) ) ;
#18093 = FACE_OUTER_BOUND ( 'NONE', #30334, .T. ) ;
#18095 = DIRECTION ( 'NONE',  ( 1.000000000000000000, 1.047444401652940007E-14, 0.000000000000000000 ) ) ;
#18096 = EDGE_LOOP ( 'NONE', ( #28362, #22795, #7009, #21497 ) ) ;
#18097 = EDGE_CURVE ( 'NONE', #13195, #6282, #2267, .T. ) ;
#18098 = CARTESIAN_POINT ( 'NONE',  ( 51.29912638713659589, 3.898228643449898723, 2.049999999999820410 ) ) ;
#18099 = CARTESIAN_POINT ( 'NONE',  ( 22.04321716858593661, 7.679566743993218481, -1.550000000000076206 ) ) ;
#18100 = AXIS2_PLACEMENT_3D ( 'NONE', #4716, #5044, #19461 ) ;
#18101 = VECTOR ( 'NONE', #21681, 1000.000000000000000 ) ;
#18102 = EDGE_LOOP ( 'NONE', ( #27433, #27425, #8502 ) ) ;
#18103 = DIRECTION ( 'NONE',  ( 3.491481338843133355E-15, 3.491481338843133355E-15, -1.000000000000000000 ) ) ;
#18104 = ORIENTED_EDGE ( 'NONE', *, *, #1422, .F. ) ;
#18105 = LINE ( 'NONE', #10794, #11760 ) ;
#18106 = CARTESIAN_POINT ( 'NONE',  ( -45.15971931043468146, 0.000000000000000000, 4.700000000000000178 ) ) ;
#18107 = ORIENTED_EDGE ( 'NONE', *, *, #26532, .F. ) ;
#18108 =( LENGTH_UNIT ( ) NAMED_UNIT ( * ) SI_UNIT ( .MILLI., .METRE. ) );
#18109 = CARTESIAN_POINT ( 'NONE',  ( 25.91283125986204183, 5.216860428245192693, 1.949999999999909583 ) ) ;
#18110 = AXIS2_PLACEMENT_3D ( 'NONE', #1529, #27968, #14188 ) ;
#18111 = EDGE_CURVE ( 'NONE', #29960, #8275, #2299, .T. ) ;
#18112 = CARTESIAN_POINT ( 'NONE',  ( -58.70655989232410832, 1.962990915244748891, -3.400000000000199751 ) ) ;
#18113 = ORIENTED_EDGE ( 'NONE', *, *, #15444, .F. ) ;
#18114 = CARTESIAN_POINT ( 'NONE',  ( 56.96706223141283942, 0.7377629956704406800, -1.750942290135934831 ) ) ;
#18115 = ORIENTED_EDGE ( 'NONE', *, *, #24764, .F. ) ;
#18116 = EDGE_CURVE ( 'NONE', #30783, #28370, #28590, .T. ) ;
#18117 = ORIENTED_EDGE ( 'NONE', *, *, #8633, .F. ) ;
#18118 = CARTESIAN_POINT ( 'NONE',  ( -58.99999999999995737, 2.023778652682509683E-14, -3.400000000000209521 ) ) ;
#18119 = CYLINDRICAL_SURFACE ( 'NONE', #30160, 2.874999999999999112 ) ;
#18120 = CARTESIAN_POINT ( 'NONE',  ( -60.64999999999998437, 1.610824598944129570E-15, 1.901562740512771401E-15 ) ) ;
#18121 = CIRCLE ( 'NONE', #2421, 2.700000000000000178 ) ;
#18122 = DIRECTION ( 'NONE',  ( 0.000000000000000000, 1.000000000000000000, 8.673617379884030739E-15 ) ) ;
#18123 = CARTESIAN_POINT ( 'NONE',  ( 47.10000000000002274, -3.826179070414207573, 1.000000000000000222 ) ) ;
#18124 = AXIS2_PLACEMENT_3D ( 'NONE', #29728, #29556, #25132 ) ;
#18125 = EDGE_CURVE ( 'NONE', #618, #25510, #19222, .T. ) ;
#18126 = CIRCLE ( 'NONE', #19572, 1.899999999999999911 ) ;
#18128 = CARTESIAN_POINT ( 'NONE',  ( -57.72499999999998010, 4.751120590182407177, 0.9743475445367628662 ) ) ;
#18127 = DIRECTION ( 'NONE',  ( -1.000000000000000000, -2.586136946169074517E-16, 0.000000000000000000 ) ) ;
#18129 = CARTESIAN_POINT ( 'NONE',  ( -62.09999999999997300, 1.168016602258162478E-15, 2.197726754101795588E-15 ) ) ;
#18130 = DIRECTION ( 'NONE',  ( -0.8023336663629263565, 0.5470456816110726983, 0.2387503090077608969 ) ) ;
#18131 = DIRECTION ( 'NONE',  ( 1.520093157366878676E-16, -0.5877852522924743583, 0.8090169943749466741 ) ) ;
#18132 = DIRECTION ( 'NONE',  ( -0.9993908270190957621, 0.03489949670250106634, 3.490838185622846777E-15 ) ) ;
#18133 = CARTESIAN_POINT ( 'NONE',  ( 48.34282069333976040, -1.210123066480733200, 3.917958458743180827 ) ) ;
#18134 = ORIENTED_EDGE ( 'NONE', *, *, #22563, .T. ) ;
#18135 = CARTESIAN_POINT ( 'NONE',  ( -54.49999999999997868, -3.188085654472696540, 1.181570928782897267 ) ) ;
#18136 = ADVANCED_FACE ( 'NONE', ( #28863 ), #18585, .T. ) ;
#18137 = CARTESIAN_POINT ( 'NONE',  ( 51.25000000000001421, 5.368152558471320595E-13, 3.111507638930570854E-58 ) ) ;
#18138 = ORIENTED_EDGE ( 'NONE', *, *, #27272, .F. ) ;
#18139 = ORIENTED_EDGE ( 'NONE', *, *, #26822, .T. ) ;
#18140 =( LENGTH_UNIT ( ) NAMED_UNIT ( * ) SI_UNIT ( .MILLI., .METRE. ) );
#18141 = CARTESIAN_POINT ( 'NONE',  ( 61.25000000000001421, 0.8666666666673039643, -1.374595900215358268 ) ) ;
#18143 = CARTESIAN_POINT ( 'NONE',  ( -54.49999999999997868, -4.179189514726506793, -0.8999999999999998002 ) ) ;
#18142 = CARTESIAN_POINT ( 'NONE',  ( -56.31249999999998579, -1.962990915244731793, 3.399999999999792077 ) ) ;
#18144 = EDGE_LOOP ( 'NONE', ( #19510, #2301, #1147, #879 ) ) ;
#18145 = ORIENTED_EDGE ( 'NONE', *, *, #18280, .T. ) ;
#18146 = CARTESIAN_POINT ( 'NONE',  ( 51.80000000000001137, -3.933368109459640660, -2.186004417993355098 ) ) ;
#18147 =( GEOMETRIC_REPRESENTATION_CONTEXT ( 3 ) GLOBAL_UNCERTAINTY_ASSIGNED_CONTEXT ( ( #30053 ) ) GLOBAL_UNIT_ASSIGNED_CONTEXT ( ( #16501, #1936, #9223 ) ) REPRESENTATION_CONTEXT ( 'NONE', 'WORKASPACE' ) );
#18148 = ORIENTED_EDGE ( 'NONE', *, *, #25906, .F. ) ;
#18149 = DIRECTION ( 'NONE',  ( 0.000000000000000000, 1.000000000000000000, 3.491481338843130594E-15 ) ) ;
#18150 = EDGE_CURVE ( 'NONE', #19150, #13242, #25017, .T. ) ;
#18151 =( BOUNDED_SURFACE ( )  B_SPLINE_SURFACE ( 1, 2, ( 
 ( #17591, #7463, #22490, #3167, #12809, #17134, #26779, #788, #29767, #5084, #19666, #14734, #22034, #330, #29303, #5228, #17275, #26917, #14877, #24539, #2858, #12508, #25175, #11075, #22960, #30065, #28170, #20604, #8541, #3494, #1415, #25473, #27863, #30528, #1250, #3782, #13131, #30233, #15971, #13421, #6177, #963, #18226, #12978, #1108, #10613, #20756, #25795, #15822, #17897, #23127, #27533, #10911, #6486, #30384, #10758, #8686, #28005, #8834, #1565, #16146, #18367, #6320, #13271, #25636, #22666, #22820, #3949, #13589, #8380, #23279, #8230, #20291, #18526, #29920, #11224, #20898, #15682, #5859, #15522, #20440, #18066, #27709, #6031, #25328, #3637, #31010, #16304, #23899, #16628, #19000, #21703, #23751, #26271, #4251, #21386, #7120, #4577, #28649, #23428, #11705, #4103, #23588, #1710, #11855, #16928, #6967, #9014, #14225 ),
 ( #26423, #4719, #12027, #28335, #16779, #14376, #11378, #21233, #21063, #2191, #24047, #28486, #21533, #30865, #13895, #1891, #31175, #30707, #9508, #9331, #13743, #2043, #2358, #6792, #14141, #19169, #9182, #28809, #18844, #9662, #19316, #28952, #18686, #6640, #25949, #7260, #11556, #16451, #26108, #4423, #14069, #14551, #27204, #29560, #7875, #24671, #5513, #15168, #3136, #9957, #2527, #24362, #12309, #597, #22458, #288, #7722, #17552, #7584, #2984, #2813, #19632, #24822, #29271, #17383, #753, #26572, #4885, #9796, #24502, #24215, #5338, #20098, #26883, #10414, #19464, #17244, #10259, #29732, #10111, #8046, #12777, #12176, #5193, #21857, #144, #29109, #29414, #2673, #27030, #15003, #12627, #7426, #12468, #22312, #19928, #14841, #22160, #17100, #26748, #5048, #448, #14701, #21996, #19778, #16225, #23353, #5824, #18447 ) ),
 .UNSPECIFIED., .F., .F., .F. ) 
 B_SPLINE_SURFACE_WITH_KNOTS ( ( 2, 2 ),
 ( 3, 2, 2, 2, 2, 2, 2, 2, 2, 2, 2, 2, 2, 2, 2, 2, 2, 2, 2, 2, 2, 2, 2, 2, 2, 2, 2, 2, 2, 2, 2, 2, 2, 2, 2, 2, 2, 2, 2, 2, 2, 2, 2, 2, 2, 2, 2, 2, 2, 2, 2, 2, 2, 2, 3 ),
 ( 0.000000000000000000, 1.000000000000000000 ),
 ( 0.000000000000000000, 0.01851851851851851749, 0.03703703703703703498, 0.05555555555555555247, 0.07407407407407406996, 0.09259259259259258745, 0.1111111111111111049, 0.1296296296296296224, 0.1481481481481481399, 0.1666666666666666574, 0.1851851851851851749, 0.2037037037037036924, 0.2222222222222222099, 0.2407407407407407274, 0.2592592592592592449, 0.2777777777777777901, 0.2962962962962962798, 0.3148148148148148251, 0.3333333333333333148, 0.3518518518518518601, 0.3703703703703703498, 0.3888888888888888951, 0.4074074074074073848, 0.4259259259259259300, 0.4444444444444444198, 0.4629629629629629650, 0.4814814814814814548, 0.5000000000000000000, 0.5185185185185184897, 0.5370370370370370905, 0.5555555555555555802, 0.5740740740740740700, 0.5925925925925925597, 0.6111111111111111605, 0.6296296296296296502, 0.6481481481481481399, 0.6666666666666666297, 0.6851851851851852304, 0.7037037037037037202, 0.7222222222222222099, 0.7407407407407406996, 0.7592592592592593004, 0.7777777777777777901, 0.7962962962962962798, 0.8148148148148147696, 0.8333333333333333703, 0.8518518518518518601, 0.8703703703703703498, 0.8888888888888888395, 0.9074074074074074403, 0.9259259259259259300, 0.9444444444444444198, 0.9629629629629629095, 0.9814814814814815103, 1.000000000000000000 ),
 .UNSPECIFIED. ) 
 GEOMETRIC_REPRESENTATION_ITEM ( )  RATIONAL_B_SPLINE_SURFACE ( (
 ( 1.000000000000000000, 0.8660254037844387076, 1.000000000000000000, 0.8660254037844387076, 1.000000000000000000, 0.8660254037844387076, 1.000000000000000000, 0.8660254037844387076, 1.000000000000000000, 0.8660254037844387076, 1.000000000000000000, 0.8660254037844387076, 1.000000000000000000, 0.8660254037844387076, 1.000000000000000000, 0.8660254037844387076, 1.000000000000000000, 0.8660254037844387076, 1.000000000000000000, 0.8660254037844387076, 1.000000000000000000, 0.8660254037844387076, 1.000000000000000000, 0.8660254037844387076, 1.000000000000000000, 0.8660254037844387076, 1.000000000000000000, 0.8660254037844387076, 1.000000000000000000, 0.8660254037844387076, 1.000000000000000000, 0.8660254037844387076, 1.000000000000000000, 0.8660254037844387076, 1.000000000000000000, 0.8660254037844387076, 1.000000000000000000, 0.8660254037844387076, 1.000000000000000000, 0.8660254037844387076, 1.000000000000000000, 0.8660254037844387076, 1.000000000000000000, 0.8660254037844387076, 1.000000000000000000, 0.8660254037844387076, 1.000000000000000000, 0.8660254037844387076, 1.000000000000000000, 0.8660254037844387076, 1.000000000000000000, 0.8660254037844387076, 1.000000000000000000, 0.8660254037844387076, 1.000000000000000000, 0.8660254037844387076, 1.000000000000000000, 0.8660254037844387076, 1.000000000000000000, 0.8660254037844387076, 1.000000000000000000, 0.8660254037844387076, 1.000000000000000000, 0.8660254037844387076, 1.000000000000000000, 0.8660254037844387076, 1.000000000000000000, 0.8660254037844387076, 1.000000000000000000, 0.8660254037844387076, 1.000000000000000000, 0.8660254037844387076, 1.000000000000000000, 0.8660254037844387076, 1.000000000000000000, 0.8660254037844387076, 1.000000000000000000, 0.8660254037844387076, 1.000000000000000000, 0.8660254037844387076, 1.000000000000000000, 0.8660254037844387076, 1.000000000000000000, 0.8660254037844387076, 1.000000000000000000, 0.8660254037844387076, 1.000000000000000000, 0.8660254037844387076, 1.000000000000000000, 0.8660254037844387076, 1.000000000000000000, 0.8660254037844387076, 1.000000000000000000, 0.8660254037844387076, 1.000000000000000000, 0.8660254037844387076, 1.000000000000000000, 0.8660254037844387076, 1.000000000000000000, 0.8660254037844387076, 1.000000000000000000, 0.8660254037844387076, 1.000000000000000000, 0.8660254037844387076, 1.000000000000000000, 0.8660254037844387076, 1.000000000000000000, 0.8660254037844387076, 1.000000000000000000),
 ( 1.000000000000000000, 0.8660254037844387076, 1.000000000000000000, 0.8660254037844387076, 1.000000000000000000, 0.8660254037844387076, 1.000000000000000000, 0.8660254037844387076, 1.000000000000000000, 0.8660254037844387076, 1.000000000000000000, 0.8660254037844387076, 1.000000000000000000, 0.8660254037844387076, 1.000000000000000000, 0.8660254037844387076, 1.000000000000000000, 0.8660254037844387076, 1.000000000000000000, 0.8660254037844387076, 1.000000000000000000, 0.8660254037844387076, 1.000000000000000000, 0.8660254037844387076, 1.000000000000000000, 0.8660254037844387076, 1.000000000000000000, 0.8660254037844387076, 1.000000000000000000, 0.8660254037844387076, 1.000000000000000000, 0.8660254037844387076, 1.000000000000000000, 0.8660254037844387076, 1.000000000000000000, 0.8660254037844387076, 1.000000000000000000, 0.8660254037844387076, 1.000000000000000000, 0.8660254037844387076, 1.000000000000000000, 0.8660254037844387076, 1.000000000000000000, 0.8660254037844387076, 1.000000000000000000, 0.8660254037844387076, 1.000000000000000000, 0.8660254037844387076, 1.000000000000000000, 0.8660254037844387076, 1.000000000000000000, 0.8660254037844387076, 1.000000000000000000, 0.8660254037844387076, 1.000000000000000000, 0.8660254037844387076, 1.000000000000000000, 0.8660254037844387076, 1.000000000000000000, 0.8660254037844387076, 1.000000000000000000, 0.8660254037844387076, 1.000000000000000000, 0.8660254037844387076, 1.000000000000000000, 0.8660254037844387076, 1.000000000000000000, 0.8660254037844387076, 1.000000000000000000, 0.8660254037844387076, 1.000000000000000000, 0.8660254037844387076, 1.000000000000000000, 0.8660254037844387076, 1.000000000000000000, 0.8660254037844387076, 1.000000000000000000, 0.8660254037844387076, 1.000000000000000000, 0.8660254037844387076, 1.000000000000000000, 0.8660254037844387076, 1.000000000000000000, 0.8660254037844387076, 1.000000000000000000, 0.8660254037844387076, 1.000000000000000000, 0.8660254037844387076, 1.000000000000000000, 0.8660254037844387076, 1.000000000000000000, 0.8660254037844387076, 1.000000000000000000, 0.8660254037844387076, 1.000000000000000000, 0.8660254037844387076, 1.000000000000000000, 0.8660254037844387076, 1.000000000000000000, 0.8660254037844387076, 1.000000000000000000, 0.8660254037844387076, 1.000000000000000000, 0.8660254037844387076, 1.000000000000000000, 0.8660254037844387076, 1.000000000000000000, 0.8660254037844387076, 1.000000000000000000) ) ) 
 REPRESENTATION_ITEM ( '' )  SURFACE ( )  );
#18152 = ORIENTED_EDGE ( 'NONE', *, *, #1460, .F. ) ;
#18153 = CARTESIAN_POINT ( 'NONE',  ( -54.49999999999997868, 8.366749974758391359E-15, -1.938977325913827332E-13 ) ) ;
#18154 = EDGE_CURVE ( 'NONE', #25147, #19387, #4302, .T. ) ;
#18155 = EDGE_LOOP ( 'NONE', ( #28918, #13404, #14529, #7119 ) ) ;
#18156 = CARTESIAN_POINT ( 'NONE',  ( 52.06628335902944826, 0.5434431642986583544, -1.996089927833914146 ) ) ;
#18157 = ADVANCED_FACE ( 'NONE', ( #11272 ), #4156, .F. ) ;
#18158 = CYLINDRICAL_SURFACE ( 'NONE', #30336, 3.750000000000000444 ) ;
#18159 = CARTESIAN_POINT ( 'NONE',  ( -44.49999999999998579, -1.843099986694572142E-14, 0.000000000000000000 ) ) ;
#18160 = CARTESIAN_POINT ( 'NONE',  ( 15.03925126672132961, 1.123735532908305634, 5.289358697221540950 ) ) ;
#18161 = CARTESIAN_POINT ( 'NONE',  ( -60.26905989232410121, 2.023778652682511261E-14, -3.400000000000213518 ) ) ;
#18162 = CARTESIAN_POINT ( 'NONE',  ( -54.49999999999996447, -1.599999999999981215, -3.363870538531692489 ) ) ;
#18163 = CARTESIAN_POINT ( 'NONE',  ( 58.74999981196283727, 1.321459237640902007, 1.441661833135547965 ) ) ;
#18164 = CARTESIAN_POINT ( 'NONE',  ( 58.50000000000001421, 0.000000000000000000, 0.000000000000000000 ) ) ;
#18165 = CARTESIAN_POINT ( 'NONE',  ( 57.01637874260923411, 0.7374533274050908416, -1.789443367489095049 ) ) ;
#18166 = CARTESIAN_POINT ( 'NONE',  ( 50.25000000000002842, -0.6373668173464875908, -1.895722432252557432 ) ) ;
#18167 =( GEOMETRIC_REPRESENTATION_CONTEXT ( 3 ) GLOBAL_UNCERTAINTY_ASSIGNED_CONTEXT ( ( #24075 ) ) GLOBAL_UNIT_ASSIGNED_CONTEXT ( ( #15355, #30240, #20445 ) ) REPRESENTATION_CONTEXT ( 'NONE', 'WORKASPACE' ) );
#18168 = DIRECTION ( 'NONE',  ( 1.000000000000000000, 1.047444401652940007E-14, 0.000000000000000000 ) ) ;
#18169 = CARTESIAN_POINT ( 'NONE',  ( 50.25000000000000000, 1.791164585742626159, 0.8897917884450912140 ) ) ;
#18170 = CIRCLE ( 'NONE', #26753, 4.849999999999999645 ) ;
#18171 = CARTESIAN_POINT ( 'NONE',  ( 58.75000000000002132, 6.153735859711025284E-13, 3.111507638930570854E-58 ) ) ;
#18172 = EDGE_LOOP ( 'NONE', ( #26713, #12758, #5937, #24986, #17584, #474, #16232 ) ) ;
#18173 = ADVANCED_FACE ( 'NONE', ( #4306 ), #22507, .T. ) ;
#18174 = CARTESIAN_POINT ( 'NONE',  ( 54.32946523776459458, 6.710822964229192777, -2.050000000000189004 ) ) ;
#18175 = ORIENTED_EDGE ( 'NONE', *, *, #2445, .T. ) ;
#18176 = CARTESIAN_POINT ( 'NONE',  ( -59.66183546925923764, -3.174920041538525251, -1.216504307364950854 ) ) ;
#18177 = ORIENTED_EDGE ( 'NONE', *, *, #5323, .F. ) ;
#18178 = EDGE_CURVE ( 'NONE', #3064, #21345, #8836, .T. ) ;
#18179 = DIRECTION ( 'NONE',  ( 1.000000000000000000, 1.047444401652940007E-14, 0.000000000000000000 ) ) ;
#18180 = CARTESIAN_POINT ( 'NONE',  ( -58.22085481156723574, -3.673546848079176197, -0.7533615035078065070 ) ) ;
#18181 = AXIS2_PLACEMENT_3D ( 'NONE', #30468, #30958, #8772 ) ;
#18183 = DIRECTION ( 'NONE',  ( -1.000000000000000000, -1.047444401652940007E-14, -0.000000000000000000 ) ) ;
#18182 = FACE_OUTER_BOUND ( 'NONE', #17309, .T. ) ;
#18184 = EDGE_LOOP ( 'NONE', ( #17789, #22813 ) ) ;
#18185 = CARTESIAN_POINT ( 'NONE',  ( 34.56269065792915995, 8.313757757582562746, -2.050000000000119726 ) ) ;
#18186 = CARTESIAN_POINT ( 'NONE',  ( 57.03449256411899881, -0.7475344026195360758, -1.780552047803072302 ) ) ;
#18187 = ORIENTED_EDGE ( 'NONE', *, *, #30622, .F. ) ;
#18189 = CARTESIAN_POINT ( 'NONE',  ( -35.85663232820584767, 4.383220986679467579, -0.4611378927914189241 ) ) ;
#18188 = CARTESIAN_POINT ( 'NONE',  ( 50.32838854698020725, 1.409900272549312827, 3.850000494969507248 ) ) ;
#18190 = CARTESIAN_POINT ( 'NONE',  ( 50.80000000000002558, -4.319730106884873244, 1.256953381662059277 ) ) ;
#18191 = ORIENTED_EDGE ( 'NONE', *, *, #31282, .F. ) ;
#18192 = CARTESIAN_POINT ( 'NONE',  ( -36.30424252565939724, 4.979756346315198812, -1.501439362221551166 ) ) ;
#18193 = EDGE_CURVE ( 'NONE', #22436, #19955, #17044, .T. ) ;
#18194 = CARTESIAN_POINT ( 'NONE',  ( -54.50990849663458704, -3.088199225670062997, 1.451082037244374900 ) ) ;
#18195 = AXIS2_PLACEMENT_3D ( 'NONE', #6055, #30557, #13456 ) ;
#18196 = CARTESIAN_POINT ( 'NONE',  ( 22.07280086217095061, 8.086143481909148889, 2.049999999999922995 ) ) ;
#18197 = DIRECTION ( 'NONE',  ( 1.000000000000000000, 1.047444401652940007E-14, 0.000000000000000000 ) ) ;
#18198 = CARTESIAN_POINT ( 'NONE',  ( -54.44999999999997442, 1.499999999999999556, -3.300094695611021312 ) ) ;
#18199 = ORIENTED_EDGE ( 'NONE', *, *, #31253, .T. ) ;
#18200 = CARTESIAN_POINT ( 'NONE',  ( 15.03925126672125501, 2.525801270006243548, 4.794550352686353101 ) ) ;
#18201 = SHAPE_REPRESENTATION ( 'Body', ( #9018 ), #23745 ) ;
#18202 = CARTESIAN_POINT ( 'NONE',  ( -54.73542740578361077, -3.725040285533364859, 1.239922660687674760 ) ) ;
#18203 = AXIS2_PLACEMENT_3D ( 'NONE', #11220, #11701, #9010 ) ;
#18204 = CARTESIAN_POINT ( 'NONE',  ( 51.70000000000001705, -4.276948333784438283, 0.9210526315789470120 ) ) ;
#18205 = EDGE_CURVE ( 'NONE', #23306, #4483, #26795, .T. ) ;
#18206 = CARTESIAN_POINT ( 'NONE',  ( -57.13452994616205416, 3.117691453623977260, 1.799999999999813971 ) ) ;
#18207 = CARTESIAN_POINT ( 'NONE',  ( -35.85663232820579793, 1.123735532908286316, 5.289358697221541838 ) ) ;
#18208 = CARTESIAN_POINT ( 'NONE',  ( 48.42201677308601404, 1.327156576403744959, -3.879406274192464643 ) ) ;
#18209 = ADVANCED_FACE ( 'NONE', ( #17149 ), #17678, .T. ) ;
#18210 = ORIENTED_EDGE ( 'NONE', *, *, #10374, .F. ) ;
#18211 = CIRCLE ( 'NONE', #6554, 0.04999999999999988481 ) ;
#18212 = CIRCLE ( 'NONE', #25265, 1.975000000000001865 ) ;
#18213 = CARTESIAN_POINT ( 'NONE',  ( -57.31249999999996447, 3.400000000000008349, -1.881930883448047941E-13 ) ) ;
#18214 = VERTEX_POINT ( 'NONE', #17608 ) ;
#18215 = EDGE_CURVE ( 'NONE', #26599, #4962, #15430, .T. ) ;
#18216 = CARTESIAN_POINT ( 'NONE',  ( -59.17529728802922051, 2.511751407530337765, -0.9443652579017279836 ) ) ;
#18218 = DIRECTION ( 'NONE',  ( 1.000000000000000000, 0.000000000000000000, -4.738179285253040686E-16 ) ) ;
#18217 = CARTESIAN_POINT ( 'NONE',  ( 58.65000000000000568, 0.8495817349404608532, -1.671477153794393766 ) ) ;
#18219 = ORIENTED_EDGE ( 'NONE', *, *, #5080, .T. ) ;
#18220 = ORIENTED_EDGE ( 'NONE', *, *, #568, .T. ) ;
#18221 = DIRECTION ( 'NONE',  ( 0.000000000000000000, 1.000000000000000000, 0.000000000000000000 ) ) ;
#18222 = VECTOR ( 'NONE', #6249, 1000.000000000000000 ) ;
#18223 = CARTESIAN_POINT ( 'NONE',  ( 50.25000000000001421, 0.6373668173465375508, 1.895722432253563516 ) ) ;
#18225 = LINE ( 'NONE', #6484, #31219 ) ;
#18224 = CARTESIAN_POINT ( 'NONE',  ( 51.41699094018468230, -4.256549615192540159, -1.449195206876658482 ) ) ;
#18226 = CARTESIAN_POINT ( 'NONE',  ( -56.92292740578359656, -3.330682475591783209, -0.6830477631804109384 ) ) ;
#18227 = CARTESIAN_POINT ( 'NONE',  ( -36.04581030752632387, -4.861582136949317068, -2.394243986684321701 ) ) ;
#18228 = PRODUCT_CONTEXT ( 'NONE', #10736, 'mechanical' ) ;
#18229 = EDGE_CURVE ( 'NONE', #20284, #26116, #26548, .T. ) ;
#18230 = CARTESIAN_POINT ( 'NONE',  ( 56.95000000000001705, -0.7137254901960785602, 2.500119182087999548 ) ) ;
#18231 = ORIENTED_EDGE ( 'NONE', *, *, #21785, .T. ) ;
#18232 = FACE_OUTER_BOUND ( 'NONE', #21702, .T. ) ;
#18233 = CARTESIAN_POINT ( 'NONE',  ( 54.23225718638637005, 5.947176913004134313, -2.050000000000189004 ) ) ;
#18234 = CARTESIAN_POINT ( 'NONE',  ( 51.15394434968253279, 0.9591183795348902086, -1.387856512383046637 ) ) ;
#18235 = CARTESIAN_POINT ( 'NONE',  ( 15.41170998834797246, 0.6969927240736308871, 5.374332520738719587 ) ) ;
#18236 = AXIS2_PLACEMENT_3D ( 'NONE', #4848, #14345, #16747 ) ;
#18237 = CARTESIAN_POINT ( 'NONE',  ( -55.06249999999997158, 3.400000000000007905, -1.826733775103631524E-13 ) ) ;
#18239 = DIRECTION ( 'NONE',  ( 0.000000000000000000, 0.000000000000000000, 1.000000000000000000 ) ) ;
#18238 = LINE ( 'NONE', #8097, #18082 ) ;
#18240 = CARTESIAN_POINT ( 'NONE',  ( 53.96125931204732495, 5.169815675097246377, -2.050000000000188116 ) ) ;
#18242 = DIRECTION ( 'NONE',  ( 1.000000000000000000, 1.047444401652940007E-14, 0.000000000000000000 ) ) ;
#18241 = CARTESIAN_POINT ( 'NONE',  ( 31.35411506561226602, 7.935106537971987173, 1.424999999999891021 ) ) ;
#18243 = ADVANCED_FACE ( 'NONE', ( #27875 ), #3183, .F. ) ;
#18244 = EDGE_LOOP ( 'NONE', ( #8756, #16573, #16556, #31095 ) ) ;
#18245 = DIRECTION ( 'NONE',  ( -1.000000000000000000, -1.047444401652940007E-14, -0.000000000000000000 ) ) ;
#18246 = CARTESIAN_POINT ( 'NONE',  ( -36.92398358572908990, 3.410993390446889872, -4.205682099886818293 ) ) ;
#18248 = CARTESIAN_POINT ( 'NONE',  ( -59.67318048135356179, -2.383480368854686393, -1.229362881338657454 ) ) ;
#18247 = CARTESIAN_POINT ( 'NONE',  ( -67.89999999999997726, -1.599503783497495890, -0.03984528299809441537 ) ) ;
#18249 = DIRECTION ( 'NONE',  ( 1.000000000000000000, 1.047444401652940007E-14, 0.000000000000000000 ) ) ;
#18250 = ORIENTED_EDGE ( 'NONE', *, *, #13638, .F. ) ;
#18251 = DIRECTION ( 'NONE',  ( -1.000000000000000000, -1.047444401652940007E-14, -0.000000000000000000 ) ) ;
#18252 = CARTESIAN_POINT ( 'NONE',  ( 47.00572760024188312, -4.149162114478044394, 1.064915450748001424 ) ) ;
#18253 = ORIENTED_EDGE ( 'NONE', *, *, #10926, .T. ) ;
#18254 = CARTESIAN_POINT ( 'NONE',  ( -61.34999999999997300, -2.609922480197373940, 0.4591346723570145505 ) ) ;
#18255 = ORIENTED_EDGE ( 'NONE', *, *, #395, .F. ) ;
#18256 = CARTESIAN_POINT ( 'NONE',  ( 61.25000000000002132, 6.415596960124259844E-13, 3.111507638930570854E-58 ) ) ;
#18257 = CARTESIAN_POINT ( 'NONE',  ( 47.10000000000000853, 7.037371096768279372E-14, -4.500000000000199840 ) ) ;
#18258 = ORIENTED_EDGE ( 'NONE', *, *, #22542, .T. ) ;
#18259 = AXIS2_PLACEMENT_3D ( 'NONE', #21710, #28958, #19176 ) ;
#18260 = CARTESIAN_POINT ( 'NONE',  ( -56.25952994616206126, -1.280183170538300192E-14, 3.599999999999798916 ) ) ;
#18261 = EDGE_CURVE ( 'NONE', #27932, #826, #1764, .T. ) ;
#18262 = CARTESIAN_POINT ( 'NONE',  ( -59.45655989232410832, 1.962990915244748891, -3.400000000000202416 ) ) ;
#18263 = ORIENTED_EDGE ( 'NONE', *, *, #30205, .T. ) ;
#18264 = CARTESIAN_POINT ( 'NONE',  ( 56.99280487254718253, 0.7628505807388673565, -1.740142286037820618 ) ) ;
#18265 = VERTEX_POINT ( 'NONE', #12997 ) ;
#18266 = VERTEX_POINT ( 'NONE', #25190 ) ;
#18267 = CARTESIAN_POINT ( 'NONE',  ( -56.24999999999997868, -2.944486372867089141, 1.699999999999789235 ) ) ;
#18268 = DIRECTION ( 'NONE',  ( 0.000000000000000000, 0.000000000000000000, 1.000000000000000000 ) ) ;
#18269 = CARTESIAN_POINT ( 'NONE',  ( 22.11060592828335203, 7.457498294695588115, -1.425000000000077094 ) ) ;
#18270 = CARTESIAN_POINT ( 'NONE',  ( -44.49999999999997868, 4.700000000000000178, 0.000000000000000000 ) ) ;
#18271 = DIRECTION ( 'NONE',  ( 3.491481338843133355E-15, 3.491481338843133355E-15, -1.000000000000000000 ) ) ;
#18273 = DIRECTION ( 'NONE',  ( 1.000000000000000000, -0.000000000000000000, -1.047444401652940007E-14 ) ) ;
#18272 = CARTESIAN_POINT ( 'NONE',  ( -35.85663232820584057, 4.018128179617551865, -3.618665901676622720 ) ) ;
#18274 = PRESENTATION_STYLE_ASSIGNMENT (( #8598 ) ) ;
#18275 = DIRECTION ( 'NONE',  ( 1.000000000000000000, 0.000000000000000000, -3.491481338843133355E-15 ) ) ;
#18276 = DIRECTION ( 'NONE',  ( 1.000000000000000000, 1.018631342913014973E-14, 0.000000000000000000 ) ) ;
#18277 = EDGE_CURVE ( 'NONE', #16857, #9403, #10384, .T. ) ;
#18278 = CARTESIAN_POINT ( 'NONE',  ( 56.95000000000001705, 0.7255611966503594523, 2.496740365009429752 ) ) ;
#18279 = CARTESIAN_POINT ( 'NONE',  ( 48.30268969835653792, -0.9327905306641465222, 3.995066436131524235 ) ) ;
#18280 = EDGE_CURVE ( 'NONE', #4799, #24892, #12885, .T. ) ;
#18281 = DIRECTION ( 'NONE',  ( 0.000000000000000000, -0.9996898646859344595, -0.02490330187381123786 ) ) ;
#18282 = ORIENTED_EDGE ( 'NONE', *, *, #20261, .F. ) ;
#18283 = DIRECTION ( 'NONE',  ( -2.581436205204234499E-16, 0.9796124928211140670, 0.2008964009354147762 ) ) ;
#18284 = ORIENTED_EDGE ( 'NONE', *, *, #18537, .T. ) ;
#18285 = DIRECTION ( 'NONE',  ( -1.000000000000000000, -0.000000000000000000, -0.000000000000000000 ) ) ;
#18286 = CYLINDRICAL_SURFACE ( 'NONE', #17338, 2.374999999999998668 ) ;
#18288 = CARTESIAN_POINT ( 'NONE',  ( 56.95118308248727601, 0.7317690799413573144, -2.494914055551520793 ) ) ;
#18287 = CARTESIAN_POINT ( 'NONE',  ( -56.24999999999997868, -2.944486372867089141, 1.699999999999789235 ) ) ;
#18289 = ORIENTED_EDGE ( 'NONE', *, *, #9177, .F. ) ;
#18290 = ORIENTED_EDGE ( 'NONE', *, *, #10083, .T. ) ;
#18291 = DIRECTION ( 'NONE',  ( 0.000000000000000000, 0.4295302013422958032, 0.9030524935654886676 ) ) ;
#18292 = ORIENTED_EDGE ( 'NONE', *, *, #23253, .F. ) ;
#18293 = CARTESIAN_POINT ( 'NONE',  ( 58.74999999305997989, -1.657788420846199706, 0.9867593359912983919 ) ) ;
#18294 = AXIS2_PLACEMENT_3D ( 'NONE', #15760, #28094, #16233 ) ;
#18295 = VERTEX_POINT ( 'NONE', #20307 ) ;
#18296 = CARTESIAN_POINT ( 'NONE',  ( 22.00282357524660171, 7.757228885921728434, -2.049999999999808420 ) ) ;
#18297 = CARTESIAN_POINT ( 'NONE',  ( 36.55000000000001847, 0.000000000000000000, 0.000000000000000000 ) ) ;
#18298 = DIRECTION ( 'NONE',  ( 1.000000000000000000, 1.047444401652940007E-14, 0.000000000000000000 ) ) ;
#18299 = ORIENTED_EDGE ( 'NONE', *, *, #4292, .T. ) ;
#18300 = CARTESIAN_POINT ( 'NONE',  ( -69.18535533905931345, -6.887031541980249260E-16, 2.444420817412074983E-15 ) ) ;
#18301 = EDGE_CURVE ( 'NONE', #21983, #29950, #15697, .T. ) ;
#18302 = CARTESIAN_POINT ( 'NONE',  ( 47.19713079078776019, -3.901416201057355426, 1.541017813822200155 ) ) ;
#18303 = CARTESIAN_POINT ( 'NONE',  ( 15.18459684427939926, 4.018128179617495022, 3.618665901676702656 ) ) ;
#18304 = AXIS2_PLACEMENT_3D ( 'NONE', #6686, #6221, #30758 ) ;
#18305 = CARTESIAN_POINT ( 'NONE',  ( 51.23644008536122385, 1.080112125196981854, 1.214076932077872817 ) ) ;
#18306 = DIRECTION ( 'NONE',  ( -1.000000000000000000, 1.219044193948983948E-29, -3.491481338843133355E-15 ) ) ;
#18308 = FACE_OUTER_BOUND ( 'NONE', #7325, .T. ) ;
#18307 = DIRECTION ( 'NONE',  ( 0.000000000000000000, 0.8914544820235111855, -0.4531102586349080030 ) ) ;
#18309 = TOROIDAL_SURFACE ( 'NONE', #21980, 1.824999999999998623, 0.05000000000000000278 ) ;
#18310 = CARTESIAN_POINT ( 'NONE',  ( -44.49999999999997868, -4.766731106216475591E-14, -1.485745783470907590E-13 ) ) ;
#18311 = LINE ( 'NONE', #18169, #8952 ) ;
#18312 = AXIS2_PLACEMENT_3D ( 'NONE', #78, #19400, #29042 ) ;
#18313 = EDGE_CURVE ( 'NONE', #4452, #22781, #27552, .T. ) ;
#18314 = FACE_OUTER_BOUND ( 'NONE', #24886, .T. ) ;
#18315 = ADVANCED_FACE ( 'NONE', ( #25344 ), #20771, .T. ) ;
#18316 = ORIENTED_EDGE ( 'NONE', *, *, #7209, .F. ) ;
#18317 = ADVANCED_FACE ( 'NONE', ( #20153 ), #9807, .F. ) ;
#18318 = DIRECTION ( 'NONE',  ( 2.459994892347944311E-12, 0.6683962987616191009, -0.7438053426816511049 ) ) ;
#18319 = ORIENTED_EDGE ( 'NONE', *, *, #9215, .F. ) ;
#18320 = ORIENTED_EDGE ( 'NONE', *, *, #6943, .F. ) ;
#18321 = CARTESIAN_POINT ( 'NONE',  ( 51.67634979243387505, -3.859233156638911755, 1.644927388240807531 ) ) ;
#18322 =( BOUNDED_SURFACE ( )  B_SPLINE_SURFACE ( 1, 2, ( 
 ( #14656, #405, #4998, #24319, #10065, #19739, #23198, #15886, #25244, #1486, #3861, #8750, #15746, #10681, #17822, #27458, #29988, #8299, #20513, #8610, #20674, #5773, #20209, #8151, #20365, #30447, #22736, #3413, #18287, #18142, #25712, #10830, #15425, #25396, #30301, #25077, #13053, #3700, #22569, #10996, #27781, #11142, #29839, #30140, #13340, #28075, #8464, #6096, #6397, #15598, #1032, #1174, #6242, #13513, #23032, #25543, #16062, #20817, #18440, #10535, #17967, #27616, #1326, #12881, #5944, #27927, #3565, #13199, #22883, #876, #11287, #6867, #11628, #4019, #23671, #4646, #28404, #26343, #4493, #30779, #9406, #21146, #1627, #16535, #1962, #13807, #26190, #31256, #9090, #14147, #14301, #16369, #2112, #21307, #6706, #23972, #18761, #23823, #9579, #13662, #23344, #18606, #30936, #20970, #11776, #28879, #4323, #19240, #28248 ),
 ( #7187, #9252, #21451, #18913, #23491, #13975, #2266, #19075, #31081, #6558, #28730, #16855, #26015, #30603, #8916, #7040, #16219, #16702, #28556, #25866, #11929, #21617, #4168, #1784, #11462, #8082, #10455, #13129, #15201, #961, #19959, #26492, #15520, #27389, #20134, #14455, #3165, #4797, #14617, #24131, #3324, #17009, #10611, #4964, #2439, #65, #24849, #20438, #12975, #12099, #17589, #29765, #24285, #25174, #10756, #17747, #20289, #27236, #29918, #30063, #7338, #22664, #5549, #12658, #12807, #21778, #9726, #1106, #19385, #5698, #15349, #29594, #24996, #8378, #3015, #629, #22488, #22341, #8228, #17895, #29029, #26662, #7917, #10291, #786, #27531, #5857, #3491, #22818, #16143, #1707, #13586, #23276, #6175, #13269, #11221, #20601, #11375, #25326, #1562, #18683, #6029, #4100, #22958, #10909, #20895, #27706, #25792, #30525 ) ),
 .UNSPECIFIED., .F., .F., .F. ) 
 B_SPLINE_SURFACE_WITH_KNOTS ( ( 2, 2 ),
 ( 3, 2, 2, 2, 2, 2, 2, 2, 2, 2, 2, 2, 2, 2, 2, 2, 2, 2, 2, 2, 2, 2, 2, 2, 2, 2, 2, 2, 2, 2, 2, 2, 2, 2, 2, 2, 2, 2, 2, 2, 2, 2, 2, 2, 2, 2, 2, 2, 2, 2, 2, 2, 2, 2, 3 ),
 ( 0.000000000000000000, 1.000000000000000000 ),
 ( 0.000000000000000000, 0.01851851851851851749, 0.03703703703703703498, 0.05555555555555555247, 0.07407407407407406996, 0.09259259259259258745, 0.1111111111111111049, 0.1296296296296296224, 0.1481481481481481399, 0.1666666666666666574, 0.1851851851851851749, 0.2037037037037036924, 0.2222222222222222099, 0.2407407407407407274, 0.2592592592592592449, 0.2777777777777777901, 0.2962962962962962798, 0.3148148148148148251, 0.3333333333333333148, 0.3518518518518518601, 0.3703703703703703498, 0.3888888888888888951, 0.4074074074074073848, 0.4259259259259259300, 0.4444444444444444198, 0.4629629629629629650, 0.4814814814814814548, 0.5000000000000000000, 0.5185185185185184897, 0.5370370370370370905, 0.5555555555555555802, 0.5740740740740740700, 0.5925925925925925597, 0.6111111111111111605, 0.6296296296296296502, 0.6481481481481481399, 0.6666666666666666297, 0.6851851851851852304, 0.7037037037037037202, 0.7222222222222222099, 0.7407407407407406996, 0.7592592592592593004, 0.7777777777777777901, 0.7962962962962962798, 0.8148148148148147696, 0.8333333333333333703, 0.8518518518518518601, 0.8703703703703703498, 0.8888888888888888395, 0.9074074074074074403, 0.9259259259259259300, 0.9444444444444444198, 0.9629629629629629095, 0.9814814814814815103, 1.000000000000000000 ),
 .UNSPECIFIED. ) 
 GEOMETRIC_REPRESENTATION_ITEM ( )  RATIONAL_B_SPLINE_SURFACE ( (
 ( 1.000000000000000000, 0.8660254037844387076, 1.000000000000000000, 0.8660254037844387076, 1.000000000000000000, 0.8660254037844387076, 1.000000000000000000, 0.8660254037844387076, 1.000000000000000000, 0.8660254037844387076, 1.000000000000000000, 0.8660254037844387076, 1.000000000000000000, 0.8660254037844387076, 1.000000000000000000, 0.8660254037844387076, 1.000000000000000000, 0.8660254037844387076, 1.000000000000000000, 0.8660254037844387076, 1.000000000000000000, 0.8660254037844387076, 1.000000000000000000, 0.8660254037844387076, 1.000000000000000000, 0.8660254037844387076, 1.000000000000000000, 0.8660254037844387076, 1.000000000000000000, 0.8660254037844387076, 1.000000000000000000, 0.8660254037844387076, 1.000000000000000000, 0.8660254037844387076, 1.000000000000000000, 0.8660254037844387076, 1.000000000000000000, 0.8660254037844387076, 1.000000000000000000, 0.8660254037844387076, 1.000000000000000000, 0.8660254037844387076, 1.000000000000000000, 0.8660254037844387076, 1.000000000000000000, 0.8660254037844387076, 1.000000000000000000, 0.8660254037844387076, 1.000000000000000000, 0.8660254037844387076, 1.000000000000000000, 0.8660254037844387076, 1.000000000000000000, 0.8660254037844387076, 1.000000000000000000, 0.8660254037844387076, 1.000000000000000000, 0.8660254037844387076, 1.000000000000000000, 0.8660254037844387076, 1.000000000000000000, 0.8660254037844387076, 1.000000000000000000, 0.8660254037844387076, 1.000000000000000000, 0.8660254037844387076, 1.000000000000000000, 0.8660254037844387076, 1.000000000000000000, 0.8660254037844387076, 1.000000000000000000, 0.8660254037844387076, 1.000000000000000000, 0.8660254037844387076, 1.000000000000000000, 0.8660254037844387076, 1.000000000000000000, 0.8660254037844387076, 1.000000000000000000, 0.8660254037844387076, 1.000000000000000000, 0.8660254037844387076, 1.000000000000000000, 0.8660254037844387076, 1.000000000000000000, 0.8660254037844387076, 1.000000000000000000, 0.8660254037844387076, 1.000000000000000000, 0.8660254037844387076, 1.000000000000000000, 0.8660254037844387076, 1.000000000000000000, 0.8660254037844387076, 1.000000000000000000, 0.8660254037844387076, 1.000000000000000000, 0.8660254037844387076, 1.000000000000000000, 0.8660254037844387076, 1.000000000000000000, 0.8660254037844387076, 1.000000000000000000, 0.8660254037844387076, 1.000000000000000000, 0.8660254037844387076, 1.000000000000000000, 0.8660254037844387076, 1.000000000000000000),
 ( 1.000000000000000000, 0.8660254037844387076, 1.000000000000000000, 0.8660254037844387076, 1.000000000000000000, 0.8660254037844387076, 1.000000000000000000, 0.8660254037844387076, 1.000000000000000000, 0.8660254037844387076, 1.000000000000000000, 0.8660254037844387076, 1.000000000000000000, 0.8660254037844387076, 1.000000000000000000, 0.8660254037844387076, 1.000000000000000000, 0.8660254037844387076, 1.000000000000000000, 0.8660254037844387076, 1.000000000000000000, 0.8660254037844387076, 1.000000000000000000, 0.8660254037844387076, 1.000000000000000000, 0.8660254037844387076, 1.000000000000000000, 0.8660254037844387076, 1.000000000000000000, 0.8660254037844387076, 1.000000000000000000, 0.8660254037844387076, 1.000000000000000000, 0.8660254037844387076, 1.000000000000000000, 0.8660254037844387076, 1.000000000000000000, 0.8660254037844387076, 1.000000000000000000, 0.8660254037844387076, 1.000000000000000000, 0.8660254037844387076, 1.000000000000000000, 0.8660254037844387076, 1.000000000000000000, 0.8660254037844387076, 1.000000000000000000, 0.8660254037844387076, 1.000000000000000000, 0.8660254037844387076, 1.000000000000000000, 0.8660254037844387076, 1.000000000000000000, 0.8660254037844387076, 1.000000000000000000, 0.8660254037844387076, 1.000000000000000000, 0.8660254037844387076, 1.000000000000000000, 0.8660254037844387076, 1.000000000000000000, 0.8660254037844387076, 1.000000000000000000, 0.8660254037844387076, 1.000000000000000000, 0.8660254037844387076, 1.000000000000000000, 0.8660254037844387076, 1.000000000000000000, 0.8660254037844387076, 1.000000000000000000, 0.8660254037844387076, 1.000000000000000000, 0.8660254037844387076, 1.000000000000000000, 0.8660254037844387076, 1.000000000000000000, 0.8660254037844387076, 1.000000000000000000, 0.8660254037844387076, 1.000000000000000000, 0.8660254037844387076, 1.000000000000000000, 0.8660254037844387076, 1.000000000000000000, 0.8660254037844387076, 1.000000000000000000, 0.8660254037844387076, 1.000000000000000000, 0.8660254037844387076, 1.000000000000000000, 0.8660254037844387076, 1.000000000000000000, 0.8660254037844387076, 1.000000000000000000, 0.8660254037844387076, 1.000000000000000000, 0.8660254037844387076, 1.000000000000000000, 0.8660254037844387076, 1.000000000000000000, 0.8660254037844387076, 1.000000000000000000, 0.8660254037844387076, 1.000000000000000000, 0.8660254037844387076, 1.000000000000000000, 0.8660254037844387076, 1.000000000000000000) ) ) 
 REPRESENTATION_ITEM ( '' )  SURFACE ( )  );
#18323 = ORIENTED_EDGE ( 'NONE', *, *, #6312, .F. ) ;
#18324 = CARTESIAN_POINT ( 'NONE',  ( 54.23463818034554862, 5.946682447858800735, 2.049999999999810640 ) ) ;
#18325 = CARTESIAN_POINT ( 'NONE',  ( -59.15835481156722864, -0.8699069336946633202, 4.241846523238430144 ) ) ;
#18327 = CARTESIAN_POINT ( 'NONE',  ( 51.80000000000001137, -3.700146292169718354, -1.985065161562939107 ) ) ;
#18326 = CARTESIAN_POINT ( 'NONE',  ( 50.50000000000001421, 0.7375000000005331735, 3.111507638930570854E-58 ) ) ;
#18328 = ORIENTED_EDGE ( 'NONE', *, *, #4402, .T. ) ;
#18329 = ORIENTED_EDGE ( 'NONE', *, *, #18280, .F. ) ;
#18330 = CARTESIAN_POINT ( 'NONE',  ( 31.73174553812004106, 7.673395716939830358, -2.050000000000110845 ) ) ;
#18331 = LINE ( 'NONE', #13557, #19605 ) ;
#18332 = EDGE_CURVE ( 'NONE', #27746, #24537, #23610, .T. ) ;
#18333 = ORIENTED_EDGE ( 'NONE', *, *, #18991, .F. ) ;
#18335 = DIRECTION ( 'NONE',  ( 1.000000000000000000, 0.000000000000000000, -3.491481338843133355E-15 ) ) ;
#18334 = DIRECTION ( 'NONE',  ( 1.000000000000000000, 0.000000000000000000, -0.000000000000000000 ) ) ;
#18336 = CARTESIAN_POINT ( 'NONE',  ( -56.14405989232413674, -1.162579938981959285E-14, 3.399999999999799627 ) ) ;
#18337 = ORIENTED_EDGE ( 'NONE', *, *, #17141, .F. ) ;
#18338 = B_SPLINE_CURVE_WITH_KNOTS ( 'NONE', 3,
 ( #2164, #28924, #18814, #28458 ),
 .UNSPECIFIED., .F., .F.,
 ( 4, 4 ),
 ( 8.741117365843378158E-19, 2.862003379457683788E-05 ),
 .UNSPECIFIED. ) ;
#18339 = CARTESIAN_POINT ( 'NONE',  ( -36.22909104983143180, 5.326676561279607647, -0.9978806102894379748 ) ) ;
#18340 = CARTESIAN_POINT ( 'NONE',  ( 58.66118217212532215, 1.806736155628216656, -0.5016043952913777915 ) ) ;
#18341 = CARTESIAN_POINT ( 'NONE',  ( -36.00197790576392265, -4.018128179617563411, 3.618665901676646701 ) ) ;
#18342 = FACE_OUTER_BOUND ( 'NONE', #11512, .T. ) ;
#18343 = CYLINDRICAL_SURFACE ( 'NONE', #19465, 0.05000000000000001665 ) ;
#18344 = ADVANCED_FACE ( 'NONE', ( #31027 ), #23441, .T. ) ;
#18345 = EDGE_CURVE ( 'NONE', #15816, #25173, #13896, .T. ) ;
#18346 = CYLINDRICAL_SURFACE ( 'NONE', #23096, 1.000000000000000000 ) ;
#18347 = CARTESIAN_POINT ( 'NONE',  ( -58.61042740578360366, -0.7887156198831720699, 3.845940847736171619 ) ) ;
#18348 = CARTESIAN_POINT ( 'NONE',  ( -56.59585481156723574, -1.184343223768586251, -3.558065644182725862 ) ) ;
#18349 = EDGE_CURVE ( 'NONE', #25407, #13124, #20517, .T. ) ;
#18350 = EDGE_CURVE ( 'NONE', #30038, #18483, #14431, .T. ) ;
#18351 = FACE_OUTER_BOUND ( 'NONE', #23849, .T. ) ;
#18352 = CARTESIAN_POINT ( 'NONE',  ( 58.65844932252321797, -1.874781853996629666, -0.03312599131424567855 ) ) ;
#18353 = DIRECTION ( 'NONE',  ( 0.000000000000000000, -4.336808689942024836E-15, 1.000000000000000000 ) ) ;
#18354 = ORIENTED_EDGE ( 'NONE', *, *, #16828, .T. ) ;
#18355 = CARTESIAN_POINT ( 'NONE',  ( 58.65000038048027164, 1.663933463836820170, 0.8644232797869607632 ) ) ;
#18356 = EDGE_LOOP ( 'NONE', ( #20334, #3375, #6833, #23447 ) ) ;
#18357 = CYLINDRICAL_SURFACE ( 'NONE', #2091, 0.09999999999999850675 ) ;
#18359 = CARTESIAN_POINT ( 'NONE',  ( 68.00000000000004263, 0.7500000000000000000, 1.988246715072644166 ) ) ;
#18358 = DIRECTION ( 'NONE',  ( 3.002035892788116966E-16, -0.9996898646859343485, -0.02490330187381124133 ) ) ;
#18360 = EDGE_LOOP ( 'NONE', ( #14151, #28213, #11783, #8692 ) ) ;
#18361 = ORIENTED_EDGE ( 'NONE', *, *, #2247, .F. ) ;
#18362 = CARTESIAN_POINT ( 'NONE',  ( -59.28448904087068883, -2.425384292835011557, -1.073600088316542411 ) ) ;
#18363 = CARTESIAN_POINT ( 'NONE',  ( 29.29107486424065243, 6.659593085418572755, 1.424999999999897238 ) ) ;
#18365 = CARTESIAN_POINT ( 'NONE',  ( -55.47085481156723574, 1.184343223768591580, 3.558065644182726750 ) ) ;
#18364 = DIRECTION ( 'NONE',  ( 1.000000000000000000, 1.047444401652940007E-14, 0.000000000000000000 ) ) ;
#18366 = ORIENTED_EDGE ( 'NONE', *, *, #25559, .F. ) ;
#18367 = CARTESIAN_POINT ( 'NONE',  ( -58.11042740578360366, 3.725040285533370632, -1.239922660687675871 ) ) ;
#18368 = AXIS2_PLACEMENT_3D ( 'NONE', #19384, #6866, #24130 ) ;
#18369 = FACE_OUTER_BOUND ( 'NONE', #14953, .T. ) ;
#18370 = ITEM_DEFINED_TRANSFORMATION ( 'NONE', 'NONE', #26266,  #9018 ) ;
#18371 = CARTESIAN_POINT ( 'NONE',  ( 57.05000000000001847, -0.8156862745098041323, 2.468735688885368873 ) ) ;
#18372 = B_SPLINE_CURVE_WITH_KNOTS ( 'NONE', 3,
 ( #6496, #6331, #18698, #8693, #23764, #8847, #31022, #13600, #23289, #1574, #18540, #16154, #4112 ),
 .UNSPECIFIED., .F., .F.,
 ( 4, 3, 3, 3, 4 ),
 ( 0.000000000000000000, 4.969793434218336409E-05, 9.932084631986548421E-05, 0.0001499488332825157780, 0.0001857305951757664718 ),
 .UNSPECIFIED. ) ;
#18373 = EDGE_CURVE ( 'NONE', #8368, #20255, #780, .T. ) ;
#18374 = ORIENTED_EDGE ( 'NONE', *, *, #1113, .T. ) ;
#18375 = ADVANCED_FACE ( 'NONE', ( #6502 ), #14090, .F. ) ;
#18376 = CARTESIAN_POINT ( 'NONE',  ( 47.03019939778821623, -4.166995010554928491, -1.027517533905029090 ) ) ;
#18377 = EDGE_CURVE ( 'NONE', #3768, #23038, #25655, .T. ) ;
#18378 = CARTESIAN_POINT ( 'NONE',  ( -36.22955757456080761, 2.840625797034106448, -4.363718033548086517 ) ) ;
#18379 = CARTESIAN_POINT ( 'NONE',  ( 58.45000000000001705, -0.8156862745098041323, -2.468735688885368873 ) ) ;
#18380 = DIRECTION ( 'NONE',  ( -0.9993908270190957621, 0.03489949670250100389, 3.492120980335537899E-15 ) ) ;
#18381 = CARTESIAN_POINT ( 'NONE',  ( -59.69999999999998153, -2.279157448682842091, 1.538811659727345349 ) ) ;
#18383 = FACE_OUTER_BOUND ( 'NONE', #26710, .T. ) ;
#18382 = CARTESIAN_POINT ( 'NONE',  ( -55.03335481156724995, 0.7533615035078067290, -3.673546848079180194 ) ) ;
#18384 = AXIS2_PLACEMENT_3D ( 'NONE', #30370, #8673, #6306 ) ;
#18385 = AXIS2_PLACEMENT_3D ( 'NONE', #10940, #27883, #1437 ) ;
#18386 = CARTESIAN_POINT ( 'NONE',  ( 52.38136139153902349, 3.988241223888660869, -2.045676639479365733 ) ) ;
#18388 = CARTESIAN_POINT ( 'NONE',  ( -54.49999999999997868, 3.712072993515388664, 0.5023824248525554648 ) ) ;
#18387 = DIRECTION ( 'NONE',  ( 1.000000000000000000, 1.047444401652940007E-14, 0.000000000000000000 ) ) ;
#18389 = EDGE_LOOP ( 'NONE', ( #1488, #30849, #18117, #11591 ) ) ;
#18390 = CARTESIAN_POINT ( 'NONE',  ( 50.40000000000001279, -0.6462379109120511833, -4.048750000000022276 ) ) ;
#18391 = B_SPLINE_CURVE_WITH_KNOTS ( 'NONE', 3,
 ( #29368, #21810, #9905, #9756, #29509, #12271, #27154, #240, #99, #10361, #8001, #19879, #701, #20038, #29682, #5149 ),
 .UNSPECIFIED., .F., .F.,
 ( 4, 2, 2, 2, 2, 2, 2, 4 ),
 ( 1.738108305489988542E-18, 0.0004351083927046406927, 0.0008702167854092796506, 0.001740433570818558217, 0.002175541963523197446, 0.002610650356227837109, 0.003045758748932476771, 0.003480867141637116434 ),
 .UNSPECIFIED. ) ;
#18392 = CARTESIAN_POINT ( 'NONE',  ( -54.49999999999997868, 9.184850993605150903E-17, 0.7500000000000001110 ) ) ;
#18394 = CARTESIAN_POINT ( 'NONE',  ( 47.00000000000002132, -3.701043595308294076, -1.983423889356798142 ) ) ;
#18393 = CARTESIAN_POINT ( 'NONE',  ( 58.72200624034154259, 1.805437858156837549, 0.5064713447814576108 ) ) ;
#18395 = CARTESIAN_POINT ( 'NONE',  ( 15.22780280894164129, -5.340403875751315255, 0.9205822004573636086 ) ) ;
#18396 = VERTEX_POINT ( 'NONE', #16649 ) ;
#18397 = CARTESIAN_POINT ( 'NONE',  ( 52.18343291569984643, 8.689381540779885782, 2.049999999999818190 ) ) ;
#18398 = DIRECTION ( 'NONE',  ( 1.000000000000000000, 0.000000000000000000, 0.000000000000000000 ) ) ;
#18399 = ORIENTED_EDGE ( 'NONE', *, *, #8503, .T. ) ;
#18400 = LINE ( 'NONE', #28037, #19969 ) ;
#18401 = ORIENTED_EDGE ( 'NONE', *, *, #16282, .T. ) ;
#18402 = CARTESIAN_POINT ( 'NONE',  ( 15.59140265158955607, 3.917459231545712850, -3.727878977586764009 ) ) ;
#18403 = CARTESIAN_POINT ( 'NONE',  ( 51.25000000000001421, 5.368159983410797313E-13, 3.111507638930570854E-58 ) ) ;
#18404 = ORIENTED_EDGE ( 'NONE', *, *, #12165, .T. ) ;
#18405 =( NAMED_UNIT ( * ) PLANE_ANGLE_UNIT ( ) SI_UNIT ( $, .RADIAN. ) );
#18406 = CARTESIAN_POINT ( 'NONE',  ( 23.02975722382757695, 6.234282476769586800, 1.949999999999919131 ) ) ;
#18407 = CARTESIAN_POINT ( 'NONE',  ( -58.45655989232412963, 1.962990915244722245, 3.399999999999800071 ) ) ;
#18408 = ORIENTED_EDGE ( 'NONE', *, *, #30476, .T. ) ;
#18409 = DIRECTION ( 'NONE',  ( -1.000000000000000000, -1.047444401652940007E-14, -0.000000000000000000 ) ) ;
#18410 = ORIENTED_EDGE ( 'NONE', *, *, #14822, .T. ) ;
#18411 = CIRCLE ( 'NONE', #8776, 0.1500000000000001887 ) ;
#18412 = EDGE_CURVE ( 'NONE', #6633, #9415, #16453, .T. ) ;
#18413 = VERTEX_POINT ( 'NONE', #26291 ) ;
#18414 = EDGE_CURVE ( 'NONE', #20935, #18759, #23296, .T. ) ;
#18415 = CARTESIAN_POINT ( 'NONE',  ( -56.87499999999996447, -2.944486372867076707, -1.700000000000212674 ) ) ;
#18416 = ADVANCED_FACE ( 'NONE', ( #18383 ), #6844, .F. ) ;
#18417 = CARTESIAN_POINT ( 'NONE',  ( 56.95349779155813508, -0.7404564066163630276, 2.492333105726597164 ) ) ;
#18418 = DIRECTION ( 'NONE',  ( 1.000000000000000000, 1.047444401652940007E-14, 0.000000000000000000 ) ) ;
#18419 = CARTESIAN_POINT ( 'NONE',  ( 57.05000000000001847, 0.8156862745098041323, 2.468735688885368873 ) ) ;
#18420 = VECTOR ( 'NONE', #26253, 1000.000000000000000 ) ;
#18421 = CARTESIAN_POINT ( 'NONE',  ( -54.49999999999997868, -1.550000000000000044, 3.300094695611020867 ) ) ;
#18423 = DIRECTION ( 'NONE',  ( 0.000000000000000000, 0.000000000000000000, 1.000000000000000000 ) ) ;
#18422 = CARTESIAN_POINT ( 'NONE',  ( -36.79682133506354091, 4.944296796129599159, -2.193698057025677439 ) ) ;
#18424 = DIRECTION ( 'NONE',  ( -1.520093157366847861E-16, 0.5877852522924624790, 0.8090169943749551118 ) ) ;
#18425 = CARTESIAN_POINT ( 'NONE',  ( 58.45000000000001705, 0.8000000000000001554, -1.778341924377873973 ) ) ;
#18426 = CARTESIAN_POINT ( 'NONE',  ( -55.74999999999997158, -2.489203624310587948, 2.804704140674914026 ) ) ;
#18427 = EDGE_CURVE ( 'NONE', #10413, #13311, #14246, .T. ) ;
#18428 = CARTESIAN_POINT ( 'NONE',  ( 58.65000000000003411, -1.571497941946114585, -1.022750809560766250 ) ) ;
#18429 = CARTESIAN_POINT ( 'NONE',  ( 56.95000000000001705, 0.7137254901960784492, -2.500119182087999548 ) ) ;
#18430 = AXIS2_PLACEMENT_3D ( 'NONE', #2396, #7001, #4920 ) ;
#18431 = CARTESIAN_POINT ( 'NONE',  ( -59.29999999999996163, 1.763130761670032021, 3.204107478254790919 ) ) ;
#18432 = B_SPLINE_CURVE_WITH_KNOTS ( 'NONE', 3,
 ( #15202, #3166, #787, #10456, #14876, #20135, #5227, #7462, #29766, #27390, #5699, #15350, #9831, #21887, #19498, #328 ),
 .UNSPECIFIED., .F., .F.,
 ( 4, 3, 3, 3, 3, 4 ),
 ( 0.000000000000000000, 3.843454199181276345E-05, 7.602611568626176531E-05, 0.0001118455301991774195, 0.0001459326773459513119, 0.0001653157283245150629 ),
 .UNSPECIFIED. ) ;
#18433 = ORIENTED_EDGE ( 'NONE', *, *, #2171, .T. ) ;
#18434 = CARTESIAN_POINT ( 'NONE',  ( -54.50000000000001421, -3.416259366980110901, 0.5361331873031048856 ) ) ;
#18435 = FACE_OUTER_BOUND ( 'NONE', #24591, .T. ) ;
#18436 = ORIENTED_EDGE ( 'NONE', *, *, #20198, .F. ) ;
#18437 = CARTESIAN_POINT ( 'NONE',  ( 51.31572262954152563, 1.002608958138273554, 1.584424273060082378 ) ) ;
#18438 = AXIS2_PLACEMENT_3D ( 'NONE', #21543, #31185, #19177 ) ;
#18439 = DIRECTION ( 'NONE',  ( 0.000000000000000000, 0.000000000000000000, 1.000000000000000000 ) ) ;
#18441 = CARTESIAN_POINT ( 'NONE',  ( 56.99824518417612751, 0.8016297048612398557, -2.473345119325445651 ) ) ;
#18440 = CARTESIAN_POINT ( 'NONE',  ( -58.12499999999996447, 2.944486372867106905, -1.700000000000193801 ) ) ;
#18442 = VERTEX_POINT ( 'NONE', #13604 ) ;
#18443 = VERTEX_POINT ( 'NONE', #11237 ) ;
#18444 = CARTESIAN_POINT ( 'NONE',  ( 58.45000000000001705, -0.7794871794871796045, -1.732743413496389939 ) ) ;
#18445 = ORIENTED_EDGE ( 'NONE', *, *, #18215, .T. ) ;
#18446 = CARTESIAN_POINT ( 'NONE',  ( 61.09423418603945777, 0.6373668173466511266, 1.895722432253563516 ) ) ;
#18447 = CARTESIAN_POINT ( 'NONE',  ( -61.24999999999996447, 3.673546848079179750, 0.7533615035078069511 ) ) ;
#18448 = ORIENTED_EDGE ( 'NONE', *, *, #15191, .T. ) ;
#18449 = CARTESIAN_POINT ( 'NONE',  ( 24.17629218427073923, 5.599093920977425753, -2.050000000000020695 ) ) ;
#18450 = CARTESIAN_POINT ( 'NONE',  ( -59.69999999999997442, -3.237160264815294841, -1.238538609462289219 ) ) ;
#18451 = VECTOR ( 'NONE', #8462, 1000.000000000000000 ) ;
#18452 = CARTESIAN_POINT ( 'NONE',  ( -44.59999999999997300, 8.366749974758271452E-15, -1.593320673368357066E-13 ) ) ;
#18453 = ORIENTED_EDGE ( 'NONE', *, *, #19319, .T. ) ;
#18454 = ORIENTED_EDGE ( 'NONE', *, *, #13224, .T. ) ;
#18455 = EDGE_CURVE ( 'NONE', #12071, #26911, #21003, .T. ) ;
#18456 = DIRECTION ( 'NONE',  ( -1.000000000000000000, -3.053848253006669023E-16, 2.042510438544995415E-16 ) ) ;
#18457 = EDGE_CURVE ( 'NONE', #865, #31227, #25569, .T. ) ;
#18458 = CARTESIAN_POINT ( 'NONE',  ( 15.32752150720753725, 1.093737229520479692, 5.295968199484769379 ) ) ;
#18460 = CARTESIAN_POINT ( 'NONE',  ( 57.03828022491683924, -0.8151581666669124315, -2.468910358759941914 ) ) ;
#18459 = CIRCLE ( 'NONE', #4286, 1.000000000000000000 ) ;
#18461 = CARTESIAN_POINT ( 'NONE',  ( 47.10000000000002984, -3.550773357292059007, 2.049880134335656745 ) ) ;
#18462 = DIRECTION ( 'NONE',  ( 0.000000000000000000, -0.2008964009354147484, 0.9796124928211139560 ) ) ;
#18463 = PLANE ( 'NONE',  #4514 ) ;
#18464 = AXIS2_PLACEMENT_3D ( 'NONE', #25509, #11254, #8717 ) ;
#18465 = CARTESIAN_POINT ( 'NONE',  ( 57.00000000000001421, 0.7059996929583092218, -1.815412393553804460 ) ) ;
#18467 = DIRECTION ( 'NONE',  ( 0.000000000000000000, 0.000000000000000000, 1.000000000000000000 ) ) ;
#18466 = CARTESIAN_POINT ( 'NONE',  ( -61.38137739671037707, -2.621185111045226446, 0.6505274733237536022 ) ) ;
#18468 = DIRECTION ( 'NONE',  ( 3.002035892788117459E-16, -0.9996898646859344595, -0.02490330187381123786 ) ) ;
#18469 = DIRECTION ( 'NONE',  ( 0.000000000000000000, 0.9996898646859344595, 0.02490330187381122745 ) ) ;
#18470 = ADVANCED_FACE ( 'NONE', ( #2832 ), #15023, .F. ) ;
#18471 = DIRECTION ( 'NONE',  ( 1.000000000000000000, 1.047444401652940007E-14, 0.000000000000000000 ) ) ;
#18472 =( BOUNDED_SURFACE ( )  B_SPLINE_SURFACE ( 3, 2, ( 
 ( #14562, #24227, #10230 ),
 ( #29527, #20991, #3579 ),
 ( #9111, #13685, #8483 ),
 ( #23366, #20696, #30164 ),
 ( #13532, #6114, #28267 ),
 ( #8770, #3717, #30320 ),
 ( #15619, #18780, #27801 ),
 ( #18163, #5965, #15764 ),
 ( #8628, #11306, #11486 ),
 ( #18626, #3882, #30467 ) ),
 .UNSPECIFIED., .F., .F., .T. ) 
 B_SPLINE_SURFACE_WITH_KNOTS ( ( 4, 2, 2, 2, 4 ),
 ( 3, 3 ),
 ( 0.0001706658715694011708, 0.0002229276920777971318, 0.0002751895125861931199, 0.0003274513330945891081, 0.0003797131536029850962 ),
 ( 0.000000000000000000, 1.000000000000000000 ),
 .UNSPECIFIED. ) 
 GEOMETRIC_REPRESENTATION_ITEM ( )  RATIONAL_B_SPLINE_SURFACE ( (
 ( 1.000000000000000000, 0.7071067811865441310, 1.000000000000000000),
 ( 1.000000000000000000, 0.7375607040700675743, 1.000000000000000000),
 ( 1.000000000000000000, 0.7730431127425798632, 1.000000000000000000),
 ( 1.000000000000000000, 0.8321012486979311173, 1.000000000000000000),
 ( 1.000000000000000000, 0.8541932017400215571, 1.000000000000000000),
 ( 1.000000000000000000, 0.8545723906050046725, 1.000000000000000000),
 ( 1.000000000000000000, 0.8327032135041435579, 1.000000000000000000),
 ( 1.000000000000000000, 0.7734559727060076328, 1.000000000000000000),
 ( 1.000000000000000000, 0.7377766653995073698, 1.000000000000000000),
 ( 1.000000000000000000, 0.7071067811865465735, 1.000000000000000000) ) ) 
 REPRESENTATION_ITEM ( '' )  SURFACE ( )  );
#18473 = ORIENTED_EDGE ( 'NONE', *, *, #4082, .T. ) ;
#18474 = VECTOR ( 'NONE', #15992, 1000.000000000000000 ) ;
#18475 = ORIENTED_EDGE ( 'NONE', *, *, #29371, .F. ) ;
#18476 = CARTESIAN_POINT ( 'NONE',  ( 58.75000000000002132, 6.153735859711025284E-13, 3.111507638930570854E-58 ) ) ;
#18477 = ORIENTED_EDGE ( 'NONE', *, *, #211, .T. ) ;
#18478 = CARTESIAN_POINT ( 'NONE',  ( 54.16322038507461656, 5.604326647956827223, 2.049999999999811084 ) ) ;
#18479 = CIRCLE ( 'NONE', #11892, 1.875000000000001776 ) ;
#18480 = CARTESIAN_POINT ( 'NONE',  ( -59.28335481156722864, 3.238593381231847257, 2.874284765127022911 ) ) ;
#18482 = CARTESIAN_POINT ( 'NONE',  ( -35.85663232820581925, 3.426725943139507624, 3.937891353488775170 ) ) ;
#18481 = FACE_OUTER_BOUND ( 'NONE', #30412, .T. ) ;
#18483 = VERTEX_POINT ( 'NONE', #160 ) ;
#18484 = EDGE_LOOP ( 'NONE', ( #23631, #24132, #1286, #5587 ) ) ;
#18485 = DIRECTION ( 'NONE',  ( 2.117927888850090591E-16, -0.02490330187381111643, 0.9996898646859343485 ) ) ;
#18486 = CARTESIAN_POINT ( 'NONE',  ( 57.05000000000001847, -0.7500000000000000000, -1.778341924377873751 ) ) ;
#18487 = ORIENTED_EDGE ( 'NONE', *, *, #29531, .T. ) ;
#18489 = CARTESIAN_POINT ( 'NONE',  ( 51.80000048029754822, 4.021162616303429971, -2.019962949071075542 ) ) ;
#18488 = CARTESIAN_POINT ( 'NONE',  ( 57.00000000000001421, 0.6999999999999999556, -2.452039967047845437 ) ) ;
#18490 = CIRCLE ( 'NONE', #23048, 0.09999999999999989453 ) ;
#18491 = VERTEX_POINT ( 'NONE', #26895 ) ;
#18492 = FACE_OUTER_BOUND ( 'NONE', #24453, .T. ) ;
#18493 = CARTESIAN_POINT ( 'NONE',  ( 51.14630318392407560, -0.9364487020629673752, -1.503522130792586564 ) ) ;
#18494 = EDGE_CURVE ( 'NONE', #12299, #8533, #20538, .T. ) ;
#18495 = FILL_AREA_STYLE_COLOUR ( '', #29601 ) ;
#18496 = CARTESIAN_POINT ( 'NONE',  ( -59.00952994616203284, -3.117691453623963938, -1.800000000000220757 ) ) ;
#18497 = ADVANCED_FACE ( 'NONE', ( #31197 ), #9526, .T. ) ;
#18498 = VECTOR ( 'NONE', #28021, 1000.000000000000114 ) ;
#18499 = AXIS2_PLACEMENT_3D ( 'NONE', #692, #24912, #10527 ) ;
#18500 = CARTESIAN_POINT ( 'NONE',  ( 61.05467743520237178, -0.5998170657512601478, -1.862568116882888480 ) ) ;
#18501 = AXIS2_PLACEMENT_3D ( 'NONE', #19904, #18168, #27810 ) ;
#18502 = CIRCLE ( 'NONE', #25558, 0.5000000000000013323 ) ;
#18503 = CARTESIAN_POINT ( 'NONE',  ( -56.86042740578360366, -2.936324665650192234, -2.606018187048508850 ) ) ;
#18504 = EDGE_CURVE ( 'NONE', #11045, #23968, #20068, .T. ) ;
#18505 =( BOUNDED_CURVE ( )  B_SPLINE_CURVE ( 2, ( #8176, #10850, #12907, #15453, #3107, #20233, #27647, #13074, #17843 ),
 .UNSPECIFIED., .F., .T. ) 
 B_SPLINE_CURVE_WITH_KNOTS ( ( 3, 2, 2, 2, 3 ),
 ( 0.6388888888888889506, 0.6481481481481481399, 0.6666666666666666297, 0.6851851851851852304, 0.6944444444444445308 ),
 .UNSPECIFIED. ) 
 CURVE ( )  GEOMETRIC_REPRESENTATION_ITEM ( )  RATIONAL_B_SPLINE_CURVE ( ( 0.9330127018922194093, 0.9330127018922197424, 1.000000000000000000, 0.8660254037844387076, 1.000000000000000000, 0.8660254037844387076, 1.000000000000000000, 0.9330127018922189652, 0.9330127018922194093 ) ) 
 REPRESENTATION_ITEM ( '' )  );
#18506 = CARTESIAN_POINT ( 'NONE',  ( -55.83155989232411542, -1.962990915244703372, -3.400000000000206413 ) ) ;
#18507 = DIRECTION ( 'NONE',  ( 0.000000000000000000, -1.000000000000000000, 0.000000000000000000 ) ) ;
#18508 = CARTESIAN_POINT ( 'NONE',  ( -36.30347965937240673, 0.1138661108245775516, 5.199999999057504319 ) ) ;
#18509 = DIRECTION ( 'NONE',  ( 0.7071067811865455743, 7.319954787623226069E-15, -0.7071067811865493491 ) ) ;
#18510 = ORIENTED_EDGE ( 'NONE', *, *, #28677, .T. ) ;
#18511 = CARTESIAN_POINT ( 'NONE',  ( 58.66122797211851747, 1.615588400947291392, 0.9517229765820476306 ) ) ;
#18512 = ORIENTED_EDGE ( 'NONE', *, *, #12120, .F. ) ;
#18513 = DIRECTION ( 'NONE',  ( 0.000000000000000000, 0.000000000000000000, 1.000000000000000000 ) ) ;
#18515 = DIRECTION ( 'NONE',  ( 1.000000000000000000, 1.047444401652940007E-14, 0.000000000000000000 ) ) ;
#18514 = CARTESIAN_POINT ( 'NONE',  ( 48.40000000000002700, 0.6304760106459517122, 3.950000000000022826 ) ) ;
#18516 = ADVANCED_FACE ( 'NONE', ( #5208 ), #12486, .F. ) ;
#18517 = EDGE_LOOP ( 'NONE', ( #30196, #9330, #23228, #23483 ) ) ;
#18518 = CIRCLE ( 'NONE', #6870, 4.600000000000036948 ) ;
#18519 = ORIENTED_EDGE ( 'NONE', *, *, #10405, .T. ) ;
#18520 = FACE_OUTER_BOUND ( 'NONE', #6087, .T. ) ;
#18521 = AXIS2_PLACEMENT_3D ( 'NONE', #14598, #24552, #2576 ) ;
#18522 = CARTESIAN_POINT ( 'NONE',  ( -44.49999999999997868, 6.542789527549899840E-15, -1.397091617737396343E-15 ) ) ;
#18524 = CARTESIAN_POINT ( 'NONE',  ( -55.59585481156724285, 3.673546848079182414, 0.7533615035078059519 ) ) ;
#18523 = DIRECTION ( 'NONE',  ( 0.000000000000000000, 0.000000000000000000, 1.000000000000000000 ) ) ;
#18525 = VERTEX_POINT ( 'NONE', #22174 ) ;
#18526 = CARTESIAN_POINT ( 'NONE',  ( -58.86042740578360366, 3.725040285533370632, -1.239922660687675648 ) ) ;
#18527 = AXIS2_PLACEMENT_3D ( 'NONE', #23244, #30195, #21023 ) ;
#18528 = TOROIDAL_SURFACE ( 'NONE', #5376, 4.350000000000019185, 0.05000000000000000278 ) ;
#18529 = CARTESIAN_POINT ( 'NONE',  ( -60.49999999999996447, 3.526604974156013039, 0.7232270433674945487 ) ) ;
#18530 = SHAPE_DEFINITION_REPRESENTATION ( #30574, #1561 ) ;
#18531 = AXIS2_PLACEMENT_3D ( 'NONE', #24521, #9977, #2689 ) ;
#18532 = EDGE_CURVE ( 'NONE', #15307, #22261, #23057, .T. ) ;
#18533 = CARTESIAN_POINT ( 'NONE',  ( 52.27848606442668711, 4.392737230661539094, -1.555162892461804613 ) ) ;
#18534 = CARTESIAN_POINT ( 'NONE',  ( 51.84772254680353143, 0.6924618999072380543, -1.653428777428159968 ) ) ;
#18535 = ADVANCED_FACE ( 'NONE', ( #12 ), #2687, .F. ) ;
#18536 = CARTESIAN_POINT ( 'NONE',  ( 51.24099374247646921, -1.086790822298242087, 1.208135181987622486 ) ) ;
#18537 = EDGE_CURVE ( 'NONE', #14302, #15552, #8372, .T. ) ;
#18538 = ORIENTED_EDGE ( 'NONE', *, *, #21037, .T. ) ;
#18539 = AXIS2_PLACEMENT_3D ( 'NONE', #15390, #25039, #3370 ) ;
#18540 = CARTESIAN_POINT ( 'NONE',  ( 61.23837541685294639, 0.8927489269151840379, -1.767200183692393844 ) ) ;
#18541 = CARTESIAN_POINT ( 'NONE',  ( -59.30412500704678536, 3.195544065279134038, 1.250136525132556242 ) ) ;
#18542 = DIRECTION ( 'NONE',  ( -2.095850865446309212E-30, -1.000000000000000000, -2.891205793294679411E-15 ) ) ;
#18543 = AXIS2_PLACEMENT_3D ( 'NONE', #25423, #12087, #8636 ) ;
#18544 = CARTESIAN_POINT ( 'NONE',  ( 50.87477060347374902, 8.633605004118187765, 1.949999999999822320 ) ) ;
#18545 = AXIS2_PLACEMENT_3D ( 'NONE', #29053, #27296, #3076 ) ;
#18546 = CARTESIAN_POINT ( 'NONE',  ( 15.03925126672132784, 3.817150320980643663, 2.203324261490567704 ) ) ;
#18547 = AXIS2_PLACEMENT_3D ( 'NONE', #3348, #12679, #19686 ) ;
#18548 = CARTESIAN_POINT ( 'NONE',  ( 47.88109723283228192, -4.387164036186663729, -1.383037136012811308 ) ) ;
#18549 = AXIS2_PLACEMENT_3D ( 'NONE', #8664, #18819, #23727 ) ;
#18551 = DIRECTION ( 'NONE',  ( 1.000000000000000000, 1.047444401652940007E-14, 0.000000000000000000 ) ) ;
#18550 = DIRECTION ( 'NONE',  ( 1.000000000000000000, 3.053848253006669023E-16, -2.042510438544995415E-16 ) ) ;
#18552 = ORIENTED_EDGE ( 'NONE', *, *, #6648, .F. ) ;
#18553 = CARTESIAN_POINT ( 'NONE',  ( -54.39999999999997726, 8.366749974758487600E-15, -2.213041600731273397E-13 ) ) ;
#18554 = DIRECTION ( 'NONE',  ( -1.000000000000000000, -0.000000000000000000, -0.000000000000000000 ) ) ;
#18556 = CARTESIAN_POINT ( 'NONE',  ( 47.73697115155167126, -4.023893809447296910, -1.198232146805585874 ) ) ;
#18555 = CARTESIAN_POINT ( 'NONE',  ( 58.64999999999999147, 1.782657835994909901, 0.5811678240991509092 ) ) ;
#18557 = CARTESIAN_POINT ( 'NONE',  ( -35.85663232820583346, -5.377732432866659806, -0.5657657256215629094 ) ) ;
#18558 = EDGE_CURVE ( 'NONE', #29802, #21265, #14398, .T. ) ;
#18559 = ORIENTED_EDGE ( 'NONE', *, *, #21654, .F. ) ;
#18560 = CARTESIAN_POINT ( 'NONE',  ( 53.21917409580260028, 8.083376426877340037, 2.049999999999814637 ) ) ;
#18561 = DIRECTION ( 'NONE',  ( -0.000000000000000000, -0.000000000000000000, -1.000000000000000000 ) ) ;
#18562 = ORIENTED_EDGE ( 'NONE', *, *, #17334, .T. ) ;
#18563 = EDGE_CURVE ( 'NONE', #21195, #24661, #14943, .T. ) ;
#18564 = DIRECTION ( 'NONE',  ( 0.000000000000000000, 0.000000000000000000, 1.000000000000000000 ) ) ;
#18565 = CIRCLE ( 'NONE', #21662, 2.750000000000000444 ) ;
#18566 = ORIENTED_EDGE ( 'NONE', *, *, #12321, .T. ) ;
#18567 = CARTESIAN_POINT ( 'NONE',  ( 58.65000045311409593, 1.873226731664826117, 0.08323357347720464205 ) ) ;
#18568 = EDGE_LOOP ( 'NONE', ( #15545, #16859, #15528, #9778 ) ) ;
#18569 = AXIS2_PLACEMENT_3D ( 'NONE', #9323, #14367, #26562 ) ;
#18570 = CYLINDRICAL_SURFACE ( 'NONE', #29318, 1.000000000000000000 ) ;
#18571 = CARTESIAN_POINT ( 'NONE',  ( -57.89405989232411542, 2.944486372867106461, -1.700000000000192912 ) ) ;
#18572 = VERTEX_POINT ( 'NONE', #19646 ) ;
#18573 = VECTOR ( 'NONE', #7141, 1000.000000000000000 ) ;
#18574 = ORIENTED_EDGE ( 'NONE', *, *, #16600, .T. ) ;
#18575 = ORIENTED_EDGE ( 'NONE', *, *, #3647, .F. ) ;
#18576 = CLOSED_SHELL ( 'NONE', ( #9644, #13735, #6354, #7421, #6219, #18535, #8407, #14669, #26220, #6917, #19260, #29976, #11153, #30634, #29921, #8088, #23555, #16403, #1642, #27343, #5352, #29351, #11918, #6183, #4732, #12266, #18157, #12194, #23381, #4311, #19137, #21474, #5507, #26839, #12463, #12742, #11174, #155, #26363, #7361, #28696, #12711, #6123, #17495, #30887, #19264, #14087, #16307, #24188, #5553, #1392, #17929, #11618, #8883, #22644, #28210, #11565, #19362, #157, #26011, #17342, #12129, #10164, #9054, #11621, #16436, #1226, #21193, #17629, #21466, #28293, #20247, #10531, #16772, #22648, #30236, #24768, #2683, #29135, #24514, #30081, #17912, #20610, #25619, #17909, #30338, #11334, #26643, #19047, #13680, #25334, #4855, #5057, #23760, #20878, #7848 ) ) ;
#18577 = AXIS2_PLACEMENT_3D ( 'NONE', #19678, #2719, #7770 ) ;
#18578 = CARTESIAN_POINT ( 'NONE',  ( -55.57202994616207548, 2.078460969082646770, 3.599999999999810019 ) ) ;
#18579 = VECTOR ( 'NONE', #14568, 1000.000000000000000 ) ;
#18580 = AXIS2_PLACEMENT_3D ( 'NONE', #15257, #17325, #14787 ) ;
#18581 = DIRECTION ( 'NONE',  ( 3.489354422748178582E-15, -1.218509414717996338E-16, 1.000000000000000000 ) ) ;
#18582 = CARTESIAN_POINT ( 'NONE',  ( 30.02700392305999344, 6.560679691584628159, -1.425000000000105072 ) ) ;
#18583 = CYLINDRICAL_SURFACE ( 'NONE', #5918, 3.399999999999999911 ) ;
#18585 = PLANE ( 'NONE',  #13394 ) ;
#18584 = CARTESIAN_POINT ( 'NONE',  ( -36.14490256869206064, 5.374748457514291644, -0.5963382560599886917 ) ) ;
#18586 = AXIS2_PLACEMENT_3D ( 'NONE', #15820, #18523, #25472 ) ;
#18587 = CARTESIAN_POINT ( 'NONE',  ( 47.05963571244991783, 8.266527678078146479, 1.949999999999835865 ) ) ;
#18588 = DIRECTION ( 'NONE',  ( 1.000000000000000000, 3.054027077731387480E-16, -2.042479963029832083E-16 ) ) ;
#18589 = CARTESIAN_POINT ( 'NONE',  ( 15.86395258069111414, 5.320649567603495278, -0.9667173501063296426 ) ) ;
#18590 = DIRECTION ( 'NONE',  ( 0.000000000000000000, 0.000000000000000000, -1.000000000000000000 ) ) ;
#18592 = CARTESIAN_POINT ( 'NONE',  ( -56.72499999999997300, 3.116721586436802063E-15, -1.005743832985040150E-16 ) ) ;
#18591 = AXIS2_PLACEMENT_3D ( 'NONE', #28472, #11060, #16289 ) ;
#18593 = DIRECTION ( 'NONE',  ( 0.000000000000000000, 0.000000000000000000, -1.000000000000000000 ) ) ;
#18594 = ORIENTED_EDGE ( 'NONE', *, *, #16759, .F. ) ;
#18596 = CARTESIAN_POINT ( 'NONE',  ( 50.40000000000001990, -0.6462379109120509613, 4.048750000000022276 ) ) ;
#18595 = CARTESIAN_POINT ( 'NONE',  ( 50.59602332238209499, -0.1408342061598474859, 1.212874140286674285 ) ) ;
#18597 = EDGE_CURVE ( 'NONE', #26864, #25905, #17255, .T. ) ;
#18598 = EDGE_CURVE ( 'NONE', #22328, #8007, #13976, .T. ) ;
#18599 = AXIS2_PLACEMENT_3D ( 'NONE', #1840, #4213, #11333 ) ;
#18600 = EDGE_LOOP ( 'NONE', ( #2564, #16338, #8712, #1373 ) ) ;
#18601 = CIRCLE ( 'NONE', #4938, 0.04999999999999989175 ) ;
#18602 = EDGE_CURVE ( 'NONE', #1827, #1635, #30216, .T. ) ;
#18603 = CIRCLE ( 'NONE', #7452, 0.4576450603546999840 ) ;
#18604 = DIRECTION ( 'NONE',  ( 0.000000000000000000, 1.000000000000000000, 0.000000000000000000 ) ) ;
#18605 = DIRECTION ( 'NONE',  ( -1.168655815394902336E-14, 0.000000000000000000, -1.000000000000000000 ) ) ;
#18606 = CARTESIAN_POINT ( 'NONE',  ( -60.81249999999997868, -1.962990915244731793, 3.399999999999776090 ) ) ;
#18607 = ORIENTED_EDGE ( 'NONE', *, *, #12479, .F. ) ;
#18608 = VERTEX_POINT ( 'NONE', #22801 ) ;
#18609 = FACE_OUTER_BOUND ( 'NONE', #3526, .T. ) ;
#18610 = ORIENTED_EDGE ( 'NONE', *, *, #15291, .T. ) ;
#18611 = CARTESIAN_POINT ( 'NONE',  ( 58.65000000000003411, -1.571497941946663923, 1.022750809559922036 ) ) ;
#18612 = CARTESIAN_POINT ( 'NONE',  ( 50.93312545610844211, -0.6352506689584648258, 1.438808137080897165 ) ) ;
#18613 = ORIENTED_EDGE ( 'NONE', *, *, #25043, .F. ) ;
#18614 = DIRECTION ( 'NONE',  ( 3.489354422748178582E-15, -1.218509414717996338E-16, 1.000000000000000000 ) ) ;
#18615 = CARTESIAN_POINT ( 'NONE',  ( -35.85663232820584057, -3.426725943139554698, -3.937891353488750301 ) ) ;
#18616 = CARTESIAN_POINT ( 'NONE',  ( -54.49821982711414847, -3.342839925777855381, -1.196915030700223426 ) ) ;
#18617 = EDGE_LOOP ( 'NONE', ( #22144, #11255, #25087, #25714 ) ) ;
#18618 = ORIENTED_EDGE ( 'NONE', *, *, #30350, .F. ) ;
#18619 = CONICAL_SURFACE ( 'NONE', #7002, 2.765000000000001013, 0.03997868712329009228 ) ;
#18620 = ADVANCED_FACE ( 'NONE', ( #942 ), #1088, .F. ) ;
#18621 = CIRCLE ( 'NONE', #31244, 0.2500000000000000555 ) ;
#18622 = CARTESIAN_POINT ( 'NONE',  ( 47.01037571208187416, -4.157296476791674245, -1.048491968755484560 ) ) ;
#18623 = CARTESIAN_POINT ( 'NONE',  ( -55.77900635094609783, 3.400000000000004352, 0.9110272542656325800 ) ) ;
#18624 = CARTESIAN_POINT ( 'NONE',  ( 15.03925126672132784, 4.683225679163368405, -2.703237727951182112 ) ) ;
#18625 = CARTESIAN_POINT ( 'NONE',  ( -57.97085481156723574, 2.489203624310592389, -2.804704140674918911 ) ) ;
#18626 = CARTESIAN_POINT ( 'NONE',  ( 58.75000000000000711, 1.320082690053780983, 1.469015551797190788 ) ) ;
#18627 = FACE_BOUND ( 'NONE', #5322, .T. ) ;
#18628 = CARTESIAN_POINT ( 'NONE',  ( 58.75000000000003553, -1.499837071478441031, 1.323060376181713016 ) ) ;
#18630 = DIRECTION ( 'NONE',  ( 0.000000000000000000, 0.000000000000000000, -1.000000000000000000 ) ) ;
#18629 = SURFACE_STYLE_FILL_AREA ( #14170 ) ;
#18631 = DIRECTION ( 'NONE',  ( 0.000000000000000000, -1.000000000000000000, -4.379659758543257010E-15 ) ) ;
#18632 = CARTESIAN_POINT ( 'NONE',  ( -44.59999999999999432, 1.499999999999995781, 4.029888335921785192 ) ) ;
#18633 = CARTESIAN_POINT ( 'NONE',  ( 61.23793632918122398, -0.8908246368665424519, -1.774550402278997518 ) ) ;
#18634 = ORIENTED_EDGE ( 'NONE', *, *, #16589, .T. ) ;
#18635 = ORIENTED_EDGE ( 'NONE', *, *, #19827, .F. ) ;
#18636 = EDGE_CURVE ( 'NONE', #18736, #20389, #7877, .T. ) ;
#18637 = ORIENTED_EDGE ( 'NONE', *, *, #20143, .F. ) ;
#18638 = CARTESIAN_POINT ( 'NONE',  ( 51.06223082645568923, -3.930699233196520481, 1.170919866330858650 ) ) ;
#18639 = ORIENTED_EDGE ( 'NONE', *, *, #13848, .F. ) ;
#18640 = CARTESIAN_POINT ( 'NONE',  ( 54.23267447929808327, 6.619944661321486734, 2.049999999999810640 ) ) ;
#18641 = CARTESIAN_POINT ( 'NONE',  ( -58.65835481156723574, 4.108500314926515351, -1.367561758111407899 ) ) ;
#18642 = CARTESIAN_POINT ( 'NONE',  ( -36.26369610968607304, 2.881190829692216848, 4.334245811858008501 ) ) ;
#18643 = ORIENTED_EDGE ( 'NONE', *, *, #12677, .T. ) ;
#18644 = ORIENTED_EDGE ( 'NONE', *, *, #27542, .F. ) ;
#18645 = DIRECTION ( 'NONE',  ( 1.000000000000000000, 1.047444401652940007E-14, 0.000000000000000000 ) ) ;
#18646 = ORIENTED_EDGE ( 'NONE', *, *, #8668, .F. ) ;
#18647 = CARTESIAN_POINT ( 'NONE',  ( -44.49999999999999289, 1.399999999999995914, 3.959797974644454044 ) ) ;
#18648 = EDGE_LOOP ( 'NONE', ( #11661, #5112, #7867, #18678 ) ) ;
#18650 = FACE_OUTER_BOUND ( 'NONE', #29482, .T. ) ;
#18649 = DIRECTION ( 'NONE',  ( 0.000000000000000000, -1.000000000000000000, 0.000000000000000000 ) ) ;
#18651 = CARTESIAN_POINT ( 'NONE',  ( 41.48619405472009447, -151.3359592902261852, -1.550000000000163469 ) ) ;
#18652 = ORIENTED_EDGE ( 'NONE', *, *, #7190, .F. ) ;
#18653 = CARTESIAN_POINT ( 'NONE',  ( -35.85663232820595425, 5.340403872473318714, -0.9205822173395590280 ) ) ;
#18654 = CARTESIAN_POINT ( 'NONE',  ( 51.25000000000002842, -1.099999999999462963, -1.996089927833914146 ) ) ;
#18655 = EDGE_CURVE ( 'NONE', #24129, #30441, #12216, .T. ) ;
#18656 = DIRECTION ( 'NONE',  ( 0.000000000000000000, -1.000000000000000000, 0.000000000000000000 ) ) ;
#18657 = DIRECTION ( 'NONE',  ( 0.000000000000000000, 0.9996898646859347926, 0.02490330187379614924 ) ) ;
#18658 = CARTESIAN_POINT ( 'NONE',  ( -59.69702994616202574, -2.078460969082631227, -3.600000000000218137 ) ) ;
#18659 = CARTESIAN_POINT ( 'NONE',  ( -59.41132486540516311, 3.161828374300071687, 1.250136525132550691 ) ) ;
#18660 = CARTESIAN_POINT ( 'NONE',  ( 58.75000000000002132, 6.153735859711025284E-13, 3.111507638930570854E-58 ) ) ;
#18661 =( BOUNDED_CURVE ( )  B_SPLINE_CURVE ( 2, ( #19467, #9183, #23753, #24049, #6969 ),
 .UNSPECIFIED., .F., .T. ) 
 B_SPLINE_CURVE_WITH_KNOTS ( ( 3, 2, 3 ),
 ( 0.06011924821131572894, 0.07407407407407406996, 0.08333333333333332871 ),
 .UNSPECIFIED. ) 
 CURVE ( )  GEOMETRIC_REPRESENTATION_ITEM ( )  RATIONAL_B_SPLINE_CURVE ( ( 0.9502399529286075230, 0.8990420233480378442, 1.000000000000000000, 0.9330127018922194093, 0.9330127018922194093 ) ) 
 REPRESENTATION_ITEM ( '' )  );
#18662 = CARTESIAN_POINT ( 'NONE',  ( 50.39869454013827976, 0.9107929593200400076, -3.923749358243191043 ) ) ;
#18663 = CARTESIAN_POINT ( 'NONE',  ( -56.29792740578360366, -2.256877952708266299, 2.542931754211921191 ) ) ;
#18664 = DIRECTION ( 'NONE',  ( 0.000000000000000000, -0.9996898646859343485, -0.02490330187381124133 ) ) ;
#18665 = VERTEX_POINT ( 'NONE', #20420 ) ;
#18666 = CARTESIAN_POINT ( 'NONE',  ( -54.39999999999996305, 1.500000000000021316, -3.300094695611233142 ) ) ;
#18667 = CARTESIAN_POINT ( 'NONE',  ( 51.23644008536122385, 1.080112125196981854, 1.214076932077872817 ) ) ;
#18668 = CARTESIAN_POINT ( 'NONE',  ( -36.25997906085252254, 0.2181161761758398654, 5.200000001420970186 ) ) ;
#18669 = LINE ( 'NONE', #30997, #15022 ) ;
#18670 = ORIENTED_EDGE ( 'NONE', *, *, #1087, .T. ) ;
#18671 = EDGE_CURVE ( 'NONE', #4537, #15739, #6007, .T. ) ;
#18672 = DIRECTION ( 'NONE',  ( 0.9990482215818580203, -0.008762977932701932968, 0.04273009679227924434 ) ) ;
#18673 = VERTEX_POINT ( 'NONE', #27689 ) ;
#18674 = FACE_OUTER_BOUND ( 'NONE', #24548, .T. ) ;
#18676 = CARTESIAN_POINT ( 'NONE',  ( 58.65844932252308297, -1.349094575298446008, 1.302247349114806552 ) ) ;
#18675 = FACE_OUTER_BOUND ( 'NONE', #25160, .T. ) ;
#18677 = ORIENTED_EDGE ( 'NONE', *, *, #3852, .F. ) ;
#18678 = ORIENTED_EDGE ( 'NONE', *, *, #26940, .F. ) ;
#18679 = FACE_BOUND ( 'NONE', #1177, .T. ) ;
#18680 = AXIS2_PLACEMENT_3D ( 'NONE', #10616, #22494, #791 ) ;
#18681 = TOROIDAL_SURFACE ( 'NONE', #5017, 4.199999999999993072, 0.1000000000000000056 ) ;
#18682 = DIRECTION ( 'NONE',  ( -1.000000000000000000, 0.000000000000000000, 0.000000000000000000 ) ) ;
#18684 = DIRECTION ( 'NONE',  ( 1.000000000000000000, 3.053848253006669023E-16, -2.042510438544995415E-16 ) ) ;
#18683 = CARTESIAN_POINT ( 'NONE',  ( -60.63452994616204705, -3.117691453623976816, 1.799999999999772671 ) ) ;
#18685 = ORIENTED_EDGE ( 'NONE', *, *, #11955, .F. ) ;
#18686 = CARTESIAN_POINT ( 'NONE',  ( -56.49999999999997158, -2.489203624310585283, 2.804704140674916690 ) ) ;
#18687 = CARTESIAN_POINT ( 'NONE',  ( -36.40878371307408656, 3.917459231545620035, 3.727878977586848386 ) ) ;
#18688 = PRODUCT_CONTEXT ( 'NONE', #4261, 'mechanical' ) ;
#18689 = ADVANCED_FACE ( 'NONE', ( #29900, #15661 ), #13254, .T. ) ;
#18690 = CARTESIAN_POINT ( 'NONE',  ( 50.59602332238209499, 0.1408342061609074158, -1.212874140286673841 ) ) ;
#18691 = DIRECTION ( 'NONE',  ( -1.000000000000000000, 1.219044193948983948E-29, -3.491481338843133355E-15 ) ) ;
#18692 = CARTESIAN_POINT ( 'NONE',  ( -54.47710365256552478, 1.507983431629474014, -4.035431478432994545 ) ) ;
#18693 = CIRCLE ( 'NONE', #28788, 4.100000000000022737 ) ;
#18694 = ORIENTED_EDGE ( 'NONE', *, *, #24855, .F. ) ;
#18695 = CARTESIAN_POINT ( 'NONE',  ( 57.05000000000001847, -0.7500000000000000000, 1.778341924377873751 ) ) ;
#18696 =( BOUNDED_SURFACE ( )  B_SPLINE_SURFACE ( 3, 2, ( 
 ( #9983, #9818, #2551 ),
 ( #7144, #14254, #11731 ),
 ( #24383, #2693, #21878 ),
 ( #12332, #310, #16806 ),
 ( #21562, #9533, #7451 ),
 ( #28833, #4912, #29292 ),
 ( #165, #19, #7604 ),
 ( #17260, #26903, #5214 ),
 ( #2067, #6993, #21728 ),
 ( #12199, #9357, #14403 ) ),
 .UNSPECIFIED., .F., .F., .F. ) 
 B_SPLINE_SURFACE_WITH_KNOTS ( ( 4, 2, 2, 2, 4 ),
 ( 3, 3 ),
 ( 0.0001706658715701054685, 0.0002229276920781130141, 0.0002751895125861205868, 0.0003274513330941281053, 0.0003797131536021356780 ),
 ( 0.000000000000000000, 1.000000000000000000 ),
 .UNSPECIFIED. ) 
 GEOMETRIC_REPRESENTATION_ITEM ( )  RATIONAL_B_SPLINE_SURFACE ( (
 ( 1.000000000000000000, 0.7071067811873459341, 1.000000000000000000),
 ( 1.000000000000000000, 0.7375607040706478879, 1.000000000000000000),
 ( 1.000000000000000000, 0.7730431127430092975, 1.000000000000000000),
 ( 1.000000000000000000, 0.8321012486969630029, 1.000000000000000000),
 ( 1.000000000000000000, 0.8541932017383955245, 1.000000000000000000),
 ( 1.000000000000000000, 0.8545723906030464612, 1.000000000000000000),
 ( 1.000000000000000000, 0.8327032135025188575, 1.000000000000000000),
 ( 1.000000000000000000, 0.7734559727053201827, 1.000000000000000000),
 ( 1.000000000000000000, 0.7377766653992472445, 1.000000000000000000),
 ( 1.000000000000000000, 0.7071067811865522357, 1.000000000000000000) ) ) 
 REPRESENTATION_ITEM ( '' )  SURFACE ( )  );
#18697 = AXIS2_PLACEMENT_3D ( 'NONE', #6788, #9178, #11851 ) ;
#18698 = CARTESIAN_POINT ( 'NONE',  ( 61.24919886530818758, 0.9685650917412264027, -1.667277206150558966 ) ) ;
#18699 = CARTESIAN_POINT ( 'NONE',  ( -44.49999999999997868, 1.499999999999999556, -4.029888335921975262 ) ) ;
#18700 = DIRECTION ( 'NONE',  ( 3.083952846180964840E-15, 0.000000000000000000, 1.000000000000000000 ) ) ;
#18701 = ADVANCED_FACE ( 'NONE', ( #1228 ), #10890, .T. ) ;
#18702 = AXIS2_PLACEMENT_3D ( 'NONE', #3170, #22199, #15205 ) ;
#18703 = CARTESIAN_POINT ( 'NONE',  ( 15.32766723174653301, 1.093755498983968399, -5.295967089285809948 ) ) ;
#18704 = CIRCLE ( 'NONE', #10105, 0.4576450603546982632 ) ;
#18705 = AXIS2_PLACEMENT_3D ( 'NONE', #3958, #3645, #30244 ) ;
#18707 = CARTESIAN_POINT ( 'NONE',  ( 58.65844932252326061, -1.802326573993413561, -0.5172264997589001156 ) ) ;
#18706 = CARTESIAN_POINT ( 'NONE',  ( 50.93312545610843500, -0.6352506689584650479, -1.438808137080897165 ) ) ;
#18709 = CIRCLE ( 'NONE', #19219, 1.875000000000001776 ) ;
#18708 = CARTESIAN_POINT ( 'NONE',  ( -62.09999999999997300, -2.665234058423473495, -0.3155123021236101999 ) ) ;
#18711 = CARTESIAN_POINT ( 'NONE',  ( -59.69999999999997442, 3.264622394567738617, -1.238538609462263240 ) ) ;
#18710 = FACE_OUTER_BOUND ( 'NONE', #23200, .T. ) ;
#18712 = ORIENTED_EDGE ( 'NONE', *, *, #29868, .T. ) ;
#18713 = EDGE_CURVE ( 'NONE', #6507, #31094, #612, .T. ) ;
#18714 = CARTESIAN_POINT ( 'NONE',  ( 61.25000000000000000, 1.800471618824466935, 1.039502773797588597 ) ) ;
#18715 = DIRECTION ( 'NONE',  ( 1.000000000000000000, 2.586136946169074517E-16, -0.000000000000000000 ) ) ;
#18717 = CARTESIAN_POINT ( 'NONE',  ( -36.25997906085275702, 5.012895491272595372, 1.399447560527683931 ) ) ;
#18716 = LINE ( 'NONE', #18247, #22170 ) ;
#18718 = CARTESIAN_POINT ( 'NONE',  ( 51.25000000000001421, 0.9938153758931693726, 1.589954715908409755 ) ) ;
#18719 = EDGE_LOOP ( 'NONE', ( #15724, #24806, #29995, #2427 ) ) ;
#18720 = ORIENTED_EDGE ( 'NONE', *, *, #20074, .F. ) ;
#18721 = CARTESIAN_POINT ( 'NONE',  ( -36.30424252565902776, -4.979756346315149962, 1.501439362221238083 ) ) ;
#18722 = CARTESIAN_POINT ( 'NONE',  ( 50.40000000000001279, -0.7619326981554289668, 3.939508824314739144 ) ) ;
#18723 = EDGE_LOOP ( 'NONE', ( #143, #27750, #8186, #785 ) ) ;
#18724 = CARTESIAN_POINT ( 'NONE',  ( -59.69999999999997442, 8.366749974758454467E-15, -2.120534355533670266E-13 ) ) ;
#18725 = ORIENTED_EDGE ( 'NONE', *, *, #1402, .T. ) ;
#18726 = CARTESIAN_POINT ( 'NONE',  ( 58.65838214097842496, 1.874774200234571087, -0.03350837198745684753 ) ) ;
#18727 = EDGE_LOOP ( 'NONE', ( #22006, #888, #26706, #1096 ) ) ;
#18728 = CARTESIAN_POINT ( 'NONE',  ( -55.57202994616207548, 2.078460969082644105, 3.599999999999811351 ) ) ;
#18729 = AXIS2_PLACEMENT_3D ( 'NONE', #26844, #406, #5293 ) ;
#18730 = EDGE_CURVE ( 'NONE', #22370, #518, #21169, .T. ) ;
#18731 = CARTESIAN_POINT ( 'NONE',  ( -56.08155989232413674, -1.962990915244731571, 3.399999999999792077 ) ) ;
#18732 = ORIENTED_EDGE ( 'NONE', *, *, #29449, .F. ) ;
#18733 = SURFACE_SIDE_STYLE ('',( #7164 ) ) ;
#18734 = VERTEX_POINT ( 'NONE', #27370 ) ;
#18735 = TOROIDAL_SURFACE ( 'NONE', #17214, 4.200000000000016165, 0.1000000000000000056 ) ;
#18736 = VERTEX_POINT ( 'NONE', #5529 ) ;
#18737 = AXIS2_PLACEMENT_3D ( 'NONE', #29997, #16071, #25724 ) ;
#18738 = CARTESIAN_POINT ( 'NONE',  ( -61.12499999999995737, 2.944486372867106905, -1.700000000000204459 ) ) ;
#18739 = CARTESIAN_POINT ( 'NONE',  ( 56.97354279652698494, -0.7803351525568237301, 2.480154250529269522 ) ) ;
#18740 = FACE_OUTER_BOUND ( 'NONE', #5723, .T. ) ;
#18741 = DIRECTION ( 'NONE',  ( -1.000000000000000000, -3.054025858079668409E-16, 2.042474015755241579E-16 ) ) ;
#18742 = ADVANCED_FACE ( 'NONE', ( #15182 ), #24834, .F. ) ;
#18743 = CARTESIAN_POINT ( 'NONE',  ( 61.19881854997407800, 0.7436933986918214945, 1.660788881864679212 ) ) ;
#18744 = EDGE_CURVE ( 'NONE', #2592, #17201, #20031, .T. ) ;
#18746 = DIRECTION ( 'NONE',  ( 1.000000000000000000, 0.000000000000000000, -1.047444401652940007E-14 ) ) ;
#18745 = FILL_AREA_STYLE ('',( #30585 ) ) ;
#18747 = DIRECTION ( 'NONE',  ( 0.000000000000000000, 1.000000000000000000, 3.491481338843132961E-15 ) ) ;
#18748 = DIRECTION ( 'NONE',  ( 1.000000000000000000, 0.000000000000000000, 0.000000000000000000 ) ) ;
#18749 = CARTESIAN_POINT ( 'NONE',  ( 51.80000000000002558, 6.475000000000061817, 1.949999999999818767 ) ) ;
#18750 = CARTESIAN_POINT ( 'NONE',  ( 56.99032252660322939, 0.7964187825544630783, 2.475026498169530687 ) ) ;
#18751 = B_SPLINE_CURVE_WITH_KNOTS ( 'NONE', 3,
 ( #25531, #21135, #30766, #9075, #13326, #23190, #30438, #18750, #11277, #1617, #23021, #25388, #6696, #11611, #18278, #16357 ),
 .UNSPECIFIED., .F., .F.,
 ( 4, 3, 3, 3, 3, 4 ),
 ( 0.000000000000000000, 1.754151282668922588E-05, 5.222880005687533889E-05, 8.869434694929045231E-05, 0.0001259176481356621589, 0.0001632567749836554797 ),
 .UNSPECIFIED. ) ;
#18752 = EDGE_CURVE ( 'NONE', #30275, #24434, #15331, .T. ) ;
#18753 = CARTESIAN_POINT ( 'NONE',  ( 50.34130827207516745, 1.344780351710889610, -3.858600739747802599 ) ) ;
#18754 = ORIENTED_EDGE ( 'NONE', *, *, #30491, .T. ) ;
#18756 = DIRECTION ( 'NONE',  ( -2.614375865348240525E-16, 0.2008964009354147762, -0.9796124928211140670 ) ) ;
#18755 = CARTESIAN_POINT ( 'NONE',  ( 47.00000000000002132, -1.391941090707485396, -3.750000000000022649 ) ) ;
#18757 = EDGE_CURVE ( 'NONE', #15131, #10599, #11399, .T. ) ;
#18758 = CYLINDRICAL_SURFACE ( 'NONE', #19561, 2.000000000000000000 ) ;
#18759 = VERTEX_POINT ( 'NONE', #30681 ) ;
#18760 = CARTESIAN_POINT ( 'NONE',  ( -60.92292740578359656, 1.073804522883521351, 3.225979517392337570 ) ) ;
#18761 = CARTESIAN_POINT ( 'NONE',  ( -60.49999999999995737, 2.023778652682511576E-14, -3.400000000000214850 ) ) ;
#18762 = ORIENTED_EDGE ( 'NONE', *, *, #9032, .F. ) ;
#18763 = ORIENTED_EDGE ( 'NONE', *, *, #29868, .F. ) ;
#18764 = DIRECTION ( 'NONE',  ( 1.000000000000000000, -1.219044193948983948E-29, 3.491481338843133355E-15 ) ) ;
#18765 = ORIENTED_EDGE ( 'NONE', *, *, #9349, .T. ) ;
#18766 = CYLINDRICAL_SURFACE ( 'NONE', #5326, 4.099999999999992539 ) ;
#18767 = EDGE_LOOP ( 'NONE', ( #4400, #24691 ) ) ;
#18768 = CARTESIAN_POINT ( 'NONE',  ( 69.00000000000005684, 4.557543281186736018E-17, 3.020710678117923376 ) ) ;
#18769 = DIRECTION ( 'NONE',  ( 0.000000000000000000, 0.000000000000000000, -1.000000000000000000 ) ) ;
#18770 = CARTESIAN_POINT ( 'NONE',  ( 57.00000000000001421, 0.6999999999999999556, 2.489477856900920383 ) ) ;
#18771 = ORIENTED_EDGE ( 'NONE', *, *, #969, .T. ) ;
#18772 = ORIENTED_EDGE ( 'NONE', *, *, #23699, .T. ) ;
#18773 = LINE ( 'NONE', #16384, #16805 ) ;
#18774 = DIRECTION ( 'NONE',  ( 0.000000000000000000, -1.000000000000000000, 0.000000000000000000 ) ) ;
#18775 = CARTESIAN_POINT ( 'NONE',  ( 56.95000000000001705, -0.7255611966503594523, -2.496740365009429752 ) ) ;
#18776 = ORIENTED_EDGE ( 'NONE', *, *, #775, .F. ) ;
#18777 = AXIS2_PLACEMENT_3D ( 'NONE', #16971, #19963, #10000 ) ;
#18778 = DIRECTION ( 'NONE',  ( 1.000000000000000000, 1.047444401652940007E-14, 0.000000000000000000 ) ) ;
#18779 = EDGE_CURVE ( 'NONE', #24434, #3601, #1788, .T. ) ;
#18780 = CARTESIAN_POINT ( 'NONE',  ( 58.72419296898077334, 1.293880926823876676, 1.357170036000481916 ) ) ;
#18781 = EDGE_CURVE ( 'NONE', #3236, #30643, #5733, .T. ) ;
#18782 = FACE_OUTER_BOUND ( 'NONE', #9061, .T. ) ;
#18783 = EDGE_CURVE ( 'NONE', #20516, #8800, #17492, .T. ) ;
#18784 = CARTESIAN_POINT ( 'NONE',  ( 57.03469936322583322, 0.7478111487523275702, -1.780306085601951027 ) ) ;
#18786 = FACE_OUTER_BOUND ( 'NONE', #15595, .T. ) ;
#18785 = CARTESIAN_POINT ( 'NONE',  ( -35.85663232820579793, -2.199885893005965709, 4.939696249117681681 ) ) ;
#18787 = CARTESIAN_POINT ( 'NONE',  ( 63.50000000000005684, 2.908536147974998226E-16, 2.374999999999333422 ) ) ;
#18788 = CARTESIAN_POINT ( 'NONE',  ( -56.06249999999997868, 4.108500314926513575, -1.367561758111403680 ) ) ;
#18789 = DIRECTION ( 'NONE',  ( 0.000000000000000000, -0.2008964009354146929, 0.9796124928211140670 ) ) ;
#18790 = VERTEX_POINT ( 'NONE', #25776 ) ;
#18791 = VECTOR ( 'NONE', #28324, 1000.000000000000000 ) ;
#18792 = ORIENTED_EDGE ( 'NONE', *, *, #23122, .T. ) ;
#18793 = B_SPLINE_CURVE_WITH_KNOTS ( 'NONE', 3,
 ( #7248, #21982, #19155, #9319 ),
 .UNSPECIFIED., .F., .F.,
 ( 4, 4 ),
 ( 2.928550287019058723E-17, 7.626196476045024651E-05 ),
 .UNSPECIFIED. ) ;
#18794 = VERTEX_POINT ( 'NONE', #9313 ) ;
#18795 = CARTESIAN_POINT ( 'NONE',  ( -59.10064013560211293, -2.331281186115777615, 1.260011170057584451 ) ) ;
#18796 = ORIENTED_EDGE ( 'NONE', *, *, #10028, .F. ) ;
#18797 = CARTESIAN_POINT ( 'NONE',  ( 53.71392934491858995, 7.814769211952036443, 2.049999999999812417 ) ) ;
#18798 = CARTESIAN_POINT ( 'NONE',  ( -56.03335481156723574, -4.108500314926510022, 1.367561758111407455 ) ) ;
#18800 = CARTESIAN_POINT ( 'NONE',  ( 51.06494979651333210, -4.023708852620672793, -1.198807875231533426 ) ) ;
#18799 = CARTESIAN_POINT ( 'NONE',  ( -56.67499999999996874, 3.131991715727200307E-15, -1.107867533772800737E-16 ) ) ;
#18801 = ORIENTED_EDGE ( 'NONE', *, *, #9337, .F. ) ;
#18802 = ORIENTED_EDGE ( 'NONE', *, *, #4075, .F. ) ;
#18803 = DIRECTION ( 'NONE',  ( 0.000000000000000000, 0.000000000000000000, 1.000000000000000000 ) ) ;
#18804 = ORIENTED_EDGE ( 'NONE', *, *, #5935, .F. ) ;
#18805 = CARTESIAN_POINT ( 'NONE',  ( -67.99999999999995737, -3.266925685480207642E-16, 2.202315069465528948E-15 ) ) ;
#18806 = ORIENTED_EDGE ( 'NONE', *, *, #5826, .T. ) ;
#18808 = DIRECTION ( 'NONE',  ( 2.581436205204234006E-16, -0.9796124928211140670, -0.2008964009354148872 ) ) ;
#18807 = CARTESIAN_POINT ( 'NONE',  ( -36.89831264271881395, 5.226279933021899637, 1.394410282272850132 ) ) ;
#18809 = ORIENTED_EDGE ( 'NONE', *, *, #11756, .F. ) ;
#18810 = DIRECTION ( 'NONE',  ( 1.000000000000000000, 3.054025858079668409E-16, -2.042474015755241579E-16 ) ) ;
#18811 = CARTESIAN_POINT ( 'NONE',  ( 58.72427158855716556, 1.798991944512857710, -0.5288318043120886491 ) ) ;
#18812 = CARTESIAN_POINT ( 'NONE',  ( -36.14490256869205353, 1.093737229520459486, -5.295968199484771155 ) ) ;
#18813 = CIRCLE ( 'NONE', #15766, 0.04999999999999449329 ) ;
#18814 = CARTESIAN_POINT ( 'NONE',  ( 51.13341687362767374, 0.9248174436480008920, -1.495576127286106560 ) ) ;
#18815 = CARTESIAN_POINT ( 'NONE',  ( -58.44702994616205416, -2.078460969082657872, 3.599999999999784261 ) ) ;
#18816 = CARTESIAN_POINT ( 'NONE',  ( 51.88150799779677413, 0.02572195732724835704, 4.373259675815027947 ) ) ;
#18817 = EDGE_CURVE ( 'NONE', #27508, #1976, #3317, .T. ) ;
#18818 = AXIS2_PLACEMENT_3D ( 'NONE', #29240, #22280, #2783 ) ;
#18819 = DIRECTION ( 'NONE',  ( 1.000000000000000000, 3.054025858079668409E-16, -2.042474015755241579E-16 ) ) ;
#18820 = CARTESIAN_POINT ( 'NONE',  ( 58.45000000000001705, 0.8000000000000000444, 2.421260002560650104 ) ) ;
#18821 = CARTESIAN_POINT ( 'NONE',  ( -56.42292740578360366, 1.073804522883514689, 3.225979517392338902 ) ) ;
#18822 = CARTESIAN_POINT ( 'NONE',  ( -77.28999999999996362, 0.4498604391086670762, 0.01120648584322041577 ) ) ;
#18823 = VERTEX_POINT ( 'NONE', #18822 ) ;
#18824 = B_SPLINE_CURVE_WITH_KNOTS ( 'NONE', 3,
 ( #23293, #31194, #28188, #6500, #28500, #9029, #25810, #23440, #1727, #11395, #4266, #21084, #30724, #18703, #17398, #22173 ),
 .UNSPECIFIED., .F., .F.,
 ( 4, 2, 2, 2, 2, 2, 2, 4 ),
 ( 1.748223473168675632E-18, 0.0004351083927046442705, 0.0008702167854092868063, 0.001740433570818572312, 0.002175541963523215227, 0.002610650356227857492, 0.003045758748932500190, 0.003480867141637142888 ),
 .UNSPECIFIED. ) ;
#18825 = DIRECTION ( 'NONE',  ( -3.491481338843133355E-15, -3.491481338843133355E-15, 1.000000000000000000 ) ) ;
#18826 = CARTESIAN_POINT ( 'NONE',  ( -59.69999999999996732, -1.873569517744609447, -3.074042495181142698 ) ) ;
#18827 = CARTESIAN_POINT ( 'NONE',  ( -36.89017861347081606, 0.3252614978953461411, 5.399488438498862841 ) ) ;
#18828 = CARTESIAN_POINT ( 'NONE',  ( 48.41509867277373047, 1.114141714781645254, -3.896173399896523559 ) ) ;
#18829 = VERTEX_POINT ( 'NONE', #8667 ) ;
#18830 = EDGE_CURVE ( 'NONE', #26982, #14402, #30843, .T. ) ;
#18831 = CARTESIAN_POINT ( 'NONE',  ( 58.64999999999999858, 1.571497941946486065, 1.022750809562083640 ) ) ;
#18832 = ORIENTED_EDGE ( 'NONE', *, *, #22250, .F. ) ;
#18833 = CARTESIAN_POINT ( 'NONE',  ( 51.87673771347597551, 8.672480599449025718, 2.049999999999819522 ) ) ;
#18834 = AXIS2_PLACEMENT_3D ( 'NONE', #16269, #13716, #15939 ) ;
#18836 = CARTESIAN_POINT ( 'NONE',  ( 57.05000000000001847, -0.6999999999999999556, 0.000000000000000000 ) ) ;
#18835 = CARTESIAN_POINT ( 'NONE',  ( 58.75000018803717694, 1.010830333487790167, -1.651902078982614208 ) ) ;
#18837 = ORIENTED_EDGE ( 'NONE', *, *, #31135, .F. ) ;
#18838 = ORIENTED_EDGE ( 'NONE', *, *, #22298, .F. ) ;
#18839 = CARTESIAN_POINT ( 'NONE',  ( -35.85663232820584057, -0.4576450603547173035, -5.200000000000000178 ) ) ;
#18840 = CARTESIAN_POINT ( 'NONE',  ( -62.34999999999997300, -2.799131621120615421, -0.06972924524666888890 ) ) ;
#18842 = CARTESIAN_POINT ( 'NONE',  ( 61.09423418604048095, 0.6373668173476213505, -1.895722432252298084 ) ) ;
#18841 = DIRECTION ( 'NONE',  ( 0.000000000000000000, 0.000000000000000000, -1.000000000000000000 ) ) ;
#18843 = EDGE_LOOP ( 'NONE', ( #29264, #15573, #30228, #22885 ) ) ;
#18844 = CARTESIAN_POINT ( 'NONE',  ( -56.24999999999997158, -1.184343223768585363, -3.558065644182724085 ) ) ;
#18845 = DIRECTION ( 'NONE',  ( 1.000000000000000000, 0.000000000000000000, -1.047444401652940007E-14 ) ) ;
#18846 = CARTESIAN_POINT ( 'NONE',  ( 50.35762544161296006, 8.151359338959888845, 1.949999999999825206 ) ) ;
#18847 = DIRECTION ( 'NONE',  ( -1.000000000000000000, -0.000000000000000000, 0.000000000000000000 ) ) ;
#18848 = CARTESIAN_POINT ( 'NONE',  ( -54.39999999999999147, -1.500000000000004441, 3.300094695610789941 ) ) ;
#18849 =( BOUNDED_SURFACE ( )  B_SPLINE_SURFACE ( 3, 2, ( 
 ( #22048, #7769, #14747 ),
 ( #15216, #3029, #9847 ),
 ( #17287, #7480, #17434 ),
 ( #12524, #496, #24407 ),
 ( #27083, #10155, #3180 ),
 ( #5404, #2718, #19822 ) ),
 .UNSPECIFIED., .F., .F., .F. ) 
 B_SPLINE_SURFACE_WITH_KNOTS ( ( 4, 2, 4 ),
 ( 3, 3 ),
 ( 0.0001319104779587709254, 0.0002905946498119449514, 0.0004492788216651189773 ),
 ( 0.000000000000000000, 1.000000000000000000 ),
 .UNSPECIFIED. ) 
 GEOMETRIC_REPRESENTATION_ITEM ( )  RATIONAL_B_SPLINE_SURFACE ( (
 ( 1.000000000000000000, 0.7779866052154992273, 1.000000000000000000),
 ( 1.000000000000000000, 0.7780052684394707097, 1.000000000000000000),
 ( 1.000000000000000000, 0.7724636952541394930, 1.000000000000000000),
 ( 1.000000000000000000, 0.7490013934200028256, 1.000000000000000000),
 ( 1.000000000000000000, 0.7305684325697047177, 1.000000000000000000),
 ( 1.000000000000000000, 0.7071067811865716646, 1.000000000000000000) ) ) 
 REPRESENTATION_ITEM ( '' )  SURFACE ( )  );
#18851 = CARTESIAN_POINT ( 'NONE',  ( -54.47328085509070661, 1.505517457405397774, -4.033720452520548783 ) ) ;
#18850 = AXIS2_PLACEMENT_3D ( 'NONE', #997, #13467, #28650 ) ;
#18852 = VERTEX_POINT ( 'NONE', #16607 ) ;
#18853 = EDGE_CURVE ( 'NONE', #19651, #19672, #14458, .T. ) ;
#18854 = CARTESIAN_POINT ( 'NONE',  ( -67.34999999999998010, -4.352537305703398686E-16, 3.270044734337918230E-15 ) ) ;
#18855 = CARTESIAN_POINT ( 'NONE',  ( -36.26369610968610147, 3.231775792180371809, -4.079530926931222545 ) ) ;
#18856 = DIRECTION ( 'NONE',  ( 0.9913331294122580406, 0.1313720918981625962, 0.000000000000000000 ) ) ;
#18857 = FACE_OUTER_BOUND ( 'NONE', #11372, .T. ) ;
#18858 = CARTESIAN_POINT ( 'NONE',  ( 57.00103033359725657, -0.7116617362530316404, -2.445288145576760552 ) ) ;
#18860 = DIRECTION ( 'NONE',  ( 1.000000000000000000, -1.219044193948983948E-29, 3.491481338843133355E-15 ) ) ;
#18859 = CYLINDRICAL_SURFACE ( 'NONE', #9984, 4.299999999999998046 ) ;
#18861 = DIRECTION ( 'NONE',  ( 0.000000000000000000, 0.000000000000000000, -1.000000000000000000 ) ) ;
#18863 = FACE_BOUND ( 'NONE', #22105, .T. ) ;
#18862 = DIRECTION ( 'NONE',  ( 0.000000000000000000, 0.02490330187380866006, -0.9996898646859344595 ) ) ;
#18864 = EDGE_LOOP ( 'NONE', ( #24315, #18, #18139, #19710 ) ) ;
#18865 = EDGE_CURVE ( 'NONE', #23750, #27662, #2328, .T. ) ;
#18866 = CARTESIAN_POINT ( 'NONE',  ( 61.23770293222996486, -0.8897917884435792013, -1.791164585742600179 ) ) ;
#18867 = CARTESIAN_POINT ( 'NONE',  ( 51.45655683570191741, -0.9591657938390835136, 1.518428463906027037 ) ) ;
#18868 = AXIS2_PLACEMENT_3D ( 'NONE', #7186, #28878, #12242 ) ;
#18870 = CARTESIAN_POINT ( 'NONE',  ( -36.38012252111052902, 5.369990034204258578, 0.6654225812210384783 ) ) ;
#18869 = CARTESIAN_POINT ( 'NONE',  ( 15.45522337368515764, -2.900433254920993242, -4.320265374240207734 ) ) ;
#18871 = CARTESIAN_POINT ( 'NONE',  ( 15.94709373951294218, -5.297368390263452298, 1.087079755157607242 ) ) ;
#18872 = VERTEX_POINT ( 'NONE', #26087 ) ;
#18873 = ORIENTED_EDGE ( 'NONE', *, *, #3255, .T. ) ;
#18874 = CARTESIAN_POINT ( 'NONE',  ( 48.46289871413547701, 1.426739617975221863, 3.843750000000023981 ) ) ;
#18875 = PLANE ( 'NONE',  #693 ) ;
#18876 = EDGE_LOOP ( 'NONE', ( #16007, #6455, #19735, #19325, #20966, #1620 ) ) ;
#18877 = DIRECTION ( 'NONE',  ( 1.000000000000000000, 3.053848253006669023E-16, -2.042510438544995415E-16 ) ) ;
#18878 = ORIENTED_EDGE ( 'NONE', *, *, #4131, .F. ) ;
#18879 = DIRECTION ( 'NONE',  ( -1.000000000000000000, -3.054025858079668409E-16, 2.042474015755241579E-16 ) ) ;
#18880 = ORIENTED_EDGE ( 'NONE', *, *, #18655, .T. ) ;
#18881 = CARTESIAN_POINT ( 'NONE',  ( -60.64405989232412253, -3.920666489018283614E-15, 3.399999999999783640 ) ) ;
#18882 = FILL_AREA_STYLE_COLOUR ( '', #4475 ) ;
#18883 = EDGE_LOOP ( 'NONE', ( #12211, #27316, #23930, #2536 ) ) ;
#18884 = ORIENTED_EDGE ( 'NONE', *, *, #25955, .F. ) ;
#18885 = EDGE_CURVE ( 'NONE', #6477, #26303, #20762, .T. ) ;
#18886 = CARTESIAN_POINT ( 'NONE',  ( -59.43749999999997868, 1.962990915244722689, 3.399999999999796962 ) ) ;
#18887 = EDGE_CURVE ( 'NONE', #8527, #14388, #14049, .T. ) ;
#18888 = CARTESIAN_POINT ( 'NONE',  ( -59.19999999999996732, 4.156921938165317520, -0.9498634748674451567 ) ) ;
#18889 = CARTESIAN_POINT ( 'NONE',  ( 24.34823467037698919, 5.521868380698613521, -1.425000000000085087 ) ) ;
#18890 = CIRCLE ( 'NONE', #3698, 0.1000000000000001166 ) ;
#18892 = EDGE_CURVE ( 'NONE', #16720, #15457, #18518, .T. ) ;
#18891 = DIRECTION ( 'NONE',  ( -1.047444401652940007E-14, 0.000000000000000000, -1.000000000000000000 ) ) ;
#18893 = CIRCLE ( 'NONE', #7748, 2.000000000000000000 ) ;
#18894 = CARTESIAN_POINT ( 'NONE',  ( 50.25000000000000711, 1.323060376181234510, 1.499837071479058981 ) ) ;
#18896 = CARTESIAN_POINT ( 'NONE',  ( 58.45000000000001705, 0.8000000000000000444, -2.421260002560650104 ) ) ;
#18895 = SURFACE_STYLE_USAGE ( .BOTH. , #13956 ) ;
#18897 = FACE_OUTER_BOUND ( 'NONE', #15817, .T. ) ;
#18898 = CARTESIAN_POINT ( 'NONE',  ( 49.00000000000000000, 0.7500000000000000000, -1.988246715073871629 ) ) ;
#18899 = CARTESIAN_POINT ( 'NONE',  ( 15.03925126672125145, 5.340403872473335589, -0.9205822173395469266 ) ) ;
#18900 = CARTESIAN_POINT ( 'NONE',  ( 58.75000000000003553, -1.749377236608634645, -0.8979909453698914357 ) ) ;
#18901 = EDGE_CURVE ( 'NONE', #27318, #26116, #4854, .T. ) ;
#18902 = DIRECTION ( 'NONE',  ( -1.000000000000000000, 1.219044193948983948E-29, -3.491481338843133355E-15 ) ) ;
#18903 = CARTESIAN_POINT ( 'NONE',  ( 61.05375305192653457, -0.5989395831096625544, 1.861793349153599397 ) ) ;
#18904 = ORIENTED_EDGE ( 'NONE', *, *, #28988, .T. ) ;
#18906 = CARTESIAN_POINT ( 'NONE',  ( -54.39999999999997726, -4.766731106216463600E-14, -1.831402436016377855E-13 ) ) ;
#18905 = DIRECTION ( 'NONE',  ( 0.000000000000000000, 0.000000000000000000, -1.000000000000000000 ) ) ;
#18907 = CARTESIAN_POINT ( 'NONE',  ( 54.22843442268823821, 6.361173098464514730, -2.050000000000188116 ) ) ;
#18908 = CARTESIAN_POINT ( 'NONE',  ( 68.00000000000005684, 4.286263797014710090E-16, 3.499999999999287681 ) ) ;
#18909 = ORIENTED_EDGE ( 'NONE', *, *, #6982, .F. ) ;
#18910 = CARTESIAN_POINT ( 'NONE',  ( 22.54717926605049172, 7.740376438784041468, 1.424999999999921219 ) ) ;
#18911 = AXIS2_PLACEMENT_3D ( 'NONE', #16099, #23531, #18004 ) ;
#18912 = CARTESIAN_POINT ( 'NONE',  ( 29.69543387591359362, 6.938696499881336521, 1.424999999999896572 ) ) ;
#18913 = CARTESIAN_POINT ( 'NONE',  ( -54.57202994616205416, -4.156921938165296204, -2.089175772356712570E-13 ) ) ;
#18914 = ORIENTED_EDGE ( 'NONE', *, *, #22419, .F. ) ;
#18915 = EDGE_CURVE ( 'NONE', #14055, #17250, #14421, .T. ) ;
#18916 = VERTEX_POINT ( 'NONE', #23259 ) ;
#18917 = AXIS2_PLACEMENT_3D ( 'NONE', #25679, #28040, #15562 ) ;
#18918 = CARTESIAN_POINT ( 'NONE',  ( 15.29384114148383667, 4.822476035523743931, 1.985498375066824472 ) ) ;
#18919 = ORIENTED_EDGE ( 'NONE', *, *, #22937, .T. ) ;
#18920 = CARTESIAN_POINT ( 'NONE',  ( 58.75000018595672202, -1.651828233789423450, 1.011330950598698042 ) ) ;
#18921 = CARTESIAN_POINT ( 'NONE',  ( -57.07202994616206126, 2.078460969082646770, 3.599999999999804690 ) ) ;
#18922 = EDGE_LOOP ( 'NONE', ( #22610, #13265, #7708, #14176 ) ) ;
#18923 = DIRECTION ( 'NONE',  ( -0.9926670569371678354, -0.1208805777273652682, -2.408208294782601816E-14 ) ) ;
#18924 = DIRECTION ( 'NONE',  ( 1.000000000000000000, 3.053848253006669023E-16, -2.042510438544995415E-16 ) ) ;
#18925 = CARTESIAN_POINT ( 'NONE',  ( 32.30803788188344328, 7.816246126570704611, 1.949999999999824096 ) ) ;
#18926 = ORIENTED_EDGE ( 'NONE', *, *, #11089, .F. ) ;
#18927 = ORIENTED_EDGE ( 'NONE', *, *, #15994, .F. ) ;
#18928 = B_SPLINE_CURVE_WITH_KNOTS ( 'NONE', 3,
 ( #22687, #1266, #29786, #15371, #25195, #10934 ),
 .UNSPECIFIED., .F., .F.,
 ( 4, 2, 4 ),
 ( 0.000000000000000000, 0.0001000270069610021377, 0.0002000540139220042754 ),
 .UNSPECIFIED. ) ;
#18929 = EDGE_CURVE ( 'NONE', #13465, #21838, #24482, .T. ) ;
#18930 = CYLINDRICAL_SURFACE ( 'NONE', #23877, 1.000000000000000000 ) ;
#18931 = EDGE_CURVE ( 'NONE', #4965, #6063, #29112, .T. ) ;
#18932 = CARTESIAN_POINT ( 'NONE',  ( -62.09999999999997300, -2.647063127320109288, 0.1491152568578474336 ) ) ;
#18933 = DIRECTION ( 'NONE',  ( 1.000000000000000000, 0.000000000000000000, -1.047444401652940007E-14 ) ) ;
#18934 = B_SPLINE_CURVE_WITH_KNOTS ( 'NONE', 3,
 ( #1143, #17934, #30415, #29805, #10795, #25680 ),
 .UNSPECIFIED., .F., .F.,
 ( 4, 2, 4 ),
 ( 0.000000000000000000, 0.0001000270069610654009, 0.0002000540139221308018 ),
 .UNSPECIFIED. ) ;
#18935 = ORIENTED_EDGE ( 'NONE', *, *, #8165, .T. ) ;
#18936 = EDGE_CURVE ( 'NONE', #13707, #27904, #15452, .T. ) ;
#18937 = CARTESIAN_POINT ( 'NONE',  ( 57.02888841125436414, 0.7778303923484506388, 1.733491207451775207 ) ) ;
#18938 = CARTESIAN_POINT ( 'NONE',  ( 47.10000000000003695, 2.428612866367529932E-14, 4.199999999999827871 ) ) ;
#18939 = CARTESIAN_POINT ( 'NONE',  ( -56.76905989232412963, -2.944486372867094026, 1.699999999999778133 ) ) ;
#18940 = CARTESIAN_POINT ( 'NONE',  ( 58.74999981196285859, -1.050519579371408829, 1.649561145038723531 ) ) ;
#18941 = AXIS2_PLACEMENT_3D ( 'NONE', #25942, #25470, #21225 ) ;
#18942 = FACE_OUTER_BOUND ( 'NONE', #12920, .T. ) ;
#18943 = DIRECTION ( 'NONE',  ( 0.000000000000000000, -1.000000000000000000, -3.491481338843132566E-15 ) ) ;
#18944 = DIRECTION ( 'NONE',  ( 0.000000000000000000, 0.000000000000000000, 1.000000000000000000 ) ) ;
#18945 = AXIS2_PLACEMENT_3D ( 'NONE', #25641, #2911, #10185 ) ;
#18946 = EDGE_LOOP ( 'NONE', ( #30208, #30478, #31, #28576 ) ) ;
#18947 = CIRCLE ( 'NONE', #31062, 30.00000000000000355 ) ;
#18948 = CARTESIAN_POINT ( 'NONE',  ( 51.81783829102215577, 0.6462660169415540556, -4.286374879252671910 ) ) ;
#18949 = ORIENTED_EDGE ( 'NONE', *, *, #11356, .F. ) ;
#18950 = CARTESIAN_POINT ( 'NONE',  ( 52.09213388422778479, 8.599999999993011457, 2.049999999999818190 ) ) ;
#18951 = CARTESIAN_POINT ( 'NONE',  ( -54.61042740578360366, -2.936324665650200672, -2.606018187048499080 ) ) ;
#18953 = CARTESIAN_POINT ( 'NONE',  ( -36.63359589171323449, 3.777141534544248724, 3.869853550719733359 ) ) ;
#18952 = FACE_OUTER_BOUND ( 'NONE', #27102, .T. ) ;
#18954 = VERTEX_POINT ( 'NONE', #21684 ) ;
#18955 = ADVANCED_FACE ( 'NONE', ( #14528 ), #124, .F. ) ;
#18956 = B_SPLINE_CURVE_WITH_KNOTS ( 'NONE', 3,
 ( #13524, #4180, #1639, #23359, #30460, #28090, #1975, #18616, #28260, #8621 ),
 .UNSPECIFIED., .F., .F.,
 ( 4, 2, 2, 2, 4 ),
 ( 1.563658610346375379E-18, 0.0005941303177189510886, 0.001188260635437900659, 0.001782390953156850122, 0.002376521270875800017 ),
 .UNSPECIFIED. ) ;
#18957 = CARTESIAN_POINT ( 'NONE',  ( 50.40000000000001990, -0.6304760106459028624, 3.950000000000022826 ) ) ;
#18958 = ORIENTED_EDGE ( 'NONE', *, *, #23780, .T. ) ;
#18959 = DIRECTION ( 'NONE',  ( -3.489354422748178582E-15, 1.218509414717996338E-16, -1.000000000000000000 ) ) ;
#18960 = VERTEX_POINT ( 'NONE', #9934 ) ;
#18962 = CARTESIAN_POINT ( 'NONE',  ( 33.47623932017462778, 4.683225679163328437, 2.703237727951257607 ) ) ;
#18961 = CARTESIAN_POINT ( 'NONE',  ( -36.79682133506354091, 5.289443499204790733, 1.131445731060841453 ) ) ;
#18963 = EDGE_CURVE ( 'NONE', #27700, #26979, #2650, .T. ) ;
#18964 = ORIENTED_EDGE ( 'NONE', *, *, #22731, .T. ) ;
#18965 = CARTESIAN_POINT ( 'NONE',  ( 57.05000000000001137, -0.7500000000000001110, 1.778341924377885963 ) ) ;
#18966 = CARTESIAN_POINT ( 'NONE',  ( 58.64999999999999147, 1.782657835995388629, -0.5811678240976841936 ) ) ;
#18967 = CARTESIAN_POINT ( 'NONE',  ( -54.44999999999997442, -1.500000000000000222, -3.300094695611020867 ) ) ;
#18968 = DIRECTION ( 'NONE',  ( -1.000000000000000000, -0.000000000000000000, 0.000000000000000000 ) ) ;
#18969 = AXIS2_PLACEMENT_3D ( 'NONE', #25035, #29473, #12695 ) ;
#18970 = CARTESIAN_POINT ( 'NONE',  ( -59.25952994616205416, -4.643455692769875931E-15, 3.599999999999788702 ) ) ;
#18972 = EDGE_CURVE ( 'NONE', #15234, #25083, #12291, .T. ) ;
#18971 = CARTESIAN_POINT ( 'NONE',  ( -59.11085193857230280, -2.468077931648963386, -0.9654581933252147641 ) ) ;
#18973 = CARTESIAN_POINT ( 'NONE',  ( 58.65000000000001279, 0.5811678240972328879, 1.782657835995121287 ) ) ;
#18974 = CARTESIAN_POINT ( 'NONE',  ( -56.15835481156722153, -0.7533615035077977362, 3.673546848079179750 ) ) ;
#18975 = VECTOR ( 'NONE', #15103, 999.9999999999998863 ) ;
#18976 = CARTESIAN_POINT ( 'NONE',  ( -58.36042740578360366, -2.936324665650199783, -2.606018187048499524 ) ) ;
#18977 = CARTESIAN_POINT ( 'NONE',  ( 58.75000000000003553, -1.800471618824714071, 1.039502773796719959 ) ) ;
#18978 = AXIS2_PLACEMENT_3D ( 'NONE', #9094, #14620, #1965 ) ;
#18979 = ORIENTED_EDGE ( 'NONE', *, *, #19459, .F. ) ;
#18980 = CARTESIAN_POINT ( 'NONE',  ( 21.97322666366011035, 8.076925076899302169, -7.622595309165997977E-14 ) ) ;
#18981 = DIRECTION ( 'NONE',  ( -0.8262273428075540549, 0.5633368246415005887, 0.000000000000000000 ) ) ;
#18982 = DIRECTION ( 'NONE',  ( 0.000000000000000000, 0.000000000000000000, 1.000000000000000000 ) ) ;
#18983 = VERTEX_POINT ( 'NONE', #21835 ) ;
#18984 = CARTESIAN_POINT ( 'NONE',  ( -36.40878371307407235, -4.755985070912294610, 2.573747172434699859 ) ) ;
#18985 = EDGE_LOOP ( 'NONE', ( #25760, #7757, #21192, #26315 ) ) ;
#18986 = AXIS2_PLACEMENT_3D ( 'NONE', #13163, #15714, #25360 ) ;
#18987 = DIRECTION ( 'NONE',  ( 0.7542528389311764503, -0.5142632992712440343, 0.4082106245394847011 ) ) ;
#18989 = DIRECTION ( 'NONE',  ( 0.000000000000000000, 0.000000000000000000, 1.000000000000000000 ) ) ;
#18988 = DIRECTION ( 'NONE',  ( -1.000000000000000000, -1.018631342913014973E-14, -0.000000000000000000 ) ) ;
#18990 = ORIENTED_EDGE ( 'NONE', *, *, #10588, .T. ) ;
#18991 = EDGE_CURVE ( 'NONE', #7548, #4176, #23557, .T. ) ;
#18992 = ORIENTED_EDGE ( 'NONE', *, *, #27001, .F. ) ;
#18993 = DIRECTION ( 'NONE',  ( 1.000000000000000000, 1.047444401652940007E-14, -0.000000000000000000 ) ) ;
#18994 = ADVANCED_FACE ( 'NONE', ( #26863 ), #4701, .T. ) ;
#18995 = CARTESIAN_POINT ( 'NONE',  ( -60.54800159808252147, -0.7228413094357338808, 3.524724055549729229 ) ) ;
#18997 = CARTESIAN_POINT ( 'NONE',  ( 58.75000018595670070, 1.011330950599250711, 1.651828233789864875 ) ) ;
#18996 = CARTESIAN_POINT ( 'NONE',  ( 57.05000000000001847, 0.6999999999999999556, 0.000000000000000000 ) ) ;
#18998 = ADVANCED_FACE ( 'NONE', ( #5171 ), #21585, .F. ) ;
#18999 = ORIENTED_EDGE ( 'NONE', *, *, #3174, .T. ) ;
#19000 = CARTESIAN_POINT ( 'NONE',  ( -59.92292740578359656, -3.330682475591783653, -0.6830477631804103833 ) ) ;
#19001 = DIRECTION ( 'NONE',  ( 0.000000000000000000, 1.000000000000000000, 0.000000000000000000 ) ) ;
#19002 = DIRECTION ( 'NONE',  ( 1.000000000000000000, -0.000000000000000000, -1.047444401652940007E-14 ) ) ;
#19003 = CARTESIAN_POINT ( 'NONE',  ( -36.14504829323104929, 3.997758138077510015, 3.641634024966127203 ) ) ;
#19004 = AXIS2_PLACEMENT_3D ( 'NONE', #20959, #4484, #11612 ) ;
#19005 = CARTESIAN_POINT ( 'NONE',  ( 54.31409749668478071, 6.709390224138189751, -2.050000000000189004 ) ) ;
#19006 = PLANE ( 'NONE',  #18259 ) ;
#19007 = CARTESIAN_POINT ( 'NONE',  ( -62.06826830520247285, -2.668664083165746881, 0.1951513684571901941 ) ) ;
#19008 = EDGE_LOOP ( 'NONE', ( #23378, #11320, #16524, #4995 ) ) ;
#19009 = CIRCLE ( 'NONE', #7857, 0.2499999999999997780 ) ;
#19010 = EDGE_CURVE ( 'NONE', #24287, #27015, #15483, .T. ) ;
#19011 = PLANE ( 'NONE',  #3869 ) ;
#19012 = CARTESIAN_POINT ( 'NONE',  ( -36.58413561666603186, 3.261791109367091934, -4.314133646218116347 ) ) ;
#19013 = FACE_OUTER_BOUND ( 'NONE', #18184, .T. ) ;
#19014 = DIRECTION ( 'NONE',  ( 1.000000000000000000, 0.000000000000000000, -3.491481338843133750E-15 ) ) ;
#19015 = PLANE ( 'NONE',  #23614 ) ;
#19017 = CARTESIAN_POINT ( 'NONE',  ( -68.01382336603234080, -3.309142602788800391E-16, 2.205138456058669928E-15 ) ) ;
#19016 = CARTESIAN_POINT ( 'NONE',  ( -55.22085481156723574, -3.673546848079175753, -0.7533615035078071731 ) ) ;
#19018 = LINE ( 'NONE', #30729, #10937 ) ;
#19020 = DIRECTION ( 'NONE',  ( 1.047444401652940007E-14, 0.000000000000000000, 1.000000000000000000 ) ) ;
#19019 = DIRECTION ( 'NONE',  ( 1.000000000000000000, 1.047444401652940007E-14, 0.000000000000000000 ) ) ;
#19021 = EDGE_LOOP ( 'NONE', ( #16740, #25029, #18115, #19268 ) ) ;
#19022 = CARTESIAN_POINT ( 'NONE',  ( -35.85663232820584057, 4.804073783693418420, 2.042134687550397398 ) ) ;
#19023 = FACE_OUTER_BOUND ( 'NONE', #26493, .T. ) ;
#19025 = CARTESIAN_POINT ( 'NONE',  ( -36.89250464418361020, 5.037778396015492710, 1.970103387723980415 ) ) ;
#19024 = CARTESIAN_POINT ( 'NONE',  ( 15.03925126672122836, -2.199885893005920856, -4.939696249117695892 ) ) ;
#19026 = CARTESIAN_POINT ( 'NONE',  ( -59.29999999999997584, -0.7533615035078030653, 3.673546848079178417 ) ) ;
#19027 = AXIS2_PLACEMENT_3D ( 'NONE', #26862, #4860, #122 ) ;
#19028 = VERTEX_POINT ( 'NONE', #16907 ) ;
#19029 = ORIENTED_EDGE ( 'NONE', *, *, #4397, .F. ) ;
#19030 = DIRECTION ( 'NONE',  ( 1.000000000000000000, 1.293068473084537258E-16, 0.000000000000000000 ) ) ;
#19031 = EDGE_CURVE ( 'NONE', #3728, #25822, #1319, .T. ) ;
#19032 = ORIENTED_EDGE ( 'NONE', *, *, #20072, .T. ) ;
#19033 =( GEOMETRIC_REPRESENTATION_CONTEXT ( 3 ) GLOBAL_UNCERTAINTY_ASSIGNED_CONTEXT ( ( #619 ) ) GLOBAL_UNIT_ASSIGNED_CONTEXT ( ( #17870, #20872, #15486 ) ) REPRESENTATION_CONTEXT ( 'NONE', 'WORKASPACE' ) );
#19034 = CARTESIAN_POINT ( 'NONE',  ( 57.01079425239058196, -0.7499991164627679563, -1.746008812021272227 ) ) ;
#19035 = CARTESIAN_POINT ( 'NONE',  ( 57.05000000000001847, 0.7500000000000000000, -2.421260002560649660 ) ) ;
#19036 = EDGE_LOOP ( 'NONE', ( #16175, #26232, #19491, #20425 ) ) ;
#19037 = CARTESIAN_POINT ( 'NONE',  ( 58.72419296898063124, 1.874576113084453821, 0.04475215827456610618 ) ) ;
#19038 = ORIENTED_EDGE ( 'NONE', *, *, #2549, .T. ) ;
#19039 = PRESENTATION_STYLE_ASSIGNMENT (( #21580 ) ) ;
#19040 = CIRCLE ( 'NONE', #5360, 2.000000000000000000 ) ;
#19041 = CARTESIAN_POINT ( 'NONE',  ( 51.41795137217811629, -3.967700393345039878, -1.365904513877001403 ) ) ;
#19042 = ORIENTED_EDGE ( 'NONE', *, *, #25179, .F. ) ;
#19043 = EDGE_LOOP ( 'NONE', ( #5337, #12238, #1433, #14375, #6051, #22382 ) ) ;
#19044 = CIRCLE ( 'NONE', #13944, 2.625000000001612044 ) ;
#19045 = ORIENTED_EDGE ( 'NONE', *, *, #23836, .T. ) ;
#19047 = ADVANCED_FACE ( 'NONE', ( #24340 ), #9437, .T. ) ;
#19046 = B_SPLINE_CURVE_WITH_KNOTS ( 'NONE', 3,
 ( #3952, #8689, #3640, #13428, #13275, #9019, #25477, #22824, #30387, #1419, #8544, #23130, #6323 ),
 .UNSPECIFIED., .F., .F.,
 ( 4, 3, 3, 3, 4 ),
 ( 0.000000000000000000, 3.627661428711262821E-05, 7.228648945962581657E-05, 0.0001163236820996669683, 0.0001184416086866318864 ),
 .UNSPECIFIED. ) ;
#19048 = CARTESIAN_POINT ( 'NONE',  ( -61.06249999999995737, 3.925981830489463142, -2.023818954174166834E-13 ) ) ;
#19049 = AXIS2_PLACEMENT_3D ( 'NONE', #12263, #21948, #19575 ) ;
#19050 = CARTESIAN_POINT ( 'NONE',  ( -57.62499999999997158, 2.489203624310596830, -2.804704140674912249 ) ) ;
#19051 = CARTESIAN_POINT ( 'NONE',  ( 58.75000000000002132, 6.153735859711025284E-13, 3.111507638930570854E-58 ) ) ;
#19052 = CIRCLE ( 'NONE', #13443, 4.200000000000016165 ) ;
#19053 = CARTESIAN_POINT ( 'NONE',  ( -61.38137739671039128, -2.585543411474696462, -0.7802324315830138080 ) ) ;
#19054 = AXIS2_PLACEMENT_3D ( 'NONE', #17356, #27003, #14974 ) ;
#19055 = VECTOR ( 'NONE', #11238, 1000.000000000000000 ) ;
#19056 = AXIS2_PLACEMENT_3D ( 'NONE', #30325, #1509, #3886 ) ;
#19058 = DIRECTION ( 'NONE',  ( 1.000000000000000000, -0.000000000000000000, -0.000000000000000000 ) ) ;
#19057 =( NAMED_UNIT ( * ) PLANE_ANGLE_UNIT ( ) SI_UNIT ( $, .RADIAN. ) );
#19059 = DIRECTION ( 'NONE',  ( 1.163827112947767259E-15, 0.9428090415820590264, -0.3333333333333461379 ) ) ;
#19060 = CARTESIAN_POINT ( 'NONE',  ( 48.30000000000001847, 0.6462379109121000331, 4.048750000000023164 ) ) ;
#19061 = CARTESIAN_POINT ( 'NONE',  ( 15.68751737981905592, 5.244794032782712279, -1.329291831544122005 ) ) ;
#19062 = ORIENTED_EDGE ( 'NONE', *, *, #15289, .T. ) ;
#19063 = CARTESIAN_POINT ( 'NONE',  ( 52.08333333333334991, 4.368973594129894167, -1.439468559502902645 ) ) ;
#19064 = CARTESIAN_POINT ( 'NONE',  ( 54.19028661868582475, 6.697846887293304796, 2.049999999999810640 ) ) ;
#19065 = ORIENTED_EDGE ( 'NONE', *, *, #350, .F. ) ;
#19066 = LINE ( 'NONE', #26009, #16655 ) ;
#19067 = CARTESIAN_POINT ( 'NONE',  ( -58.84599364905385954, 0.2309624077928955632, 3.875409454552791289 ) ) ;
#19068 = CARTESIAN_POINT ( 'NONE',  ( 47.05963571244991783, 8.266527678078146479, 1.549999999999835953 ) ) ;
#19069 = CIRCLE ( 'NONE', #4384, 3.625000000000028866 ) ;
#19070 = ADVANCED_FACE ( 'NONE', ( #267 ), #4559, .T. ) ;
#19071 = CIRCLE ( 'NONE', #27641, 2.000000000000000000 ) ;
#19072 = EDGE_LOOP ( 'NONE', ( #9680, #22673, #16816, #28495 ) ) ;
#19073 = CARTESIAN_POINT ( 'NONE',  ( 47.73537254841801314, -4.023728077055556795, 1.198744011644558682 ) ) ;
#19074 = CARTESIAN_POINT ( 'NONE',  ( 24.57460841532291340, 5.893272594507614315, 1.424999999999914335 ) ) ;
#19075 = CARTESIAN_POINT ( 'NONE',  ( -54.82202994616206126, 2.078460969082646770, 3.599999999999812683 ) ) ;
#19076 = ORIENTED_EDGE ( 'NONE', *, *, #17181, .T. ) ;
#19077 = VECTOR ( 'NONE', #23805, 1000.000000000000000 ) ;
#19078 = ORIENTED_EDGE ( 'NONE', *, *, #182, .T. ) ;
#19079 = CARTESIAN_POINT ( 'NONE',  ( 15.03925126672122303, 4.683225679163316890, 2.703237727951268710 ) ) ;
#19080 = ORIENTED_EDGE ( 'NONE', *, *, #10614, .F. ) ;
#19081 = VECTOR ( 'NONE', #27043, 1000.000000000000000 ) ;
#19082 = LINE ( 'NONE', #14622, #30838 ) ;
#19083 = CARTESIAN_POINT ( 'NONE',  ( -57.82202994616206126, 2.078460969082646770, 3.599999999999802025 ) ) ;
#19084 = EDGE_LOOP ( 'NONE', ( #25252, #14156, #4650, #14772 ) ) ;
#19085 = CARTESIAN_POINT ( 'NONE',  ( 50.80000000000002558, -4.031600731908413948, 1.173113608511496375 ) ) ;
#19086 = CIRCLE ( 'NONE', #5917, 5.407411300779133789 ) ;
#19087 = VECTOR ( 'NONE', #7060, 1000.000000000000000 ) ;
#19088 = DIRECTION ( 'NONE',  ( 0.000000000000000000, 0.9996898646859344595, 0.02490330187381124133 ) ) ;
#19089 = DIRECTION ( 'NONE',  ( 0.000000000000000000, -1.000000000000000000, 0.000000000000000000 ) ) ;
#19090 = ORIENTED_EDGE ( 'NONE', *, *, #27756, .T. ) ;
#19091 = EDGE_CURVE ( 'NONE', #24584, #29689, #16615, .T. ) ;
#19092 = CARTESIAN_POINT ( 'NONE',  ( -35.85663232820583346, -3.817150320980684075, 2.203324261490539282 ) ) ;
#19093 = CARTESIAN_POINT ( 'NONE',  ( -54.39999999999996305, -1.399999999999979261, -3.959797974644882146 ) ) ;
#19094 = CARTESIAN_POINT ( 'NONE',  ( 15.03925126672132961, -3.426725943139530717, -3.937891353488757851 ) ) ;
#19095 = ORIENTED_EDGE ( 'NONE', *, *, #28459, .T. ) ;
#19096 = CIRCLE ( 'NONE', #5925, 0.04999999999999989175 ) ;
#19097 = CARTESIAN_POINT ( 'NONE',  ( 51.23644008536124517, -1.080112125195908046, 1.214076932077873039 ) ) ;
#19098 = CARTESIAN_POINT ( 'NONE',  ( -59.30000000000042348, -2.541725022351402963, -2.757196748647571027 ) ) ;
#19099 = CIRCLE ( 'NONE', #9486, 0.2000000000000000944 ) ;
#19100 = CIRCLE ( 'NONE', #17065, 0.2500000000000002776 ) ;
#19101 = DIRECTION ( 'NONE',  ( 0.000000000000000000, 0.000000000000000000, 1.000000000000000000 ) ) ;
#19103 = DIRECTION ( 'NONE',  ( 0.000000000000000000, 1.000000000000000000, 0.000000000000000000 ) ) ;
#19102 = CARTESIAN_POINT ( 'NONE',  ( 58.75000006180463430, -0.5511536957112744828, -1.849318015437667828 ) ) ;
#19104 = ADVANCED_FACE ( 'NONE', ( #3587 ), #29639, .T. ) ;
#19105 = DIRECTION ( 'NONE',  ( 1.000000000000000000, 1.047444401652940007E-14, 0.000000000000000000 ) ) ;
#19106 = CARTESIAN_POINT ( 'NONE',  ( 58.65000000000003411, -1.671477153793470949, 0.8495817349404535257 ) ) ;
#19107 = VECTOR ( 'NONE', #21852, 1000.000000000000000 ) ;
#19108 = CARTESIAN_POINT ( 'NONE',  ( -54.44999999999997442, 0.000000000000000000, 0.000000000000000000 ) ) ;
#19109 = AXIS2_PLACEMENT_3D ( 'NONE', #8555, #15538, #805 ) ;
#19110 = AXIS2_PLACEMENT_3D ( 'NONE', #14891, #24553, #5097 ) ;
#19111 = ORIENTED_EDGE ( 'NONE', *, *, #3445, .F. ) ;
#19112 = VERTEX_POINT ( 'NONE', #27650 ) ;
#19113 = EDGE_CURVE ( 'NONE', #27607, #3125, #7896, .T. ) ;
#19114 = CARTESIAN_POINT ( 'NONE',  ( -59.12687546363279267, -2.340603034507739100, 1.249089021148755752 ) ) ;
#19115 = EDGE_LOOP ( 'NONE', ( #11366, #19450, #5626, #24082 ) ) ;
#19116 = EDGE_CURVE ( 'NONE', #27954, #21791, #31165, .T. ) ;
#19117 = CARTESIAN_POINT ( 'NONE',  ( -54.39999999999997726, 8.366749974758389781E-15, -1.935485844574984262E-13 ) ) ;
#19118 = CARTESIAN_POINT ( 'NONE',  ( -56.61042740578360366, 3.725040285533371076, -1.239922660687675871 ) ) ;
#19120 = CARTESIAN_POINT ( 'NONE',  ( 51.41858953131476540, -3.967542327744261410, -1.366354831956597460 ) ) ;
#19119 = CARTESIAN_POINT ( 'NONE',  ( 48.50000000000002132, 1.391941090707534023, 3.750000000000022649 ) ) ;
#19121 = EDGE_CURVE ( 'NONE', #21850, #28904, #19044, .T. ) ;
#19122 = ORIENTED_EDGE ( 'NONE', *, *, #19942, .T. ) ;
#19123 = ORIENTED_EDGE ( 'NONE', *, *, #16643, .F. ) ;
#19124 = CYLINDRICAL_SURFACE ( 'NONE', #14882, 0.7500000000000001110 ) ;
#19125 = CIRCLE ( 'NONE', #31239, 0.1500000000000000777 ) ;
#19126 = ORIENTED_EDGE ( 'NONE', *, *, #24118, .T. ) ;
#19127 = LINE ( 'NONE', #7080, #27694 ) ;
#19128 = CIRCLE ( 'NONE', #24655, 0.1000000000000000611 ) ;
#19129 = VERTEX_POINT ( 'NONE', #8491 ) ;
#19131 = DIRECTION ( 'NONE',  ( 3.002035892788116966E-16, -0.9996898646859343485, -0.02490330187381123786 ) ) ;
#19130 = CARTESIAN_POINT ( 'NONE',  ( -36.92405921417682890, 5.187083072802322725, 1.534568794951225001 ) ) ;
#19132 = VERTEX_POINT ( 'NONE', #22435 ) ;
#19133 = FACE_OUTER_BOUND ( 'NONE', #14741, .T. ) ;
#19134 = DIRECTION ( 'NONE',  ( 0.000000000000000000, -0.2008964009354147484, 0.9796124928211139560 ) ) ;
#19135 = CIRCLE ( 'NONE', #30221, 0.2500000000000000000 ) ;
#19136 = CARTESIAN_POINT ( 'NONE',  ( 47.10000000000002984, -4.020776289669855785, 2.234582293948414122 ) ) ;
#19137 = ADVANCED_FACE ( 'NONE', ( #20387 ), #1197, .F. ) ;
#19138 = CARTESIAN_POINT ( 'NONE',  ( -59.19999999999997442, 8.366749974758448157E-15, -2.103076948839454410E-13 ) ) ;
#19139 = CARTESIAN_POINT ( 'NONE',  ( -56.38452994616205416, 3.117691453623979481, 1.799999999999811751 ) ) ;
#19140 = CARTESIAN_POINT ( 'NONE',  ( -59.10126175476050037, -2.465973215592141887, -0.9703132807041499053 ) ) ;
#19141 = B_SPLINE_CURVE_WITH_KNOTS ( 'NONE', 3,
 ( #19956, #27232, #5544, #12804 ),
 .UNSPECIFIED., .F., .F.,
 ( 4, 4 ),
 ( 2.168404344971008627E-19, 0.0001476506082772709844 ),
 .UNSPECIFIED. ) ;
#19142 = CARTESIAN_POINT ( 'NONE',  ( 47.00000000000002132, 6.982261990806648555E-14, -1.628983268085978048E-13 ) ) ;
#19143 = CARTESIAN_POINT ( 'NONE',  ( 58.75000000000001421, 0.6373668173475968146, -1.895722432252298084 ) ) ;
#19144 = EDGE_CURVE ( 'NONE', #3817, #13707, #5362, .T. ) ;
#19145 = AXIS2_PLACEMENT_3D ( 'NONE', #6452, #27670, #25291 ) ;
#19146 = CYLINDRICAL_SURFACE ( 'NONE', #26581, 0.1000000000000000472 ) ;
#19147 = ORIENTED_EDGE ( 'NONE', *, *, #30200, .F. ) ;
#19149 = ADVANCED_FACE ( 'NONE', ( #29865 ), #26364, .T. ) ;
#19148 = CARTESIAN_POINT ( 'NONE',  ( 51.80000000000001847, 1.734723475976807094E-15, 0.000000000000000000 ) ) ;
#19150 = VERTEX_POINT ( 'NONE', #24801 ) ;
#19151 = DIRECTION ( 'NONE',  ( 1.000000000000000000, 1.047444401652940007E-14, 0.000000000000000000 ) ) ;
#19152 = LINE ( 'NONE', #6303, #24718 ) ;
#19153 = CARTESIAN_POINT ( 'NONE',  ( 53.81464057712624793, 5.799094425976102585, -1.689602626210267466 ) ) ;
#19154 = ORIENTED_EDGE ( 'NONE', *, *, #5046, .T. ) ;
#19155 = CARTESIAN_POINT ( 'NONE',  ( -59.68727869885009341, -3.216413352772560685, -1.231193962818940113 ) ) ;
#19156 = ORIENTED_EDGE ( 'NONE', *, *, #5485, .T. ) ;
#19157 = EDGE_CURVE ( 'NONE', #26099, #19552, #27111, .T. ) ;
#19158 = CARTESIAN_POINT ( 'NONE',  ( 15.17214319754860696, 0.4576450703117014296, -5.200000005133889047 ) ) ;
#19160 = DIRECTION ( 'NONE',  ( -0.000000000000000000, 1.000000000000000000, 1.532429380227459806E-15 ) ) ;
#19159 = CARTESIAN_POINT ( 'NONE',  ( 58.65263613458535019, 0.8791532451977436269, -1.656197658588938193 ) ) ;
#19161 = EDGE_CURVE ( 'NONE', #10675, #6667, #16461, .T. ) ;
#19162 = ORIENTED_EDGE ( 'NONE', *, *, #4583, .F. ) ;
#19163 = ORIENTED_EDGE ( 'NONE', *, *, #14012, .T. ) ;
#19164 = DIRECTION ( 'NONE',  ( 0.000000000000000000, 1.000000000000000000, 0.000000000000000000 ) ) ;
#19165 = CARTESIAN_POINT ( 'NONE',  ( -54.44999999999997442, 1.499999999999999556, 3.300094695611021756 ) ) ;
#19167 = CARTESIAN_POINT ( 'NONE',  ( 58.75000000000000711, 0.8948927608033926395, 1.760622601997029690 ) ) ;
#19166 = CARTESIAN_POINT ( 'NONE',  ( 58.66054497608116947, -0.4999999999856035160, 1.807104036853935503 ) ) ;
#19168 = ORIENTED_EDGE ( 'NONE', *, *, #2688, .F. ) ;
#19169 = CARTESIAN_POINT ( 'NONE',  ( -56.06249999999997868, 4.108500314926511798, -1.367561758111407677 ) ) ;
#19170 = CARTESIAN_POINT ( 'NONE',  ( 61.24141714606658127, 0.9075239022126483368, 1.727282253938982270 ) ) ;
#19171 = FACE_OUTER_BOUND ( 'NONE', #14453, .T. ) ;
#19172 = CIRCLE ( 'NONE', #31280, 4.849999999999999645 ) ;
#19173 = CARTESIAN_POINT ( 'NONE',  ( -44.49999999999997868, 0.000000000000000000, 2.168404344971008868E-14 ) ) ;
#19174 = CARTESIAN_POINT ( 'NONE',  ( -61.35552595367609996, -2.605636331997853716, -0.5976426842213763413 ) ) ;
#19175 =( BOUNDED_SURFACE ( )  B_SPLINE_SURFACE ( 3, 2, ( 
 ( #19694, #12235, #26182 ),
 ( #56, #14294, #5109 ),
 ( #9719, #21919, #4788 ),
 ( #9573, #14610, #11922 ),
 ( #16693, #7330, #2104 ),
 ( #2431, #16525, #14446 ),
 ( #19231, #7496, #17001 ),
 ( #19535, #2257, #21443 ),
 ( #12091, #23963, #21769 ),
 ( #28872, #24420, #31249 ) ),
 .UNSPECIFIED., .F., .F., .F. ) 
 B_SPLINE_SURFACE_WITH_KNOTS ( ( 4, 2, 2, 2, 4 ),
 ( 3, 3 ),
 ( 0.0002526260074104870901, 0.0003606909493797115550, 0.0004687558913489359657, 0.0006848857752873848412, 0.001117145543164282592 ),
 ( 0.000000000000000000, 1.000000000000000000 ),
 .UNSPECIFIED. ) 
 GEOMETRIC_REPRESENTATION_ITEM ( )  RATIONAL_B_SPLINE_SURFACE ( (
 ( 1.000000000000000000, 0.9842509842511785179, 1.000000000000000000),
 ( 1.000000000000000000, 0.9838268088398656186, 1.000000000000000000),
 ( 1.000000000000000000, 0.9731519947952637084, 1.000000000000000000),
 ( 1.000000000000000000, 0.9499473078865111608, 1.000000000000000000),
 ( 1.000000000000000000, 0.9371632344323036490, 1.000000000000000000),
 ( 1.000000000000000000, 0.8981767195496310752, 1.000000000000000000),
 ( 1.000000000000000000, 0.8714317066438556081, 1.000000000000000000),
 ( 1.000000000000000000, 0.7945716934681391619, 1.000000000000000000),
 ( 1.000000000000000000, 0.7462340517456872435, 1.000000000000000000),
 ( 1.000000000000000000, 0.7071067811865260344, 1.000000000000000000) ) ) 
 REPRESENTATION_ITEM ( '' )  SURFACE ( )  );
#19176 = DIRECTION ( 'NONE',  ( 3.002035892788116966E-16, -0.9996898646859343485, -0.02490330187381123786 ) ) ;
#19177 = DIRECTION ( 'NONE',  ( 0.000000000000000000, 0.7438053426813423519, 0.6683962987619627150 ) ) ;
#19178 = ORIENTED_EDGE ( 'NONE', *, *, #28214, .T. ) ;
#19179 = CARTESIAN_POINT ( 'NONE',  ( 57.01256279823148532, -0.7331429619035759737, 1.793127402884417965 ) ) ;
#19180 = CARTESIAN_POINT ( 'NONE',  ( 16.10705563471231017, -3.051830235922889489, 4.466755975380364063 ) ) ;
#19181 = CARTESIAN_POINT ( 'NONE',  ( 52.05000000000001137, 4.616741406585203933, -2.050000000000181011 ) ) ;
#19182 = CARTESIAN_POINT ( 'NONE',  ( 26.81612439946666626, 5.236792088878508444, -1.950000000000093880 ) ) ;
#19183 = EDGE_CURVE ( 'NONE', #4826, #26557, #19261, .T. ) ;
#19184 = EDGE_CURVE ( 'NONE', #16699, #24542, #5646, .T. ) ;
#19185 = CARTESIAN_POINT ( 'NONE',  ( 57.00500393873097238, -0.7225500701544015358, -2.438740121660158078 ) ) ;
#19188 = EDGE_CURVE ( 'NONE', #22535, #4925, #6590, .T. ) ;
#19187 = CARTESIAN_POINT ( 'NONE',  ( -35.85663232820584057, 1.793057972834756431, 4.026191436120398315 ) ) ;
#19186 = FACE_OUTER_BOUND ( 'NONE', #24726, .T. ) ;
#19189 = CARTESIAN_POINT ( 'NONE',  ( 47.12385499560041779, -4.149773407328906316, -1.728861777176172509 ) ) ;
#19191 = CARTESIAN_POINT ( 'NONE',  ( -54.49999999999997868, 3.400000000000007905, -1.910919895035100347E-13 ) ) ;
#19190 = CARTESIAN_POINT ( 'NONE',  ( 50.80000000000002558, -3.908336260473453727, 1.238913909465742202 ) ) ;
#19192 = VERTEX_POINT ( 'NONE', #6269 ) ;
#19193 = AXIS2_PLACEMENT_3D ( 'NONE', #1778, #8455, #25391 ) ;
#19194 = CARTESIAN_POINT ( 'NONE',  ( 58.66107449606997903, 0.9668599424584182200, -1.606832818401373375 ) ) ;
#19195 = DIRECTION ( 'NONE',  ( 0.03489949670250097613, 0.9993908270190957621, 2.465190328815662439E-32 ) ) ;
#19197 = CARTESIAN_POINT ( 'NONE',  ( -36.27260443516981780, 5.005099703116275833, 1.423440526322142574 ) ) ;
#19196 = DIRECTION ( 'NONE',  ( 0.000000000000000000, 0.000000000000000000, 1.000000000000000000 ) ) ;
#19198 = CARTESIAN_POINT ( 'NONE',  ( 15.41586008885037806, -4.863061488092547791, 1.860589201779584867 ) ) ;
#19199 = VERTEX_POINT ( 'NONE', #2426 ) ;
#19200 = ORIENTED_EDGE ( 'NONE', *, *, #25069, .T. ) ;
#19201 = DIRECTION ( 'NONE',  ( -1.000000000000000000, -0.000000000000000000, -0.000000000000000000 ) ) ;
#19202 = ORIENTED_EDGE ( 'NONE', *, *, #17877, .F. ) ;
#19203 = FACE_OUTER_BOUND ( 'NONE', #6853, .T. ) ;
#19204 = CARTESIAN_POINT ( 'NONE',  ( -71.49999999999998579, -0.3062499654112579295, 1.493338310920507839 ) ) ;
#19205 = CIRCLE ( 'NONE', #8060, 0.09999999999999992228 ) ;
#19206 = ORIENTED_EDGE ( 'NONE', *, *, #15827, .T. ) ;
#19207 = CARTESIAN_POINT ( 'NONE',  ( 48.30000000000001847, 2.428612866367529932E-14, 0.000000000000000000 ) ) ;
#19208 = EDGE_LOOP ( 'NONE', ( #17203, #9622, #3243, #4832 ) ) ;
#19209 = CARTESIAN_POINT ( 'NONE',  ( 50.80000000000001847, -4.031600731908413948, -1.173113608511851869 ) ) ;
#19210 = AXIS2_PLACEMENT_3D ( 'NONE', #10451, #15819, #23123 ) ;
#19211 = ORIENTED_EDGE ( 'NONE', *, *, #18887, .F. ) ;
#19212 = EDGE_LOOP ( 'NONE', ( #22293, #1458, #18401, #25552 ) ) ;
#19213 = AXIS2_PLACEMENT_3D ( 'NONE', #3660, #13295, #27736 ) ;
#19214 = CARTESIAN_POINT ( 'NONE',  ( -54.38452994616203995, 2.093608279459366986E-14, -3.600000000000193268 ) ) ;
#19215 = LINE ( 'NONE', #12669, #11531 ) ;
#19216 = DIRECTION ( 'NONE',  ( 3.023770467182126270E-15, -0.4999707644721522182, 0.8660422822663637055 ) ) ;
#19217 = DIRECTION ( 'NONE',  ( 0.000000000000000000, -3.469446951953611033E-15, 1.000000000000000000 ) ) ;
#19218 = LINE ( 'NONE', #30917, #2413 ) ;
#19219 = AXIS2_PLACEMENT_3D ( 'NONE', #11293, #23496, #6406 ) ;
#19220 = ADVANCED_FACE ( 'NONE', ( #27952 ), #13439, .T. ) ;
#19222 = LINE ( 'NONE', #8899, #14921 ) ;
#19221 = DIRECTION ( 'NONE',  ( 3.304235192336781034E-15, 0.000000000000000000, 1.000000000000000000 ) ) ;
#19223 = DIRECTION ( 'NONE',  ( -1.000000000000000000, -0.000000000000000000, 3.491481338843133355E-15 ) ) ;
#19224 = DIRECTION ( 'NONE',  ( 0.000000000000000000, 0.000000000000000000, -1.000000000000000000 ) ) ;
#19226 = FACE_OUTER_BOUND ( 'NONE', #9204, .T. ) ;
#19225 = CARTESIAN_POINT ( 'NONE',  ( 15.03925126672127632, 5.086913985776164715, -1.171642053949048856 ) ) ;
#19227 = ORIENTED_EDGE ( 'NONE', *, *, #16750, .T. ) ;
#19228 = CARTESIAN_POINT ( 'NONE',  ( 15.03925126672133139, -4.804073783693434407, -2.042134687550376526 ) ) ;
#19229 =( BOUNDED_SURFACE ( )  B_SPLINE_SURFACE ( 3, 2, ( 
 ( #1931, #21419, #21110 ),
 ( #30904, #30749, #11592 ),
 ( #9055, #21274, #9219 ),
 ( #2081, #26151, #18726 ),
 ( #28522, #25831, #11744 ),
 ( #6829, #31221, #14111 ),
 ( #13775, #19037, #16669 ),
 ( #9547, #28845, #7158 ),
 ( #8876, #28371, #18567 ),
 ( #23312, #23937, #16337 ) ),
 .UNSPECIFIED., .F., .F., .F. ) 
 B_SPLINE_SURFACE_WITH_KNOTS ( ( 4, 2, 2, 2, 4 ),
 ( 3, 3 ),
 ( 0.0001706658715691949555, 0.0002229276920778155090, 0.0002751895125864360354, 0.0003274513330950565618, 0.0003797131536036770882 ),
 ( 0.000000000000000000, 1.000000000000000000 ),
 .UNSPECIFIED. ) 
 GEOMETRIC_REPRESENTATION_ITEM ( )  RATIONAL_B_SPLINE_SURFACE ( (
 ( 1.000000000000000000, 0.7071067811865214825, 1.000000000000000000),
 ( 1.000000000000000000, 0.7375607040702809591, 1.000000000000000000),
 ( 1.000000000000000000, 0.7730431127428194493, 1.000000000000000000),
 ( 1.000000000000000000, 0.8321012486990639889, 1.000000000000000000),
 ( 1.000000000000000000, 0.8541932017412365852, 1.000000000000000000),
 ( 1.000000000000000000, 0.8545723906067121955, 1.000000000000000000),
 ( 1.000000000000000000, 0.8327032135054380779, 1.000000000000000000),
 ( 1.000000000000000000, 0.7734559727063156087, 1.000000000000000000),
 ( 1.000000000000000000, 0.7377766653997859247, 1.000000000000000000),
 ( 1.000000000000000000, 0.7071067811865229258, 1.000000000000000000) ) ) 
 REPRESENTATION_ITEM ( '' )  SURFACE ( )  );
#19230 = CARTESIAN_POINT ( 'NONE',  ( -54.39999999999996305, -1.599999999999981215, -3.363870538531692045 ) ) ;
#19232 = CARTESIAN_POINT ( 'NONE',  ( 48.49162684147595570, -1.391941090707504269, -3.850000000000020517 ) ) ;
#19231 = CARTESIAN_POINT ( 'NONE',  ( 48.41509867277373047, -1.114141714781589521, 3.896173399896524003 ) ) ;
#19233 = CARTESIAN_POINT ( 'NONE',  ( 58.64999999999992042, -1.469015551795658681, -1.320082690054208419 ) ) ;
#19234 = CYLINDRICAL_SURFACE ( 'NONE', #31134, 3.500000000000000444 ) ;
#19235 = AXIS2_PLACEMENT_3D ( 'NONE', #11369, #11848, #28799 ) ;
#19236 = ADVANCED_FACE ( 'NONE', ( #6434 ), #25598, .F. ) ;
#19237 = CIRCLE ( 'NONE', #7580, 0.05000000000000012768 ) ;
#19238 = VERTEX_POINT ( 'NONE', #11315 ) ;
#19239 = CARTESIAN_POINT ( 'NONE',  ( 60.87284881435257944, 0.5000000998574327671, -1.554802432719798011 ) ) ;
#19240 = CARTESIAN_POINT ( 'NONE',  ( -61.18749999999995737, 1.962990915244749557, -3.400000000000207745 ) ) ;
#19241 = ORIENTED_EDGE ( 'NONE', *, *, #14452, .F. ) ;
#19242 = VERTEX_POINT ( 'NONE', #23225 ) ;
#19243 = CARTESIAN_POINT ( 'NONE',  ( -59.52606392228539534, 3.344530751152334780, -1.138116568171968046 ) ) ;
#19244 = VERTEX_POINT ( 'NONE', #6122 ) ;
#19245 = CIRCLE ( 'NONE', #8586, 0.04999999999999991257 ) ;
#19246 = CARTESIAN_POINT ( 'NONE',  ( 48.40116939571130672, -0.8930800907915671383, 3.925677024646228475 ) ) ;
#19247 = CARTESIAN_POINT ( 'NONE',  ( -58.57202994616204705, 2.078460969082646770, 3.599999999999799805 ) ) ;
#19248 = ORIENTED_EDGE ( 'NONE', *, *, #12393, .F. ) ;
#19249 = CARTESIAN_POINT ( 'NONE',  ( 58.65000000000001990, 6.143261415694495821E-13, 3.111507638930570854E-58 ) ) ;
#19250 = FACE_OUTER_BOUND ( 'NONE', #6522, .T. ) ;
#19251 = CARTESIAN_POINT ( 'NONE',  ( 31.73163254175109671, 7.673342709000030126, 2.049999999999888800 ) ) ;
#19252 = ORIENTED_EDGE ( 'NONE', *, *, #26030, .T. ) ;
#19253 = CIRCLE ( 'NONE', #26305, 0.05000000000000009298 ) ;
#19254 = CARTESIAN_POINT ( 'NONE',  ( -54.39999999999999147, -1.400000000000004574, 3.363870538531238630 ) ) ;
#19255 = CARTESIAN_POINT ( 'NONE',  ( -73.89999999999997726, -2.435524336289708093E-15, 4.607889071584891164E-15 ) ) ;
#19256 = CARTESIAN_POINT ( 'NONE',  ( 58.74154451056421067, -0.8556855217782239897, -1.668374833163418947 ) ) ;
#19257 = ORIENTED_EDGE ( 'NONE', *, *, #18830, .F. ) ;
#19258 = DIRECTION ( 'NONE',  ( 0.000000000000000000, 0.000000000000000000, -1.000000000000000000 ) ) ;
#19259 = DIRECTION ( 'NONE',  ( -1.499696682456171775E-15, 0.9030524935654854479, 0.4295302013423024645 ) ) ;
#19260 = ADVANCED_FACE ( 'NONE', ( #30637 ), #1514, .T. ) ;
#19261 = B_SPLINE_CURVE_WITH_KNOTS ( 'NONE', 3,
 ( #30475, #4052, #28278, #20847 ),
 .UNSPECIFIED., .F., .F.,
 ( 4, 4 ),
 ( 0.000000000000000000, 0.0002184312136277828859 ),
 .UNSPECIFIED. ) ;
#19263 = CARTESIAN_POINT ( 'NONE',  ( 58.65000038048066955, -0.8644232797868882656, 1.663933463835922666 ) ) ;
#19262 = CARTESIAN_POINT ( 'NONE',  ( -36.42771574642715393, -2.777216423307978133, 4.646230875016813755 ) ) ;
#19264 = ADVANCED_FACE ( 'NONE', ( #24115 ), #2351, .T. ) ;
#19265 = AXIS2_PLACEMENT_3D ( 'NONE', #12894, #10075, #29381 ) ;
#19266 = FACE_BOUND ( 'NONE', #27527, .T. ) ;
#19267 = CARTESIAN_POINT ( 'NONE',  ( 53.94440344817330413, 6.524635634306426901, 2.049999999999811529 ) ) ;
#19268 = ORIENTED_EDGE ( 'NONE', *, *, #22283, .F. ) ;
#19269 = ORIENTED_EDGE ( 'NONE', *, *, #10358, .F. ) ;
#19270 = EDGE_CURVE ( 'NONE', #15970, #15422, #6389, .T. ) ;
#19271 = CARTESIAN_POINT ( 'NONE',  ( 58.66595318830225381, 0.5000000000006145084, -1.807217177072659275 ) ) ;
#19272 = ORIENTED_EDGE ( 'NONE', *, *, #18081, .F. ) ;
#19273 = PLANE ( 'NONE',  #25847 ) ;
#19274 = CARTESIAN_POINT ( 'NONE',  ( -59.72085481156722864, -3.673546848079176197, -0.7533615035078060629 ) ) ;
#19276 = CARTESIAN_POINT ( 'NONE',  ( 68.00000000000001421, 1.401298464324817071E-42, -7.122621931239992550E-13 ) ) ;
#19275 = LINE ( 'NONE', #2306, #10463 ) ;
#19277 = VERTEX_POINT ( 'NONE', #4197 ) ;
#19278 = ORIENTED_EDGE ( 'NONE', *, *, #9830, .T. ) ;
#19279 = DIRECTION ( 'NONE',  ( 0.000000000000000000, 0.000000000000000000, 1.000000000000000000 ) ) ;
#19280 = EDGE_LOOP ( 'NONE', ( #30241, #19996, #12666, #24090 ) ) ;
#19281 = CARTESIAN_POINT ( 'NONE',  ( 29.25706191173316739, 5.994885333997869381, 1.949999999999897371 ) ) ;
#19282 = ORIENTED_EDGE ( 'NONE', *, *, #17320, .T. ) ;
#19283 = CARTESIAN_POINT ( 'NONE',  ( 50.40000000000001279, 0.7707709757764751313, 3.938803467580343831 ) ) ;
#19284 = VERTEX_POINT ( 'NONE', #21178 ) ;
#19285 = DIRECTION ( 'NONE',  ( 0.000000000000000000, 0.2008964009354147484, -0.9796124928211140670 ) ) ;
#19286 = EDGE_CURVE ( 'NONE', #29981, #6604, #11500, .T. ) ;
#19287 = CARTESIAN_POINT ( 'NONE',  ( 57.01635142493560693, 0.7373792903891465134, 1.789496335369930025 ) ) ;
#19288 = AXIS2_PLACEMENT_3D ( 'NONE', #17469, #24894, #528 ) ;
#19289 = CARTESIAN_POINT ( 'NONE',  ( -59.57529047491064489, 3.036744713703804166, 1.534133291490011430 ) ) ;
#19290 = CARTESIAN_POINT ( 'NONE',  ( -56.58155989232411542, -1.962990915244706924, -3.400000000000206857 ) ) ;
#19291 = DIRECTION ( 'NONE',  ( 1.057355261547768637E-14, 0.000000000000000000, 1.000000000000000000 ) ) ;
#19292 = EDGE_CURVE ( 'NONE', #20389, #28184, #23088, .T. ) ;
#19293 = CARTESIAN_POINT ( 'NONE',  ( 48.40000000000001990, 1.391941090707534245, 3.850000000000022737 ) ) ;
#19294 = EDGE_CURVE ( 'NONE', #29446, #3316, #17012, .T. ) ;
#19295 = CARTESIAN_POINT ( 'NONE',  ( -54.49999999999999289, 1.399999999999995914, 3.959797974644418961 ) ) ;
#19296 = EDGE_CURVE ( 'NONE', #76, #9362, #4352, .T. ) ;
#19297 = AXIS2_PLACEMENT_3D ( 'NONE', #13087, #22613, #22773 ) ;
#19298 = CARTESIAN_POINT ( 'NONE',  ( -36.92405921417685732, 0.1434351685890311867, 5.407416993630365987 ) ) ;
#19299 = VERTEX_POINT ( 'NONE', #8953 ) ;
#19300 = CARTESIAN_POINT ( 'NONE',  ( -59.19999999999997442, -3.399999999999991473, -2.218921219761684346E-13 ) ) ;
#19301 = CARTESIAN_POINT ( 'NONE',  ( -54.49181037333889321, 1.522049374736507144, 3.314263409011526385 ) ) ;
#19302 = CARTESIAN_POINT ( 'NONE',  ( 53.91582462592152325, 6.672259099522126036, -1.484311132272649436 ) ) ;
#19303 = VERTEX_POINT ( 'NONE', #16095 ) ;
#19304 = ADVANCED_FACE ( 'NONE', ( #19226 ), #28867, .F. ) ;
#19305 = CARTESIAN_POINT ( 'NONE',  ( -54.48478889579405404, 1.513794642953540270, 4.039462313877656641 ) ) ;
#19306 = EDGE_LOOP ( 'NONE', ( #26920, #8622, #24144, #2315 ) ) ;
#19307 = CARTESIAN_POINT ( 'NONE',  ( 47.07708546080149148, 8.766223091587903582, -1.550000000000163469 ) ) ;
#19309 = CARTESIAN_POINT ( 'NONE',  ( 47.21358082890262864, -3.755449232595078346, -1.648679025009969878 ) ) ;
#19308 = CARTESIAN_POINT ( 'NONE',  ( -57.49999999999995737, 2.356882582050588150E-14, -3.400000000000204636 ) ) ;
#19310 = EDGE_LOOP ( 'NONE', ( #30346, #6057, #4139, #18187 ) ) ;
#19311 = DIRECTION ( 'NONE',  ( 0.000000000000000000, 0.000000000000000000, 1.000000000000000000 ) ) ;
#19312 = LINE ( 'NONE', #10253, #1385 ) ;
#19314 = CARTESIAN_POINT ( 'NONE',  ( -60.48535533905928219, -0.8667965836981817995, 4.226679811941401965 ) ) ;
#19313 = DIRECTION ( 'NONE',  ( 0.000000000000000000, 0.000000000000000000, 1.000000000000000000 ) ) ;
#19315 = ORIENTED_EDGE ( 'NONE', *, *, #27210, .T. ) ;
#19316 = CARTESIAN_POINT ( 'NONE',  ( -56.37499999999997158, -3.673546848079173532, -0.7533615035078063960 ) ) ;
#19317 = DIRECTION ( 'NONE',  ( 1.000000000000000000, 3.054025858079668409E-16, -2.042474015755241579E-16 ) ) ;
#19318 = CARTESIAN_POINT ( 'NONE',  ( 47.04570146981701129, -4.276948333784440059, -0.9210526315789477891 ) ) ;
#19319 = EDGE_CURVE ( 'NONE', #20522, #133, #8910, .T. ) ;
#19320 = CARTESIAN_POINT ( 'NONE',  ( 15.59055531549693718, -3.917775493694396260, -3.727542820438248583 ) ) ;
#19321 = AXIS2_PLACEMENT_3D ( 'NONE', #12282, #9632, #11992 ) ;
#19322 = DIRECTION ( 'NONE',  ( -0.7542528389311653481, -0.5142632992712595774, -0.4082106245394850341 ) ) ;
#19323 = DIRECTION ( 'NONE',  ( -0.4772254810013855097, 0.8787808829753844808, 1.772289120718281137E-15 ) ) ;
#19324 = CARTESIAN_POINT ( 'NONE',  ( 58.45000000000001705, 0.8000000000000000444, 2.421260002560649660 ) ) ;
#19325 = ORIENTED_EDGE ( 'NONE', *, *, #18301, .T. ) ;
#19326 = EDGE_CURVE ( 'NONE', #28946, #12544, #20907, .T. ) ;
#19327 = CARTESIAN_POINT ( 'NONE',  ( -58.81249999999996447, -0.7533615035078081723, 3.673546848079176197 ) ) ;
#19328 = CARTESIAN_POINT ( 'NONE',  ( 15.68751737981906302, -3.461789369942958050, 4.158232265984262988 ) ) ;
#19329 = ADVANCED_FACE ( 'NONE', ( #18314 ), #5557, .T. ) ;
#19330 = CARTESIAN_POINT ( 'NONE',  ( 48.46374521131294699, 1.419210040599422795, -3.846553521706499446 ) ) ;
#19331 = CARTESIAN_POINT ( 'NONE',  ( 30.12780005191093480, 6.637137500361657949, -1.950000000000104539 ) ) ;
#19332 = EDGE_CURVE ( 'NONE', #10573, #29731, #2833, .T. ) ;
#19333 = CARTESIAN_POINT ( 'NONE',  ( -62.06004451743454808, -2.681695334896316840, 0.2250289189416591340 ) ) ;
#19335 = CARTESIAN_POINT ( 'NONE',  ( -59.40411988557205092, 3.289922720809018930, -1.067712145749284858 ) ) ;
#19334 = CYLINDRICAL_SURFACE ( 'NONE', #9503, 0.1000000000000000472 ) ;
#19336 = AXIS2_PLACEMENT_3D ( 'NONE', #6796, #23589, #6641 ) ;
#19337 = DIRECTION ( 'NONE',  ( 5.585208838990483560E-16, -0.05332224631853142716, -0.9985773570673159849 ) ) ;
#19339 = DIRECTION ( 'NONE',  ( 0.000000000000000000, 1.000000000000000000, 0.000000000000000000 ) ) ;
#19338 = CARTESIAN_POINT ( 'NONE',  ( 58.75000000000002132, -0.6121634413829184496, -1.877732920580952980 ) ) ;
#19340 = ORIENTED_EDGE ( 'NONE', *, *, #24213, .F. ) ;
#19341 = CIRCLE ( 'NONE', #3633, 159.7997717543496776 ) ;
#19342 = LINE ( 'NONE', #21406, #675 ) ;
#19343 = UNCERTAINTY_MEASURE_WITH_UNIT (LENGTH_MEASURE( 1.000000000000000082E-05 ), #24746, 'distance_accuracy_value', 'NONE');
#19344 = CARTESIAN_POINT ( 'NONE',  ( 58.75000000000000711, 1.039502773797200019, -1.800471618823823450 ) ) ;
#19346 = CYLINDRICAL_SURFACE ( 'NONE', #27775, 0.05000000000000143219 ) ;
#19345 = CARTESIAN_POINT ( 'NONE',  ( 52.06628335902946247, -0.5434431642975677823, -1.718465885608440713 ) ) ;
#19347 = DIRECTION ( 'NONE',  ( 1.000000000000000000, 5.570239943078649173E-15, -9.650165233620068940E-15 ) ) ;
#19348 = EDGE_LOOP ( 'NONE', ( #4110, #221, #22116, #20820 ) ) ;
#19349 = ORIENTED_EDGE ( 'NONE', *, *, #21802, .F. ) ;
#19350 =( BOUNDED_CURVE ( )  B_SPLINE_CURVE ( 2, ( #23065, #19067, #12093, #6861, #21771, #1363, #11176, #31251, #11030 ),
 .UNSPECIFIED., .F., .T. ) 
 B_SPLINE_CURVE_WITH_KNOTS ( ( 3, 2, 2, 2, 3 ),
 ( 0.6388888888888889506, 0.6481481481481481399, 0.6666666666666666297, 0.6851851851851852304, 0.6944444444444445308 ),
 .UNSPECIFIED. ) 
 CURVE ( )  GEOMETRIC_REPRESENTATION_ITEM ( )  RATIONAL_B_SPLINE_CURVE ( ( 0.9330127018922194093, 0.9330127018922197424, 1.000000000000000000, 0.8660254037844387076, 1.000000000000000000, 0.8660254037844387076, 1.000000000000000000, 0.9330127018922189652, 0.9330127018922194093 ) ) 
 REPRESENTATION_ITEM ( '' )  );
#19351 = EDGE_LOOP ( 'NONE', ( #21453, #6864, #20977, #19997, #6403, #26508, #21569, #9723, #23701, #23781, #7335, #25290, #29537 ) ) ;
#19352 = CARTESIAN_POINT ( 'NONE',  ( 51.89161117884418672, 9.098400920928359170, -2.050000000000180123 ) ) ;
#19353 = CARTESIAN_POINT ( 'NONE',  ( -67.91948434493399134, -6.091656077594763675E-16, 3.386362506249485869E-15 ) ) ;
#19354 = ORIENTED_EDGE ( 'NONE', *, *, #7132, .F. ) ;
#19355 = EDGE_CURVE ( 'NONE', #4097, #16699, #305, .T. ) ;
#19356 = PLANE ( 'NONE',  #4084 ) ;
#19357 = ORIENTED_EDGE ( 'NONE', *, *, #2449, .F. ) ;
#19358 = SURFACE_STYLE_USAGE ( .BOTH. , #23792 ) ;
#19359 = ADVANCED_FACE ( 'NONE', ( #653 ), #21056, .T. ) ;
#19360 = CARTESIAN_POINT ( 'NONE',  ( -59.70655989232412253, -3.925981830489445379, -2.260242286469037332E-13 ) ) ;
#19361 = ORIENTED_EDGE ( 'NONE', *, *, #17564, .T. ) ;
#19362 = ADVANCED_FACE ( 'NONE', ( #3188 ), #19374, .T. ) ;
#19363 = ORIENTED_EDGE ( 'NONE', *, *, #10083, .F. ) ;
#19364 = ORIENTED_EDGE ( 'NONE', *, *, #15227, .T. ) ;
#19365 = CARTESIAN_POINT ( 'NONE',  ( -56.63452994616203284, 2.093608279459369510E-14, -3.600000000000201261 ) ) ;
#19366 = FACE_OUTER_BOUND ( 'NONE', #13004, .T. ) ;
#19367 = DIRECTION ( 'NONE',  ( 0.9993908270190958731, -0.03489949670249358621, -4.336808689942082423E-15 ) ) ;
#19368 = DIRECTION ( 'NONE',  ( 0.000000000000000000, 0.000000000000000000, 1.000000000000000000 ) ) ;
#19369 = DIRECTION ( 'NONE',  ( -0.9926670569371645048, -0.1208805777273925935, 3.449037773238375127E-15 ) ) ;
#19370 = CARTESIAN_POINT ( 'NONE',  ( -59.09999999999998010, -2.331118226142294247, 1.260312586522342349 ) ) ;
#19371 = CIRCLE ( 'NONE', #25424, 0.04999999999999991257 ) ;
#19372 = CARTESIAN_POINT ( 'NONE',  ( 48.48434962373865886, 1.386108502191577108, -3.851082811767820413 ) ) ;
#19374 = PLANE ( 'NONE',  #29126 ) ;
#19373 = CARTESIAN_POINT ( 'NONE',  ( 54.40000000000001990, 1.029992063861229212E-15, -4.375000000000002665 ) ) ;
#19375 = VERTEX_POINT ( 'NONE', #26647 ) ;
#19376 = FACE_OUTER_BOUND ( 'NONE', #25425, .T. ) ;
#19377 = DIRECTION ( 'NONE',  ( 0.3420201433256648826, 0.02340144900402444869, -0.9394011889198372600 ) ) ;
#19379 = CARTESIAN_POINT ( 'NONE',  ( -71.44999999999998863, -1.380331489585512972E-15, 2.906968604901091669E-15 ) ) ;
#19378 = CARTESIAN_POINT ( 'NONE',  ( 56.95000000000001705, 0.000000000000000000, 0.000000000000000000 ) ) ;
#19380 = CARTESIAN_POINT ( 'NONE',  ( 47.00000000000002842, -4.020776289669855785, 2.234582293948414122 ) ) ;
#19381 = ORIENTED_EDGE ( 'NONE', *, *, #18597, .T. ) ;
#19382 = DIRECTION ( 'NONE',  ( 1.000000000000000000, -1.219044193948983948E-29, 3.491481338843133355E-15 ) ) ;
#19383 = ORIENTED_EDGE ( 'NONE', *, *, #21151, .F. ) ;
#19384 = CARTESIAN_POINT ( 'NONE',  ( 49.00000000000002132, 3.252606517456513302E-16, -5.132477568099407673E-13 ) ) ;
#19385 = CARTESIAN_POINT ( 'NONE',  ( -58.63452994616204705, 3.117691453623979481, 1.799999999999803757 ) ) ;
#19386 = ORIENTED_EDGE ( 'NONE', *, *, #7255, .T. ) ;
#19387 = VERTEX_POINT ( 'NONE', #7948 ) ;
#19388 = EDGE_CURVE ( 'NONE', #26655, #7417, #16503, .T. ) ;
#19389 = CARTESIAN_POINT ( 'NONE',  ( 15.66436536804550883, 5.008501212420992665, 2.048848402342041908 ) ) ;
#19390 = EDGE_LOOP ( 'NONE', ( #3630, #28746, #30100, #1138, #28253, #5802, #17799, #8727 ) ) ;
#19391 = ADVANCED_FACE ( 'NONE', ( #22511 ), #19546, .T. ) ;
#19392 = CARTESIAN_POINT ( 'NONE',  ( 48.41298237836545582, -1.088467210617550807, 3.899823238510139678 ) ) ;
#19393 = CARTESIAN_POINT ( 'NONE',  ( -56.32202994616206126, 2.078460969082646770, 3.599999999999807354 ) ) ;
#19394 = EDGE_LOOP ( 'NONE', ( #27420, #22198, #10320, #20042, #8302, #28417 ) ) ;
#19395 = CARTESIAN_POINT ( 'NONE',  ( 54.40000000000001990, -1.084202172485504434E-16, 4.374999999999999112 ) ) ;
#19396 = EDGE_CURVE ( 'NONE', #24201, #13873, #5575, .T. ) ;
#19397 = FACE_OUTER_BOUND ( 'NONE', #2179, .T. ) ;
#19398 = CARTESIAN_POINT ( 'NONE',  ( 29.19109589768859792, 6.114704649262250769, 2.049999999999898126 ) ) ;
#19399 = ORIENTED_EDGE ( 'NONE', *, *, #26831, .F. ) ;
#19400 = DIRECTION ( 'NONE',  ( 0.000000000000000000, -0.9615843008030765526, -0.2745098039215693730 ) ) ;
#19401 = CARTESIAN_POINT ( 'NONE',  ( 51.65273894882757588, 3.822289909571943145, -2.050000000000175682 ) ) ;
#19402 = CARTESIAN_POINT ( 'NONE',  ( 58.65000000000002700, -1.022750809560353469, -1.571497941946597976 ) ) ;
#19403 = CARTESIAN_POINT ( 'NONE',  ( 58.75000000000002132, 6.153735859711025284E-13, 3.111507638930570854E-58 ) ) ;
#19404 = DIRECTION ( 'NONE',  ( 0.000000000000000000, 0.000000000000000000, -1.000000000000000000 ) ) ;
#19405 = EDGE_CURVE ( 'NONE', #16179, #10988, #17445, .T. ) ;
#19407 = FACE_OUTER_BOUND ( 'NONE', #2184, .T. ) ;
#19406 = CARTESIAN_POINT ( 'NONE',  ( -36.30424252565905618, -3.146183597690385803, 4.141717300434374138 ) ) ;
#19408 = CARTESIAN_POINT ( 'NONE',  ( 51.55144386500324316, 1.037443573995146862, 1.251214392908886142 ) ) ;
#19409 = CARTESIAN_POINT ( 'NONE',  ( -44.49999999999997868, 8.366749974758269874E-15, -1.589829192029513996E-13 ) ) ;
#19410 = CARTESIAN_POINT ( 'NONE',  ( 53.21917409580247238, 8.083376426877231680, 1.902110155464532104 ) ) ;
#19411 = CIRCLE ( 'NONE', #12288, 0.05000000000000009298 ) ;
#19412 = EDGE_LOOP ( 'NONE', ( #19702, #8685, #5807, #4502, #16220 ) ) ;
#19413 = VECTOR ( 'NONE', #10485, 1000.000000000000000 ) ;
#19414 = VERTEX_POINT ( 'NONE', #2583 ) ;
#19415 = CARTESIAN_POINT ( 'NONE',  ( 51.88138499675474691, 0.02607891777379810205, -4.373234472033241893 ) ) ;
#19416 = VERTEX_POINT ( 'NONE', #12231 ) ;
#19417 = DIRECTION ( 'NONE',  ( 1.047444401652940007E-14, -1.000000000000000000, 0.000000000000000000 ) ) ;
#19418 = CARTESIAN_POINT ( 'NONE',  ( -60.22085481156723574, 2.489203624310591945, -2.804704140674918467 ) ) ;
#19420 = CARTESIAN_POINT ( 'NONE',  ( -61.34999999999997300, -2.565134197206211386, 0.6652717868084008224 ) ) ;
#19419 = CARTESIAN_POINT ( 'NONE',  ( 47.09104525948222886, 9.165979422395331255, -1.950000000000163380 ) ) ;
#19421 = ORIENTED_EDGE ( 'NONE', *, *, #17155, .F. ) ;
#19422 = ORIENTED_EDGE ( 'NONE', *, *, #6943, .T. ) ;
#19423 = CARTESIAN_POINT ( 'NONE',  ( 60.97408713704741956, 0.7545809820805179369, -1.439897579195099864 ) ) ;
#19424 = VERTEX_POINT ( 'NONE', #194 ) ;
#19425 = EDGE_CURVE ( 'NONE', #5085, #2901, #15225, .T. ) ;
#19426 = CARTESIAN_POINT ( 'NONE',  ( 31.30720621464601905, 7.411182539856417506, -1.950000000000108535 ) ) ;
#19427 = EDGE_LOOP ( 'NONE', ( #430, #26964, #3789, #6212 ) ) ;
#19428 = CARTESIAN_POINT ( 'NONE',  ( 58.65000000000003411, -1.671477153793470949, 0.8495817349404535257 ) ) ;
#19429 = EDGE_CURVE ( 'NONE', #29589, #1037, #14755, .T. ) ;
#19430 = ORIENTED_EDGE ( 'NONE', *, *, #23787, .T. ) ;
#19431 = DIRECTION ( 'NONE',  ( 0.000000000000000000, -8.673617379884043361E-16, 1.000000000000000000 ) ) ;
#19432 = DIRECTION ( 'NONE',  ( 0.000000000000000000, 0.000000000000000000, 1.000000000000000000 ) ) ;
#19433 = CARTESIAN_POINT ( 'NONE',  ( 57.02114622761336449, 0.7499999999999982236, -1.778341845356538498 ) ) ;
#19435 = CARTESIAN_POINT ( 'NONE',  ( -60.88452994616204705, 3.117691453623979481, 1.799999999999795985 ) ) ;
#19434 = AXIS2_PLACEMENT_3D ( 'NONE', #31213, #12207, #14872 ) ;
#19436 = CARTESIAN_POINT ( 'NONE',  ( 52.98236138753809854, 8.264679131573773319, -2.050000000000184119 ) ) ;
#19438 = EDGE_CURVE ( 'NONE', #28678, #21812, #9023, .T. ) ;
#19437 = B_SPLINE_CURVE_WITH_KNOTS ( 'NONE', 3,
 ( #23941, #26314, #21421, #26155, #26620, #19041, #9551, #24095, #12214, #19209 ),
 .UNSPECIFIED., .F., .F.,
 ( 4, 2, 2, 2, 4 ),
 ( 0.000000000000000000, 0.0003926182454497113513, 0.0007852364908994227026, 0.001177854736349134108, 0.001570472981798845405 ),
 .UNSPECIFIED. ) ;
#19439 = CARTESIAN_POINT ( 'NONE',  ( -54.44999999999997442, -6.938893903907228378E-14, 0.000000000000000000 ) ) ;
#19440 = CARTESIAN_POINT ( 'NONE',  ( 50.38693217303928407, 1.296871156637316114, -3.889656364559859192 ) ) ;
#19441 = VECTOR ( 'NONE', #14359, 1000.000000000000000 ) ;
#19442 = DIRECTION ( 'NONE',  ( 1.000000000000000000, 1.047444401652940007E-14, 0.000000000000000000 ) ) ;
#19443 = ORIENTED_EDGE ( 'NONE', *, *, #5015, .T. ) ;
#19444 = CARTESIAN_POINT ( 'NONE',  ( -54.44999999999997442, -1.499999999999999556, -4.029888335921975262 ) ) ;
#19445 = EDGE_CURVE ( 'NONE', #29912, #6282, #5660, .T. ) ;
#19447 = CARTESIAN_POINT ( 'NONE',  ( 58.65000000000000568, 1.253243060178336643, -1.394635017528379928 ) ) ;
#19446 = CARTESIAN_POINT ( 'NONE',  ( -36.11187263677957304, -2.734387802834445047, -4.440904455451657462 ) ) ;
#19448 = CARTESIAN_POINT ( 'NONE',  ( 53.94293340116774260, 6.381487143331855627, -2.142504121165067499E-08 ) ) ;
#19449 = AXIS2_PLACEMENT_3D ( 'NONE', #9961, #17247, #19635 ) ;
#19450 = ORIENTED_EDGE ( 'NONE', *, *, #16045, .T. ) ;
#19451 = DIRECTION ( 'NONE',  ( -1.000000000000000000, 1.219044193948983948E-29, -3.491481338843133355E-15 ) ) ;
#19452 = EDGE_LOOP ( 'NONE', ( #7369, #1977, #5769, #3152 ) ) ;
#19453 = CIRCLE ( 'NONE', #17401, 1.375000000000001332 ) ;
#19454 = CARTESIAN_POINT ( 'NONE',  ( -36.50489844130355266, -5.024465639092029257, 2.007392901578141320 ) ) ;
#19456 = CARTESIAN_POINT ( 'NONE',  ( 47.88186413446628364, -3.908336260473453727, -1.238913909466087926 ) ) ;
#19455 = CARTESIAN_POINT ( 'NONE',  ( 58.75000000000000711, 1.077297519405725712, -1.655311165516502703 ) ) ;
#19457 = ORIENTED_EDGE ( 'NONE', *, *, #7840, .F. ) ;
#19458 = CARTESIAN_POINT ( 'NONE',  ( 51.59739104186227365, 1.010292945603182169, -1.272765950230260401 ) ) ;
#19459 = EDGE_CURVE ( 'NONE', #2526, #28401, #8404, .T. ) ;
#19460 = DIRECTION ( 'NONE',  ( 0.000000000000000000, 0.000000000000000000, -1.000000000000000000 ) ) ;
#19462 = CARTESIAN_POINT ( 'NONE',  ( -54.48118151432741030, -1.510613940323803916, -4.037256667234632168 ) ) ;
#19461 = DIRECTION ( 'NONE',  ( 0.000000000000000000, -0.4531102586355347794, 0.8914544820231926625 ) ) ;
#19463 = ORIENTED_EDGE ( 'NONE', *, *, #23340, .T. ) ;
#19464 = CARTESIAN_POINT ( 'NONE',  ( -59.18749999999996447, 0.8699069336946683162, -4.241846523238426592 ) ) ;
#19465 = AXIS2_PLACEMENT_3D ( 'NONE', #22934, #17722, #3142 ) ;
#19466 = CARTESIAN_POINT ( 'NONE',  ( -57.22499999999997300, -0.9241234443029057166, 4.506217466977124886 ) ) ;
#19467 = CARTESIAN_POINT ( 'NONE',  ( -54.49999999999997158, -3.745083032500879039, 0.1919715595446555012 ) ) ;
#19468 = CARTESIAN_POINT ( 'NONE',  ( 60.75000000000002842, -0.4999999999993638977, 1.718465885608440047 ) ) ;
#19469 = LINE ( 'NONE', #2819, #7861 ) ;
#19470 = DIRECTION ( 'NONE',  ( -1.000000000000000000, 0.000000000000000000, 0.000000000000000000 ) ) ;
#19471 = FACE_OUTER_BOUND ( 'NONE', #5537, .T. ) ;
#19473 = ORIENTED_EDGE ( 'NONE', *, *, #19916, .T. ) ;
#19472 = CIRCLE ( 'NONE', #4778, 3.000000000000000000 ) ;
#19474 = EDGE_CURVE ( 'NONE', #5081, #22862, #29829, .T. ) ;
#19475 = CARTESIAN_POINT ( 'NONE',  ( 61.21684424624501730, 0.7974861228896987786, -1.837019011344032782 ) ) ;
#19476 = AXIS2_PLACEMENT_3D ( 'NONE', #24175, #4536, #16890 ) ;
#19477 = CARTESIAN_POINT ( 'NONE',  ( 30.62824136006083720, 6.974337361240579014, -1.950000000000106759 ) ) ;
#19478 = CARTESIAN_POINT ( 'NONE',  ( 58.45000000000001705, 0.8000000000000000444, -1.778341924377873751 ) ) ;
#19479 = VECTOR ( 'NONE', #14585, 1000.000000000000000 ) ;
#19480 = DIRECTION ( 'NONE',  ( 0.000000000000000000, 1.000000000000000000, 0.000000000000000000 ) ) ;
#19481 = EDGE_CURVE ( 'NONE', #17058, #15357, #26100, .T. ) ;
#19482 = CARTESIAN_POINT ( 'NONE',  ( -56.74999999999997158, 3.673546848079180638, 0.7533615035078086164 ) ) ;
#19484 = CYLINDRICAL_SURFACE ( 'NONE', #5395, 2.000000000000000000 ) ;
#19483 = CARTESIAN_POINT ( 'NONE',  ( 51.25000000000002842, -0.6499999999994634514, -1.489337100860647967 ) ) ;
#19485 = EDGE_LOOP ( 'NONE', ( #29725, #4285, #11404, #9174 ) ) ;
#19486 = CARTESIAN_POINT ( 'NONE',  ( 58.64999999999999858, 0.9947034709632315286, -1.589751505945539378 ) ) ;
#19487 = DIRECTION ( 'NONE',  ( 1.000000000000000000, -1.219044193948983948E-29, 3.491481338843133355E-15 ) ) ;
#19489 = CARTESIAN_POINT ( 'NONE',  ( 48.00000000000002842, -3.657334280697315698, 2.105684202162165342 ) ) ;
#19488 = CARTESIAN_POINT ( 'NONE',  ( 15.57907767661744991, -2.743848709681487197, -4.666930520580701014 ) ) ;
#19490 = DIRECTION ( 'NONE',  ( -1.000000000000000000, -0.000000000000000000, -0.000000000000000000 ) ) ;
#19491 = ORIENTED_EDGE ( 'NONE', *, *, #15289, .F. ) ;
#19492 = CIRCLE ( 'NONE', #7348, 0.1000000000000000472 ) ;
#19493 = ORIENTED_EDGE ( 'NONE', *, *, #30930, .T. ) ;
#19494 = DIRECTION ( 'NONE',  ( -1.000000000000000000, -0.000000000000000000, 1.047444401652940007E-14 ) ) ;
#19495 = TOROIDAL_SURFACE ( 'NONE', #5833, 1.975000000000001865, 0.1000000000000000056 ) ;
#19496 = EDGE_CURVE ( 'NONE', #16069, #6234, #30163, .T. ) ;
#19497 = ORIENTED_EDGE ( 'NONE', *, *, #29717, .F. ) ;
#19498 = CARTESIAN_POINT ( 'NONE',  ( 51.70652201333279407, -4.179189514726790122, 0.9999999999996741495 ) ) ;
#19499 = EDGE_CURVE ( 'NONE', #30383, #23530, #6927, .T. ) ;
#19500 = DIRECTION ( 'NONE',  ( -1.000000000000000000, -0.000000000000000000, 1.047444401652940007E-14 ) ) ;
#19501 = EDGE_LOOP ( 'NONE', ( #7962, #11074, #23789, #5433 ) ) ;
#19502 = EDGE_CURVE ( 'NONE', #19797, #23537, #13290, .T. ) ;
#19503 = FACE_OUTER_BOUND ( 'NONE', #22663, .T. ) ;
#19504 = ORIENTED_EDGE ( 'NONE', *, *, #7021, .F. ) ;
#19505 =( NAMED_UNIT ( * ) PLANE_ANGLE_UNIT ( ) SI_UNIT ( $, .RADIAN. ) );
#19506 = TOROIDAL_SURFACE ( 'NONE', #1281, 2.750000000000000000, 0.1000000000000000056 ) ;
#19507 = CARTESIAN_POINT ( 'NONE',  ( 58.75000000000003553, -1.457351493771257722, -1.320164791809644411 ) ) ;
#19508 =( LENGTH_UNIT ( ) NAMED_UNIT ( * ) SI_UNIT ( .MILLI., .METRE. ) );
#19509 = AXIS2_PLACEMENT_3D ( 'NONE', #30611, #17867, #1634 ) ;
#19510 = ORIENTED_EDGE ( 'NONE', *, *, #17724, .F. ) ;
#19511 = ORIENTED_EDGE ( 'NONE', *, *, #6526, .T. ) ;
#19512 = CARTESIAN_POINT ( 'NONE',  ( -59.25952994616205416, -4.643455692769875931E-15, 3.599999999999788702 ) ) ;
#19513 = CARTESIAN_POINT ( 'NONE',  ( 53.25639650609795694, 8.250950595073881288, -2.050000000000185452 ) ) ;
#19514 = CARTESIAN_POINT ( 'NONE',  ( 61.00000000000003553, -0.9999999999993611777, -1.586072192556190252 ) ) ;
#19515 = CARTESIAN_POINT ( 'NONE',  ( -54.49181037333889321, -1.522049374736507588, 3.314263409011525496 ) ) ;
#19516 = TOROIDAL_SURFACE ( 'NONE', #22046, 4.000000000000022204, 0.1000000000000000056 ) ;
#19517 = AXIS2_PLACEMENT_3D ( 'NONE', #12155, #7403, #19760 ) ;
#19518 = DIRECTION ( 'NONE',  ( -1.000000000000000000, -3.053848253006669023E-16, 2.042510438544995415E-16 ) ) ;
#19519 = AXIS2_PLACEMENT_3D ( 'NONE', #21295, #18902, #28544 ) ;
#19521 = CARTESIAN_POINT ( 'NONE',  ( -36.68133364217572989, -0.7247683022691534527, -5.358970532132250497 ) ) ;
#19520 = CARTESIAN_POINT ( 'NONE',  ( -59.23418654921033522, -3.153953023162030078, 1.269874138521803975 ) ) ;
#19523 = EDGE_CURVE ( 'NONE', #4176, #24464, #1126, .T. ) ;
#19522 = CIRCLE ( 'NONE', #23561, 4.800000000000000711 ) ;
#19524 = CARTESIAN_POINT ( 'NONE',  ( 46.90000006803324339, -4.241636233590472926, 1.073352279313351865 ) ) ;
#19525 = CARTESIAN_POINT ( 'NONE',  ( 15.03925126672132961, -4.018128179617543871, 3.618665901676652918 ) ) ;
#19526 = VECTOR ( 'NONE', #12402, 1000.000000000000000 ) ;
#19528 = CARTESIAN_POINT ( 'NONE',  ( 69.20000000000005969, 0.8558823529411765385, 2.268940368965341126 ) ) ;
#19527 = CARTESIAN_POINT ( 'NONE',  ( 54.49989931805382071, -0.003076767800981534788, -4.280178505497699959 ) ) ;
#19529 = ORIENTED_EDGE ( 'NONE', *, *, #2101, .T. ) ;
#19530 =( BOUNDED_SURFACE ( )  B_SPLINE_SURFACE ( 3, 2, ( 
 ( #30016, #25279, #8641 ),
 ( #20853, #4203, #23069 ),
 ( #11321, #18638, #25748 ),
 ( #25580, #16252, #21007 ),
 ( #1366, #30645, #8958 ),
 ( #13547, #8496, #23230 ),
 ( #30482, #6594, #18321 ),
 ( #22914, #15780, #25429 ),
 ( #3592, #6273, #15919 ),
 ( #8785, #1518, #3899 ) ),
 .UNSPECIFIED., .F., .F., .F. ) 
 B_SPLINE_SURFACE_WITH_KNOTS ( ( 4, 2, 2, 2, 4 ),
 ( 3, 3 ),
 ( -5.421010862427522170E-20, 0.0003537438758377288439, 0.0007074877516754576878, 0.001061231627513186532, 0.001414975503350915376 ),
 ( 0.000000000000000000, 1.000000000000000000 ),
 .UNSPECIFIED. ) 
 GEOMETRIC_REPRESENTATION_ITEM ( )  RATIONAL_B_SPLINE_SURFACE ( (
 ( 1.000000000000000000, 0.7154752000627009334, 1.000000000000000000),
 ( 1.000000000000000000, 0.7154106121891214976, 1.000000000000000000),
 ( 1.000000000000000000, 0.7173719856077137580, 1.000000000000000000),
 ( 1.000000000000000000, 0.7229186815317750758, 1.000000000000000000),
 ( 1.000000000000000000, 0.7264660769275549379, 1.000000000000000000),
 ( 1.000000000000000000, 0.7305267549316539766, 1.000000000000000000),
 ( 1.000000000000000000, 0.7309418327392975812, 1.000000000000000000),
 ( 1.000000000000000000, 0.7246992783963228657, 1.000000000000000000),
 ( 1.000000000000000000, 0.7179850693090684688, 1.000000000000000000),
 ( 1.000000000000000000, 0.7071067811865482389, 1.000000000000000000) ) ) 
 REPRESENTATION_ITEM ( '' )  SURFACE ( )  );
#19531 = CARTESIAN_POINT ( 'NONE',  ( 33.47623932017462778, 5.407411300779134677, 0.000000000000000000 ) ) ;
#19532 = AXIS2_PLACEMENT_3D ( 'NONE', #13801, #23487, #20358 ) ;
#19533 = EDGE_CURVE ( 'NONE', #6367, #28516, #14996, .T. ) ;
#19534 = DIRECTION ( 'NONE',  ( 0.000000000000000000, -0.2008964009354147484, 0.9796124928211139560 ) ) ;
#19536 = CARTESIAN_POINT ( 'NONE',  ( 41.48619405472010868, -151.3359592902261852, 1.549999999999835953 ) ) ;
#19535 = CARTESIAN_POINT ( 'NONE',  ( 48.40134283869316789, -0.9106118309512859499, 3.923752762110600312 ) ) ;
#19537 = CARTESIAN_POINT ( 'NONE',  ( 47.49114655384919104, -4.380199991372831114, 1.408811060053114739 ) ) ;
#19538 = EDGE_LOOP ( 'NONE', ( #17462, #18319, #8495, #13943, #7333, #1883, #6206, #6313, #31004, #20596, #12765, #10565 ) ) ;
#19539 = CARTESIAN_POINT ( 'NONE',  ( -61.39879105983192886, -2.652949782970507098, 0.5017753628371410812 ) ) ;
#19540 = VECTOR ( 'NONE', #23570, 1000.000000000000000 ) ;
#19541 = ORIENTED_EDGE ( 'NONE', *, *, #23961, .T. ) ;
#19542 = FACE_OUTER_BOUND ( 'NONE', #24279, .T. ) ;
#19543 = ORIENTED_EDGE ( 'NONE', *, *, #22679, .T. ) ;
#19544 = ORIENTED_EDGE ( 'NONE', *, *, #2933, .F. ) ;
#19545 = EDGE_CURVE ( 'NONE', #7685, #4534, #29664, .T. ) ;
#19546 = TOROIDAL_SURFACE ( 'NONE', #5874, 4.050000000000000711, 0.05000000000000000278 ) ;
#19547 = DIRECTION ( 'NONE',  ( 0.000000000000000000, 0.000000000000000000, -1.000000000000000000 ) ) ;
#19548 = ORIENTED_EDGE ( 'NONE', *, *, #25772, .T. ) ;
#19549 = AXIS2_PLACEMENT_3D ( 'NONE', #4437, #13437, #3796 ) ;
#19550 = DIRECTION ( 'NONE',  ( 0.000000000000000000, -0.9996898646859343485, -0.02490330187381124133 ) ) ;
#19551 = CARTESIAN_POINT ( 'NONE',  ( -55.07202994616204705, 2.078460969082674747, -3.600000000000187494 ) ) ;
#19552 = VERTEX_POINT ( 'NONE', #812 ) ;
#19553 = AXIS2_PLACEMENT_3D ( 'NONE', #5138, #14938, #7362 ) ;
#19554 = CARTESIAN_POINT ( 'NONE',  ( -56.37499999999998579, -1.162579938981958969E-14, 3.399999999999799183 ) ) ;
#19555 = DIRECTION ( 'NONE',  ( 3.491481338843133355E-15, 0.000000000000000000, 1.000000000000000000 ) ) ;
#19556 = CARTESIAN_POINT ( 'NONE',  ( 27.54696499482877314, 5.363421040582749377, 1.949999999999838307 ) ) ;
#19557 = EDGE_LOOP ( 'NONE', ( #29799, #29218, #28159, #15345 ) ) ;
#19558 = TOROIDAL_SURFACE ( 'NONE', #7912, 1.949999999999999956, 0.05000000000000000278 ) ;
#19559 = AXIS2_PLACEMENT_3D ( 'NONE', #29011, #29460, #22215 ) ;
#19560 = DIRECTION ( 'NONE',  ( 0.000000000000000000, -4.336808689942006692E-15, 1.000000000000000000 ) ) ;
#19561 = AXIS2_PLACEMENT_3D ( 'NONE', #9248, #28552, #16850 ) ;
#19562 = CARTESIAN_POINT ( 'NONE',  ( -54.49853245345825314, -1.536420219664552445, 4.055116445457032981 ) ) ;
#19563 = CARTESIAN_POINT ( 'NONE',  ( -60.59999999999997300, -2.464733277392923139, 0.9389111926722781831 ) ) ;
#19564 = CARTESIAN_POINT ( 'NONE',  ( 50.25000000000002842, -1.039502773796191937, -1.800471618824325493 ) ) ;
#19565 = CARTESIAN_POINT ( 'NONE',  ( 49.04999999999999716, 3.275930187719168862E-16, -2.675000000000512745 ) ) ;
#19566 = CONICAL_SURFACE ( 'NONE', #20137, 5.407411300779140895, 0.1317529408396977408 ) ;
#19568 = DIRECTION ( 'NONE',  ( 1.000000000000000000, 1.047444401652940007E-14, 0.000000000000000000 ) ) ;
#19567 = CARTESIAN_POINT ( 'NONE',  ( -35.85663232820583346, 4.383220986680242071, -0.4611378927884229317 ) ) ;
#19569 = B_SPLINE_CURVE_WITH_KNOTS ( 'NONE', 3,
 ( #10211, #24005, #21811, #19880 ),
 .UNSPECIFIED., .F., .F.,
 ( 4, 4 ),
 ( 1.084202172485504434E-19, 0.0001521069361438105792 ),
 .UNSPECIFIED. ) ;
#19570 = EDGE_CURVE ( 'NONE', #31281, #24820, #16553, .T. ) ;
#19571 = CIRCLE ( 'NONE', #31192, 4.050000000000000711 ) ;
#19572 = AXIS2_PLACEMENT_3D ( 'NONE', #19378, #7183, #29181 ) ;
#19573 = CARTESIAN_POINT ( 'NONE',  ( 51.19148447764911225, 0.9872860527330414859, 1.295557643792421443 ) ) ;
#19574 = EDGE_CURVE ( 'NONE', #26557, #18608, #16528, .T. ) ;
#19575 = DIRECTION ( 'NONE',  ( 0.000000000000000000, 0.9996898646859344595, 0.02490330187381124133 ) ) ;
#19576 = CARTESIAN_POINT ( 'NONE',  ( 58.75000000000002132, 6.153735859711025284E-13, 3.111507638930570854E-58 ) ) ;
#19577 = EDGE_LOOP ( 'NONE', ( #19241, #8721, #27501, #25871, #5693, #14988 ) ) ;
#19578 = CIRCLE ( 'NONE', #30171, 4.100000000000000533 ) ;
#19579 = CIRCLE ( 'NONE', #2363, 30.00000000000000355 ) ;
#19580 = ORIENTED_EDGE ( 'NONE', *, *, #5592, .T. ) ;
#19581 = ORIENTED_EDGE ( 'NONE', *, *, #6648, .T. ) ;
#19582 = CIRCLE ( 'NONE', #1359, 0.09999999999999982514 ) ;
#19583 = CIRCLE ( 'NONE', #6939, 0.09999999999999997780 ) ;
#19584 = CARTESIAN_POINT ( 'NONE',  ( 54.23679421920402177, 6.620234584472831862, 2.049999999999810640 ) ) ;
#19585 = CARTESIAN_POINT ( 'NONE',  ( -55.61042740578361077, -0.7887156198831598575, 3.845940847736173840 ) ) ;
#19587 = CYLINDRICAL_SURFACE ( 'NONE', #2863, 0.2500000000000000000 ) ;
#19586 = DIRECTION ( 'NONE',  ( 0.000000000000000000, 0.000000000000000000, 1.000000000000000000 ) ) ;
#19588 = ORIENTED_EDGE ( 'NONE', *, *, #28566, .T. ) ;
#19589 = VERTEX_POINT ( 'NONE', #28508 ) ;
#19590 = CARTESIAN_POINT ( 'NONE',  ( 68.00000000000000000, 0.7500000000000000000, -1.988246715074070581 ) ) ;
#19591 = EDGE_LOOP ( 'NONE', ( #5120, #27274, #27060, #29097, #13668, #9320 ) ) ;
#19592 = EDGE_CURVE ( 'NONE', #20831, #22178, #9530, .T. ) ;
#19593 = DIRECTION ( 'NONE',  ( 0.000000000000000000, 0.000000000000000000, 1.000000000000000000 ) ) ;
#19594 = ORIENTED_EDGE ( 'NONE', *, *, #29980, .F. ) ;
#19595 = CARTESIAN_POINT ( 'NONE',  ( 28.66473729876425125, 5.839050301630731354, -2.050000000000099298 ) ) ;
#19596 = ORIENTED_EDGE ( 'NONE', *, *, #18069, .T. ) ;
#19597 = DIRECTION ( 'NONE',  ( 0.5633368246415185743, -0.8262273428075417314, 0.000000000000000000 ) ) ;
#19598 = CIRCLE ( 'NONE', #5418, 1.613789466889706814 ) ;
#19599 = CARTESIAN_POINT ( 'NONE',  ( 58.45000000000001705, 0.000000000000000000, 0.000000000000000000 ) ) ;
#19600 = AXIS2_PLACEMENT_3D ( 'NONE', #30971, #9289, #21488 ) ;
#19601 = CIRCLE ( 'NONE', #18591, 0.1000000000000000472 ) ;
#19602 = CARTESIAN_POINT ( 'NONE',  ( 15.39414421509785669, -4.855742670514252346, -1.883114206442395133 ) ) ;
#19603 = CARTESIAN_POINT ( 'NONE',  ( -55.95655989232412963, -3.925981830489445379, -2.129311736262419800E-13 ) ) ;
#19604 = CARTESIAN_POINT ( 'NONE',  ( 51.87767605783385960, 8.699351266148436679, -2.050000000000180123 ) ) ;
#19605 = VECTOR ( 'NONE', #13709, 1000.000000000000000 ) ;
#19606 = CIRCLE ( 'NONE', #25631, 4.000000000000000000 ) ;
#19608 = AXIS2_PLACEMENT_3D ( 'NONE', #8442, #5922, #25848 ) ;
#19607 = CARTESIAN_POINT ( 'NONE',  ( 34.56702326949725546, 8.213851659285209550, 1.549999999999879696 ) ) ;
#19609 = CARTESIAN_POINT ( 'NONE',  ( 50.45647961155643912, 1.212999249975939886, -3.917061424767716016 ) ) ;
#19610 = DIRECTION ( 'NONE',  ( -1.000000000000000000, -3.054025858079668409E-16, 2.042474015755241579E-16 ) ) ;
#19611 = EDGE_CURVE ( 'NONE', #6604, #21318, #18070, .T. ) ;
#19612 = CARTESIAN_POINT ( 'NONE',  ( 63.50000000000005684, 2.908536147974962234E-16, 2.374999999999333422 ) ) ;
#19613 = ORIENTED_EDGE ( 'NONE', *, *, #1351, .T. ) ;
#19614 = CARTESIAN_POINT ( 'NONE',  ( 47.00000000000001421, -3.637377585518695611, -2.099877210783201331 ) ) ;
#19615 = TOROIDAL_SURFACE ( 'NONE', #9518, 4.275000000000000355, 0.1000000000000000056 ) ;
#19616 = CARTESIAN_POINT ( 'NONE',  ( -36.50489844130311212, -3.461789369942962047, -4.158232265984187492 ) ) ;
#19617 = CARTESIAN_POINT ( 'NONE',  ( 54.12874039445436836, 6.030813710072695066, 2.034055266290029085 ) ) ;
#19618 = ORIENTED_EDGE ( 'NONE', *, *, #22283, .T. ) ;
#19619 = CIRCLE ( 'NONE', #30744, 0.05000000000000017625 ) ;
#19620 = EDGE_LOOP ( 'NONE', ( #29884, #23226, #5542, #4564, #14317 ) ) ;
#19621 = CARTESIAN_POINT ( 'NONE',  ( 15.95705409078464498, -0.6016956010317232595, -5.375730734456591442 ) ) ;
#19622 = DIRECTION ( 'NONE',  ( 0.000000000000000000, 0.9996898646859344595, 0.02490330187381122745 ) ) ;
#19624 = LINE ( 'NONE', #24353, #7087 ) ;
#19623 = FACE_OUTER_BOUND ( 'NONE', #11463, .T. ) ;
#19625 = ORIENTED_EDGE ( 'NONE', *, *, #26310, .F. ) ;
#19626 = CIRCLE ( 'NONE', #7475, 5.407411300779133789 ) ;
#19627 = EDGE_CURVE ( 'NONE', #2253, #12845, #17037, .T. ) ;
#19628 = DIRECTION ( 'NONE',  ( 0.000000000000000000, 0.1576190026614809614, -0.9875000000000001554 ) ) ;
#19630 = FACE_OUTER_BOUND ( 'NONE', #25349, .T. ) ;
#19629 = CARTESIAN_POINT ( 'NONE',  ( 52.28361797084581042, 3.966539589492596107, 2.045539107969434056 ) ) ;
#19631 = VERTEX_POINT ( 'NONE', #21092 ) ;
#19632 = CARTESIAN_POINT ( 'NONE',  ( -58.31249999999997158, 4.108500314926511798, -1.367561758111407011 ) ) ;
#19633 = CARTESIAN_POINT ( 'NONE',  ( -35.85663232820584057, 2.686240680702099759, 4.475885388010746979 ) ) ;
#19634 = CARTESIAN_POINT ( 'NONE',  ( 56.96706223141283942, -0.7377629956704406800, 1.750942290135934831 ) ) ;
#19635 = DIRECTION ( 'NONE',  ( 1.057355261547768637E-14, 0.000000000000000000, 1.000000000000000000 ) ) ;
#19636 = DIRECTION ( 'NONE',  ( -0.9993908270190956511, 0.03489949670250202390, 3.491481338843132961E-15 ) ) ;
#19637 = LINE ( 'NONE', #2049, #10652 ) ;
#19638 = CARTESIAN_POINT ( 'NONE',  ( 57.05000000000001847, -0.7500000000000000000, -2.421260002560649660 ) ) ;
#19639 = ORIENTED_EDGE ( 'NONE', *, *, #14663, .F. ) ;
#19640 = CIRCLE ( 'NONE', #5977, 0.1000000000000006578 ) ;
#19641 = AXIS2_PLACEMENT_3D ( 'NONE', #6054, #27884, #13455 ) ;
#19642 = CARTESIAN_POINT ( 'NONE',  ( 16.07279755198632287, -3.436881753486524360, 4.177093996075195825 ) ) ;
#19643 = DIRECTION ( 'NONE',  ( 1.000000000000000000, 0.000000000000000000, 0.000000000000000000 ) ) ;
#19644 = FACE_OUTER_BOUND ( 'NONE', #6250, .T. ) ;
#19645 = EDGE_CURVE ( 'NONE', #18983, #6165, #28354, .T. ) ;
#19646 = CARTESIAN_POINT ( 'NONE',  ( -54.49999999999997868, -1.549999999999999600, -3.332135201338624952 ) ) ;
#19647 = B_SPLINE_CURVE_WITH_KNOTS ( 'NONE', 3,
 ( #21234, #19318, #21535, #16931, #7122, #14070 ),
 .UNSPECIFIED., .F., .F.,
 ( 4, 2, 4 ),
 ( 0.000000000000000000, 0.0001620412083492963143, 0.0003240824166985928996 ),
 .UNSPECIFIED. ) ;
#19648 = LINE ( 'NONE', #26596, #12081 ) ;
#19650 = CARTESIAN_POINT ( 'NONE',  ( 50.39883060428874018, -0.8930800907915671383, -3.925677024646228475 ) ) ;
#19649 = DIRECTION ( 'NONE',  ( 0.000000000000000000, 0.000000000000000000, 1.000000000000000000 ) ) ;
#19651 = VERTEX_POINT ( 'NONE', #13759 ) ;
#19652 = DIRECTION ( 'NONE',  ( -1.000000000000000000, 0.000000000000000000, 3.491481338843133355E-15 ) ) ;
#19653 = ORIENTED_EDGE ( 'NONE', *, *, #30535, .F. ) ;
#19654 = CARTESIAN_POINT ( 'NONE',  ( -54.54999999999998295, 3.780972210569126836E-15, -5.448124817252668230E-16 ) ) ;
#19656 = CARTESIAN_POINT ( 'NONE',  ( 58.75000000000004263, -2.008165151418373373, -0.5380862305909229759 ) ) ;
#19655 = CARTESIAN_POINT ( 'NONE',  ( -54.48922267869908609, -2.367328842898039021, -2.672487423992893074 ) ) ;
#19657 = CARTESIAN_POINT ( 'NONE',  ( -73.89999999999997726, -2.435524336289708093E-15, 4.607889071584891164E-15 ) ) ;
#19658 = ORIENTED_EDGE ( 'NONE', *, *, #19286, .F. ) ;
#19659 = AXIS2_PLACEMENT_3D ( 'NONE', #5372, #22183, #469 ) ;
#19660 = VERTEX_POINT ( 'NONE', #19191 ) ;
#19661 = CARTESIAN_POINT ( 'NONE',  ( 51.14630318392407560, -0.9364487020629673752, -1.503522130792586564 ) ) ;
#19662 = CIRCLE ( 'NONE', #8023, 0.1000000000000028644 ) ;
#19663 = CARTESIAN_POINT ( 'NONE',  ( -60.49999999999997868, 1.656632322739229403E-15, 1.870925083934595927E-15 ) ) ;
#19664 = ORIENTED_EDGE ( 'NONE', *, *, #14286, .T. ) ;
#19665 = CARTESIAN_POINT ( 'NONE',  ( 57.00000000000001421, -0.6820512820512794061, -1.773360101234991326 ) ) ;
#19666 = CARTESIAN_POINT ( 'NONE',  ( -54.92292740578361077, 1.073804522883522239, 3.225979517392335794 ) ) ;
#19667 = CARTESIAN_POINT ( 'NONE',  ( -36.58413561666647951, -5.110933801299883505, -1.769007076670894740 ) ) ;
#19668 = VERTEX_POINT ( 'NONE', #2215 ) ;
#19669 = DIRECTION ( 'NONE',  ( -1.000000000000000000, -0.000000000000000000, 1.047444401652940007E-14 ) ) ;
#19670 = FILL_AREA_STYLE_COLOUR ( '', #5516 ) ;
#19671 = ADVANCED_FACE ( 'NONE', ( #28831, #18863 ), #11727, .F. ) ;
#19672 = VERTEX_POINT ( 'NONE', #16473 ) ;
#19673 = CARTESIAN_POINT ( 'NONE',  ( -56.94702994616206126, -2.078460969082657872, 3.599999999999789591 ) ) ;
#19674 = CARTESIAN_POINT ( 'NONE',  ( 54.23701917430468455, 5.946187982713466269, -2.050000000000189004 ) ) ;
#19675 = DIRECTION ( 'NONE',  ( 1.000000000000000000, -1.219044193948983948E-29, 3.491481338843133355E-15 ) ) ;
#19676 = CARTESIAN_POINT ( 'NONE',  ( -54.49999477219272848, -1.549165129012789688, 3.331602747802265174 ) ) ;
#19677 = CARTESIAN_POINT ( 'NONE',  ( 69.20000000000003126, 3.252606517456513302E-16, -7.248315259438346108E-13 ) ) ;
#19678 = CARTESIAN_POINT ( 'NONE',  ( 15.03925126672132961, 3.275050215668611653, -2.949461045527567382 ) ) ;
#19679 = AXIS2_PLACEMENT_3D ( 'NONE', #6089, #18283, #30598 ) ;
#19680 = EDGE_CURVE ( 'NONE', #23625, #11505, #4444, .T. ) ;
#19682 = CARTESIAN_POINT ( 'NONE',  ( -36.31440869660544735, 0.05469410396133651819, -5.200000001157072838 ) ) ;
#19681 = CARTESIAN_POINT ( 'NONE',  ( 50.59602332238209499, -0.1408342061598477080, -1.212874140286674507 ) ) ;
#19683 = EDGE_CURVE ( 'NONE', #22989, #18265, #19571, .T. ) ;
#19684 =( BOUNDED_CURVE ( )  B_SPLINE_CURVE ( 3, ( #20903, #18534, #13029, #11383 ),
 .UNSPECIFIED., .F., .T. ) 
 B_SPLINE_CURVE_WITH_KNOTS ( ( 4, 4 ),
 ( 1.982313172862385064, 2.241731514487932397 ),
 .UNSPECIFIED. ) 
 CURVE ( )  GEOMETRIC_REPRESENTATION_ITEM ( )  RATIONAL_B_SPLINE_CURVE ( ( 1.000000000000000000, 0.9943997021150919879, 0.9943997021150919879, 1.000000000000000000 ) ) 
 REPRESENTATION_ITEM ( '' )  );
#19685 = EDGE_CURVE ( 'NONE', #25246, #28315, #21559, .T. ) ;
#19686 = DIRECTION ( 'NONE',  ( 0.000000000000000000, 0.000000000000000000, 1.000000000000000000 ) ) ;
#19687 = CARTESIAN_POINT ( 'NONE',  ( -35.85663232820583346, -5.377732432866661583, 0.5657657256215455899 ) ) ;
#19689 = CARTESIAN_POINT ( 'NONE',  ( -62.09999999999997300, -2.643914563970546805, -0.2822557264641659680 ) ) ;
#19688 = CARTESIAN_POINT ( 'NONE',  ( 15.61552784268242178, 4.977698683490556775, -2.127480166903953585 ) ) ;
#19690 = VERTEX_POINT ( 'NONE', #21256 ) ;
#19691 = LINE ( 'NONE', #14291, #24052 ) ;
#19692 = PLANE ( 'NONE',  #23949 ) ;
#19693 = CIRCLE ( 'NONE', #13594, 2.649999999999999911 ) ;
#19695 = CARTESIAN_POINT ( 'NONE',  ( 52.91818227938544794, 4.100069807933122590, 0.1744202563123046223 ) ) ;
#19694 = CARTESIAN_POINT ( 'NONE',  ( 48.50000000000178346, -1.391941090720833607, 3.849999999997240074 ) ) ;
#19696 = CARTESIAN_POINT ( 'NONE',  ( 47.00000000000002842, -3.933368109459640660, 2.186004417993010485 ) ) ;
#19697 = ORIENTED_EDGE ( 'NONE', *, *, #24833, .F. ) ;
#19698 = DIRECTION ( 'NONE',  ( -1.000000000000000000, -2.586136946169074517E-16, 0.000000000000000000 ) ) ;
#19699 = EDGE_CURVE ( 'NONE', #20276, #19192, #23445, .T. ) ;
#19700 = ORIENTED_EDGE ( 'NONE', *, *, #18494, .F. ) ;
#19701 = DIRECTION ( 'NONE',  ( 1.000000000000000000, -1.219044193948983948E-29, 3.491481338843133355E-15 ) ) ;
#19702 = ORIENTED_EDGE ( 'NONE', *, *, #16141, .T. ) ;
#19703 = ORIENTED_EDGE ( 'NONE', *, *, #9189, .F. ) ;
#19704 = DIRECTION ( 'NONE',  ( 2.581436205204234006E-16, -0.9796124928211140670, -0.2008964009354148872 ) ) ;
#19705 = AXIS2_PLACEMENT_3D ( 'NONE', #26921, #24708, #14880 ) ;
#19706 = EDGE_LOOP ( 'NONE', ( #18282, #2303, #20239, #27558 ) ) ;
#19707 = CARTESIAN_POINT ( 'NONE',  ( 51.82264168681148675, 4.510085190442490344, 0.9145483697865447459 ) ) ;
#19708 = CIRCLE ( 'NONE', #19213, 3.524999999999996358 ) ;
#19709 = CARTESIAN_POINT ( 'NONE',  ( -60.25952994616203284, 3.117691453623994580, -1.800000000000200329 ) ) ;
#19710 = ORIENTED_EDGE ( 'NONE', *, *, #29139, .F. ) ;
#19711 = CARTESIAN_POINT ( 'NONE',  ( -59.59999999999998010, 8.366749974758452890E-15, -2.117042874194827196E-13 ) ) ;
#19712 = CARTESIAN_POINT ( 'NONE',  ( -73.89999999999997726, 0.4598573377555274511, 0.01145551886195783631 ) ) ;
#19713 = EDGE_CURVE ( 'NONE', #15558, #9996, #27135, .T. ) ;
#19714 = CARTESIAN_POINT ( 'NONE',  ( 23.33428888328873185, 6.022557148079767941, 2.050000000000117506 ) ) ;
#19715 = VERTEX_POINT ( 'NONE', #2065 ) ;
#19716 = CARTESIAN_POINT ( 'NONE',  ( 51.79898443072417535, -4.139722501993201575, -1.083525984490930183 ) ) ;
#19717 = EDGE_CURVE ( 'NONE', #1490, #21976, #5202, .T. ) ;
#19718 = CARTESIAN_POINT ( 'NONE',  ( -54.46895629856896903, -1.503487923075246480, 4.032311158269683560 ) ) ;
#19719 = CARTESIAN_POINT ( 'NONE',  ( 58.65263613458539993, -0.9947326234269614487, -1.589467873454827984 ) ) ;
#19720 = DIRECTION ( 'NONE',  ( 0.000000000000000000, 0.000000000000000000, -1.000000000000000000 ) ) ;
#19721 = CARTESIAN_POINT ( 'NONE',  ( 57.01182421275571954, 0.7322894606377696736, 2.432677346698721266 ) ) ;
#19722 =( BOUNDED_SURFACE ( )  B_SPLINE_SURFACE ( 3, 2, ( 
 ( #20382, #24939, #30003 ),
 ( #8320, #15621, #13219 ),
 ( #4350, #1649, #1352 ),
 ( #21172, #28269, #14003 ) ),
 .UNSPECIFIED., .F., .F., .F. ) 
 B_SPLINE_SURFACE_WITH_KNOTS ( ( 4, 4 ),
 ( 3, 3 ),
 ( 0.0002753388251011180433, 0.0003797131536021330217 ),
 ( 0.000000000000000000, 1.000000000000000000 ),
 .UNSPECIFIED. ) 
 GEOMETRIC_REPRESENTATION_ITEM ( )  RATIONAL_B_SPLINE_SURFACE ( (
 ( 1.000000000000000000, 0.8543839308450231762, 1.000000000000000000),
 ( 1.000000000000000000, 0.8547349261747320126, 1.000000000000000000),
 ( 1.000000000000000000, 0.7665921203078746027, 1.000000000000000000),
 ( 1.000000000000000000, 0.7071067811865738850, 1.000000000000000000) ) ) 
 REPRESENTATION_ITEM ( '' )  SURFACE ( )  );
#19723 = CIRCLE ( 'NONE', #5030, 0.09999999999999990841 ) ;
#19724 = CARTESIAN_POINT ( 'NONE',  ( 52.20711756518984004, -0.4999999999994533817, -1.996089927833914146 ) ) ;
#19725 = EDGE_CURVE ( 'NONE', #4123, #27607, #16017, .T. ) ;
#19726 = ADVANCED_FACE ( 'NONE', ( #24688 ), #19484, .T. ) ;
#19727 = PRODUCT_DEFINITION_FORMATION_WITH_SPECIFIED_SOURCE ( 'ANY', '', #22213, .NOT_KNOWN. ) ;
#19728 = CYLINDRICAL_SURFACE ( 'NONE', #14976, 2.625000000000000444 ) ;
#19729 = CARTESIAN_POINT ( 'NONE',  ( 51.75857864376271777, -3.767600426651517953, 1.000000000000000222 ) ) ;
#19730 = VECTOR ( 'NONE', #30375, 1000.000000000000000 ) ;
#19731 = AXIS2_PLACEMENT_3D ( 'NONE', #23604, #4263, #27721 ) ;
#19732 = CARTESIAN_POINT ( 'NONE',  ( 61.24141714606679443, -0.9075239022123753330, -1.727282253937962198 ) ) ;
#19733 = ORIENTED_EDGE ( 'NONE', *, *, #1798, .T. ) ;
#19734 = VECTOR ( 'NONE', #26350, 1000.000000000000000 ) ;
#19735 = ORIENTED_EDGE ( 'NONE', *, *, #6511, .F. ) ;
#19736 = ORIENTED_EDGE ( 'NONE', *, *, #17155, .T. ) ;
#19737 = CARTESIAN_POINT ( 'NONE',  ( -44.49999999999997868, 8.366749974758269874E-15, -1.589829192029513996E-13 ) ) ;
#19738 = CARTESIAN_POINT ( 'NONE',  ( -60.17292740578359656, 1.073804522883521351, 3.225979517392337126 ) ) ;
#19740 = CARTESIAN_POINT ( 'NONE',  ( -36.11780688638206982, 2.199885882962476114, 4.939696253590518005 ) ) ;
#19739 = CARTESIAN_POINT ( 'NONE',  ( -54.81249999999998579, -1.962990915244731793, 3.399999999999796962 ) ) ;
#19741 = ORIENTED_EDGE ( 'NONE', *, *, #21672, .F. ) ;
#19742 = ORIENTED_EDGE ( 'NONE', *, *, #15906, .F. ) ;
#19743 = CARTESIAN_POINT ( 'NONE',  ( 54.00141249824493883, 6.058257955356691760, -1.948923759896386443 ) ) ;
#19744 = ORIENTED_EDGE ( 'NONE', *, *, #15472, .T. ) ;
#19745 = FACE_OUTER_BOUND ( 'NONE', #13921, .T. ) ;
#19746 = EDGE_LOOP ( 'NONE', ( #11118, #20642, #19272, #1293 ) ) ;
#19747 = CARTESIAN_POINT ( 'NONE',  ( 30.67843166873835870, 7.122989987860104399, -2.050000000000106404 ) ) ;
#19748 = ORIENTED_EDGE ( 'NONE', *, *, #9078, .T. ) ;
#19749 = CARTESIAN_POINT ( 'NONE',  ( -54.39999999999997726, -6.102218906431378987E-14, -2.213041600731275921E-13 ) ) ;
#19750 = EDGE_CURVE ( 'NONE', #26613, #29801, #25610, .T. ) ;
#19751 = DIRECTION ( 'NONE',  ( -2.614375865348240525E-16, 0.2008964009354147762, -0.9796124928211140670 ) ) ;
#19752 = ADVANCED_FACE ( 'NONE', ( #5212 ), #21724, .T. ) ;
#19753 = CARTESIAN_POINT ( 'NONE',  ( 15.66436536804540403, -5.008501212420952697, -2.048848402342096087 ) ) ;
#19754 = EDGE_CURVE ( 'NONE', #12035, #22982, #28974, .T. ) ;
#19755 = CARTESIAN_POINT ( 'NONE',  ( -54.95655989232411542, 1.962990915244748891, -3.400000000000186429 ) ) ;
#19756 = CARTESIAN_POINT ( 'NONE',  ( 53.05088594538231916, 4.168914605591084843, -2.050000000000185008 ) ) ;
#19757 = AXIS2_PLACEMENT_3D ( 'NONE', #26025, #9262, #26199 ) ;
#19758 = CARTESIAN_POINT ( 'NONE',  ( 58.75000000000000000, 2.008165151418861427, -0.5380862305899540843 ) ) ;
#19759 = CARTESIAN_POINT ( 'NONE',  ( -35.85663232820580504, -3.779372838781780430, -3.883777296072560947 ) ) ;
#19760 = DIRECTION ( 'NONE',  ( 0.000000000000000000, 0.2008964009354147762, -0.9796124928211139560 ) ) ;
#19761 = ORIENTED_EDGE ( 'NONE', *, *, #3780, .F. ) ;
#19762 = DIRECTION ( 'NONE',  ( 0.000000000000000000, -0.9996898646859344595, -0.02490330187381124827 ) ) ;
#19763 = CARTESIAN_POINT ( 'NONE',  ( -36.77443515226830328, -2.672993279333732541, -4.702725322014769560 ) ) ;
#19764 = CARTESIAN_POINT ( 'NONE',  ( 53.81464057712625504, 5.799094425976108802, -0.8364387603671682436 ) ) ;
#19765 = ORIENTED_EDGE ( 'NONE', *, *, #27270, .T. ) ;
#19766 = CARTESIAN_POINT ( 'NONE',  ( 50.49739899587714831, 0.9326869175216770946, -3.995127421239667687 ) ) ;
#19767 = EDGE_LOOP ( 'NONE', ( #6858, #11879, #26663, #547 ) ) ;
#19768 =( NAMED_UNIT ( * ) PLANE_ANGLE_UNIT ( ) SI_UNIT ( $, .RADIAN. ) );
#19769 = CARTESIAN_POINT ( 'NONE',  ( -36.25997906085252254, -4.878092280899822164, 1.814329181850224071 ) ) ;
#19771 = DIRECTION ( 'NONE',  ( 0.000000000000000000, 0.000000000000000000, 1.000000000000000000 ) ) ;
#19770 = CARTESIAN_POINT ( 'NONE',  ( -58.78335481156722864, 0.7533615035077975142, -3.673546848079180638 ) ) ;
#19772 = ORIENTED_EDGE ( 'NONE', *, *, #26582, .T. ) ;
#19773 = CARTESIAN_POINT ( 'NONE',  ( 69.20000000000001705, 0.7500000000000000000, -1.988246715074083237 ) ) ;
#19774 = AXIS2_PLACEMENT_3D ( 'NONE', #30712, #18691, #3378 ) ;
#19776 = CARTESIAN_POINT ( 'NONE',  ( 33.47623932017462778, -4.683225679163332877, -2.703237727951242508 ) ) ;
#19775 = DIRECTION ( 'NONE',  ( 0.000000000000000000, 0.000000000000000000, -1.000000000000000000 ) ) ;
#19777 = PLANE ( 'NONE',  #5849 ) ;
#19778 = CARTESIAN_POINT ( 'NONE',  ( -60.99999999999996447, -2.489203624310586171, 2.804704140674918023 ) ) ;
#19779 = CARTESIAN_POINT ( 'NONE',  ( 57.01359174706111332, -0.7734660154240907692, 1.735448526467797459 ) ) ;
#19780 = CARTESIAN_POINT ( 'NONE',  ( -55.31249999999997868, 4.108500314926513575, -1.367561758111404790 ) ) ;
#19781 = EDGE_CURVE ( 'NONE', #25278, #27496, #25098, .T. ) ;
#19782 = DIRECTION ( 'NONE',  ( -1.000000000000000000, 1.219044193948983948E-29, -3.491481338843133355E-15 ) ) ;
#19783 = CARTESIAN_POINT ( 'NONE',  ( -67.89999999999997726, 1.599503783497494780, 0.03984528299810137508 ) ) ;
#19784 = EDGE_CURVE ( 'NONE', #16970, #15088, #29375, .T. ) ;
#19785 = DIRECTION ( 'NONE',  ( 0.000000000000000000, 0.2008964009354147762, -0.9796124928211140670 ) ) ;
#19786 = FACE_OUTER_BOUND ( 'NONE', #26810, .T. ) ;
#19787 = ORIENTED_EDGE ( 'NONE', *, *, #7979, .T. ) ;
#19788 = CARTESIAN_POINT ( 'NONE',  ( 15.03925126672125678, -3.779372838781788868, 3.883777296072539187 ) ) ;
#19789 = CYLINDRICAL_SURFACE ( 'NONE', #8381, 0.7500000000000001110 ) ;
#19790 = EDGE_CURVE ( 'NONE', #24431, #4809, #28618, .T. ) ;
#19791 = DIRECTION ( 'NONE',  ( 0.000000000000000000, 0.5454670984325526994, -0.8381322357048270888 ) ) ;
#19792 = CARTESIAN_POINT ( 'NONE',  ( -56.68749999999997158, 3.238593381231837487, 2.874284765127031349 ) ) ;
#19794 = DIRECTION ( 'NONE',  ( 1.000000000000000000, 1.047444401652940007E-14, 0.000000000000000000 ) ) ;
#19793 = CARTESIAN_POINT ( 'NONE',  ( 61.25000000000000000, 2.079005547593442582, 1.004182178118534636E-12 ) ) ;
#19795 = VERTEX_POINT ( 'NONE', #16423 ) ;
#19796 = DIRECTION ( 'NONE',  ( 1.000000000000000000, 1.047444401652940007E-14, 0.000000000000000000 ) ) ;
#19797 = VERTEX_POINT ( 'NONE', #30673 ) ;
#19798 = CARTESIAN_POINT ( 'NONE',  ( 52.06628335902946247, -0.5434431642975682264, -1.794517909405659806 ) ) ;
#19800 = CARTESIAN_POINT ( 'NONE',  ( -73.85208152723558328, -2.420890761855879333E-15, 4.598101673502850081E-15 ) ) ;
#19799 = DIRECTION ( 'NONE',  ( -1.000000000000000000, -1.047444401652940007E-14, -0.000000000000000000 ) ) ;
#19801 = DIRECTION ( 'NONE',  ( 1.000000000000000000, 3.053848253006669023E-16, -2.042510438544995415E-16 ) ) ;
#19802 = VERTEX_POINT ( 'NONE', #16902 ) ;
#19803 = ORIENTED_EDGE ( 'NONE', *, *, #45, .F. ) ;
#19804 = CIRCLE ( 'NONE', #27366, 0.1000000000000002554 ) ;
#19805 = CARTESIAN_POINT ( 'NONE',  ( 51.23017468167498123, -0.9889849352709336738, -1.419511492616531978 ) ) ;
#19806 = AXIS2_PLACEMENT_3D ( 'NONE', #25919, #11051, #6001 ) ;
#19807 = CARTESIAN_POINT ( 'NONE',  ( 51.50435016707358926, 0.9265794315412906323, 1.339215852266870010 ) ) ;
#19808 = ORIENTED_EDGE ( 'NONE', *, *, #26186, .T. ) ;
#19809 = DIRECTION ( 'NONE',  ( 0.000000000000000000, -1.000000000000000000, -3.491481338843133355E-15 ) ) ;
#19810 = CARTESIAN_POINT ( 'NONE',  ( -59.19495429951913223, 2.548385458854359964, -0.9469503383365888149 ) ) ;
#19811 = CARTESIAN_POINT ( 'NONE',  ( -59.64490075983744788, -2.179131191433543169, 1.525521932368567590 ) ) ;
#19812 = ORIENTED_EDGE ( 'NONE', *, *, #19405, .F. ) ;
#19813 = APPLICATION_PROTOCOL_DEFINITION ( 'draft international standard', 'automotive_design', 1998, #15616 ) ;
#19814 = ADVANCED_FACE ( 'NONE', ( #23725 ), #30986, .T. ) ;
#19815 = CARTESIAN_POINT ( 'NONE',  ( -59.29999999999996163, -3.390200327460917595, 0.9814680162012726639 ) ) ;
#19816 =( LENGTH_UNIT ( ) NAMED_UNIT ( * ) SI_UNIT ( .MILLI., .METRE. ) );
#19817 = ORIENTED_EDGE ( 'NONE', *, *, #3255, .F. ) ;
#19818 = CARTESIAN_POINT ( 'NONE',  ( -58.88452994616202574, 2.093608279459372350E-14, -3.600000000000208811 ) ) ;
#19819 = CARTESIAN_POINT ( 'NONE',  ( 51.74540690333466841, 3.818766532315405193, -2.050000000000175682 ) ) ;
#19820 = CARTESIAN_POINT ( 'NONE',  ( 48.50000000000002132, -1.409901620910170461, -3.850000000000021849 ) ) ;
#19821 = DIRECTION ( 'NONE',  ( 0.000000000000000000, 0.000000000000000000, -1.000000000000000000 ) ) ;
#19822 = CARTESIAN_POINT ( 'NONE',  ( 51.90000000000001279, -4.227689052994015206, -1.125730994152047693 ) ) ;
#19823 = CIRCLE ( 'NONE', #30424, 2.674999999999998934 ) ;
#19824 = CARTESIAN_POINT ( 'NONE',  ( -56.83155989232414385, -1.962990915244743562, 3.399999999999782752 ) ) ;
#19825 = VECTOR ( 'NONE', #23688, 1000.000000000000000 ) ;
#19827 = EDGE_CURVE ( 'NONE', #23968, #13230, #2511, .T. ) ;
#19826 = B_SPLINE_CURVE_WITH_KNOTS ( 'NONE', 3,
 ( #6713, #16376, #25721, #15320, #10581, #20257 ),
 .UNSPECIFIED., .F., .F.,
 ( 4, 2, 4 ),
 ( 0.000000000000000000, 0.4999999999999995559, 1.000000000000000000 ),
 .UNSPECIFIED. ) ;
#19829 = CARTESIAN_POINT ( 'NONE',  ( -35.85663232820580504, -0.7747498368337907282, -5.363501452440941009 ) ) ;
#19828 = DIRECTION ( 'NONE',  ( 1.000000000000000000, 1.047444401652940007E-14, 0.000000000000000000 ) ) ;
#19830 = CARTESIAN_POINT ( 'NONE',  ( -62.08976859767152234, -2.518353679445345605, 0.1831464729044566531 ) ) ;
#19831 = DIRECTION ( 'NONE',  ( 1.009293658750142281E-14, 0.000000000000000000, 1.000000000000000000 ) ) ;
#19832 = LINE ( 'NONE', #29620, #8396 ) ;
#19833 = EDGE_LOOP ( 'NONE', ( #18613, #3202, #23973, #18677, #17742, #24656 ) ) ;
#19834 = LINE ( 'NONE', #3354, #17974 ) ;
#19835 = CARTESIAN_POINT ( 'NONE',  ( 51.74175063877302705, 3.850631602819848620, 1.433098087438243295 ) ) ;
#19837 = CARTESIAN_POINT ( 'NONE',  ( 52.29551448703413996, 3.895969970751527178, -1.277875341319584246 ) ) ;
#19836 = CYLINDRICAL_SURFACE ( 'NONE', #13969, 0.2500000000000002220 ) ;
#19838 = CARTESIAN_POINT ( 'NONE',  ( 57.00873807961998097, 0.7491996424029042645, 2.489992076190610248 ) ) ;
#19839 = VERTEX_POINT ( 'NONE', #23875 ) ;
#19840 = CARTESIAN_POINT ( 'NONE',  ( -61.39959699979583263, -2.652859410556386521, 0.5023315908532165475 ) ) ;
#19841 = VERTEX_POINT ( 'NONE', #4852 ) ;
#19842 = CARTESIAN_POINT ( 'NONE',  ( 58.75000000000002132, 6.153735859711025284E-13, 3.111507638930570854E-58 ) ) ;
#19843 = ORIENTED_EDGE ( 'NONE', *, *, #9451, .T. ) ;
#19844 = VERTEX_POINT ( 'NONE', #31302 ) ;
#19845 = CARTESIAN_POINT ( 'NONE',  ( 16.08093158123428523, 5.226279933021939605, -1.394410282272748880 ) ) ;
#19846 = ORIENTED_EDGE ( 'NONE', *, *, #19294, .F. ) ;
#19847 = B_SPLINE_CURVE_WITH_KNOTS ( 'NONE', 3,
 ( #13770, #18722, #28208, #11415, #16009, #25825, #25672, #1924, #21413, #9365, #11587, #30742, #30899, #25977 ),
 .UNSPECIFIED., .F., .F.,
 ( 4, 2, 2, 2, 2, 2, 4 ),
 ( 0.000000000000000000, 0.0003953907277084696219, 0.0005930860915627040805, 0.0006919337734898216080, 0.0007413576144533806428, 0.0007660695349351557149, 0.0007907814554169307871 ),
 .UNSPECIFIED. ) ;
#19848 = CARTESIAN_POINT ( 'NONE',  ( 46.90000000000001279, -4.227689052994015206, 1.125730994152046582 ) ) ;
#19849 = ADVANCED_FACE ( 'NONE', ( #26397 ), #14519, .F. ) ;
#19850 = CARTESIAN_POINT ( 'NONE',  ( -59.19702994616205416, -2.078460969082657872, 3.599999999999782041 ) ) ;
#19851 = ORIENTED_EDGE ( 'NONE', *, *, #21686, .F. ) ;
#19852 = CARTESIAN_POINT ( 'NONE',  ( 54.47883572522132312, -0.001215825626424074960, 4.337530305537235620 ) ) ;
#19853 = EDGE_LOOP ( 'NONE', ( #1673, #25899, #28436, #16888 ) ) ;
#19854 = CARTESIAN_POINT ( 'NONE',  ( -44.59999999999996589, 1.600000000000021627, -3.363870538531645416 ) ) ;
#19855 = EDGE_CURVE ( 'NONE', #30058, #27746, #6614, .T. ) ;
#19856 = PLANE ( 'NONE',  #14377 ) ;
#19857 = ORIENTED_EDGE ( 'NONE', *, *, #27876, .T. ) ;
#19858 = CARTESIAN_POINT ( 'NONE',  ( 51.77013903953137230, -4.166824046520646974, -1.027859347733066420 ) ) ;
#19859 =( BOUNDED_CURVE ( )  B_SPLINE_CURVE ( 3, ( #24777, #3086, #8002, #17665 ),
 .UNSPECIFIED., .F., .T. ) 
 B_SPLINE_CURVE_WITH_KNOTS ( ( 4, 4 ),
 ( 1.164632096430649133, 1.274397363402604677 ),
 .UNSPECIFIED. ) 
 CURVE ( )  GEOMETRIC_REPRESENTATION_ITEM ( )  RATIONAL_B_SPLINE_CURVE ( ( 1.000000000000000000, 0.9989962175098910935, 0.9989962175098910935, 1.000000000000000000 ) ) 
 REPRESENTATION_ITEM ( '' )  );
#19860 = CYLINDRICAL_SURFACE ( 'NONE', #14441, 0.2500000000000000000 ) ;
#19861 = DIRECTION ( 'NONE',  ( -1.000000000000000000, -0.000000000000000000, -0.000000000000000000 ) ) ;
#19862 = AXIS2_PLACEMENT_3D ( 'NONE', #12311, #17245, #7262 ) ;
#19863 = FACE_OUTER_BOUND ( 'NONE', #17657, .T. ) ;
#19864 = CARTESIAN_POINT ( 'NONE',  ( 57.03008957414009217, 0.7461961634598838211, 2.423767181580114727 ) ) ;
#19865 = EDGE_CURVE ( 'NONE', #21345, #3064, #28666, .T. ) ;
#19867 = DIRECTION ( 'NONE',  ( -1.000000000000000000, 0.000000000000000000, 1.047444401652940007E-14 ) ) ;
#19866 = DIRECTION ( 'NONE',  ( 1.047444401652940007E-14, 0.000000000000000000, 1.000000000000000000 ) ) ;
#19868 = CARTESIAN_POINT ( 'NONE',  ( -61.34999999999997300, -2.435425537339440449, 0.6665789166144534539 ) ) ;
#19869 = LINE ( 'NONE', #17040, #1322 ) ;
#19870 = CARTESIAN_POINT ( 'NONE',  ( -54.49999477219272848, 1.549165129012789466, -3.331602747802265174 ) ) ;
#19871 = CARTESIAN_POINT ( 'NONE',  ( -59.19999999999997442, 4.156921938165309527, 1.250136525132554910 ) ) ;
#19872 = ORIENTED_EDGE ( 'NONE', *, *, #1533, .T. ) ;
#19873 = EDGE_CURVE ( 'NONE', #18790, #11223, #11829, .T. ) ;
#19874 = ORIENTED_EDGE ( 'NONE', *, *, #23282, .T. ) ;
#19875 = ORIENTED_EDGE ( 'NONE', *, *, #26237, .T. ) ;
#19876 = CARTESIAN_POINT ( 'NONE',  ( 60.75000000000002842, -0.4999999999993638977, -1.863080903343643069 ) ) ;
#19877 = CIRCLE ( 'NONE', #4699, 2.000000000000000000 ) ;
#19878 = CARTESIAN_POINT ( 'NONE',  ( -59.79792740578359656, -1.073804522883517576, -3.225979517392334905 ) ) ;
#19880 = CARTESIAN_POINT ( 'NONE',  ( 51.31572262954152563, 1.002608958138273554, -1.584424273060082378 ) ) ;
#19879 = CARTESIAN_POINT ( 'NONE',  ( 15.71019289815286513, 4.797343084509189559, 2.497389432264014886 ) ) ;
#19881 = ORIENTED_EDGE ( 'NONE', *, *, #12606, .T. ) ;
#19882 = ORIENTED_EDGE ( 'NONE', *, *, #25639, .F. ) ;
#19883 = CARTESIAN_POINT ( 'NONE',  ( 51.35579717334661609, -4.328226263800980078, -1.560066312055160775 ) ) ;
#19884 = VERTEX_POINT ( 'NONE', #31142 ) ;
#19885 = CARTESIAN_POINT ( 'NONE',  ( -63.86464466094066239, 6.291209007590390943E-16, 2.558157268131197822E-15 ) ) ;
#19886 = EDGE_CURVE ( 'NONE', #8533, #7645, #30157, .T. ) ;
#19887 = EDGE_LOOP ( 'NONE', ( #6362, #30351, #15857, #8877 ) ) ;
#19888 = CARTESIAN_POINT ( 'NONE',  ( 34.56269065792915995, 8.313757757582562746, -2.050000000000119726 ) ) ;
#19889 = EDGE_CURVE ( 'NONE', #11624, #13819, #13967, .T. ) ;
#19890 = ORIENTED_EDGE ( 'NONE', *, *, #22832, .F. ) ;
#19891 = DIRECTION ( 'NONE',  ( 0.000000000000000000, 0.000000000000000000, 1.000000000000000000 ) ) ;
#19892 = EDGE_CURVE ( 'NONE', #5273, #13582, #4481, .T. ) ;
#19893 = CARTESIAN_POINT ( 'NONE',  ( 54.34016439512040364, 6.711820450561372553, 2.049999999999808420 ) ) ;
#19894 = ORIENTED_EDGE ( 'NONE', *, *, #6848, .F. ) ;
#19895 = CARTESIAN_POINT ( 'NONE',  ( 58.65000000000001990, 6.143261415694495821E-13, 3.111507638930570854E-58 ) ) ;
#19896 = CARTESIAN_POINT ( 'NONE',  ( -58.39405989232412963, -3.920666489018312013E-15, 3.399999999999791633 ) ) ;
#19897 = CARTESIAN_POINT ( 'NONE',  ( 53.82285890661302119, 4.901445667019300068, -2.050000000000187672 ) ) ;
#19898 = CARTESIAN_POINT ( 'NONE',  ( 48.00000000000001421, -3.908336260473454615, -1.238913909466087926 ) ) ;
#19899 = CARTESIAN_POINT ( 'NONE',  ( 48.30268969835653081, 0.9327905306641951499, -3.995066436131523346 ) ) ;
#19900 = FACE_OUTER_BOUND ( 'NONE', #27383, .T. ) ;
#19901 = DIRECTION ( 'NONE',  ( -1.000000000000000000, -1.047444401652940007E-14, -0.000000000000000000 ) ) ;
#19902 = VECTOR ( 'NONE', #467, 1000.000000000000000 ) ;
#19903 = VECTOR ( 'NONE', #6814, 1000.000000000000000 ) ;
#19904 = CARTESIAN_POINT ( 'NONE',  ( 58.75000000000000711, 1.470078920828144620, -1.470078920826818125 ) ) ;
#19905 = CARTESIAN_POINT ( 'NONE',  ( -59.33448904220819742, 2.516908228110276369, -1.027510759589427058 ) ) ;
#19906 = CARTESIAN_POINT ( 'NONE',  ( 51.31802667458096323, -1.005866567096536546, 1.281163073955422504 ) ) ;
#19907 = ORIENTED_EDGE ( 'NONE', *, *, #23961, .F. ) ;
#19908 = EDGE_CURVE ( 'NONE', #26840, #29149, #3553, .T. ) ;
#19909 = CARTESIAN_POINT ( 'NONE',  ( -61.34999999999997300, -2.580661732147724319, -0.5877664123773247429 ) ) ;
#19910 = DIRECTION ( 'NONE',  ( 0.000000000000000000, -0.000000000000000000, -1.000000000000000000 ) ) ;
#19911 = CARTESIAN_POINT ( 'NONE',  ( 54.28867365409859502, 5.640057820322912363, -1.625000000000180744 ) ) ;
#19912 = ORIENTED_EDGE ( 'NONE', *, *, #2468, .F. ) ;
#19913 = DIRECTION ( 'NONE',  ( 0.000000000000000000, 1.000000000000000000, 0.000000000000000000 ) ) ;
#19914 = ORIENTED_EDGE ( 'NONE', *, *, #11732, .T. ) ;
#19915 =( REPRESENTATION_RELATIONSHIP ('NONE','NONE', #7047, #29923 ) REPRESENTATION_RELATIONSHIP_WITH_TRANSFORMATION ( #8543 )SHAPE_REPRESENTATION_RELATIONSHIP( ) );
#19916 = EDGE_CURVE ( 'NONE', #3969, #9980, #7927, .T. ) ;
#19917 = CARTESIAN_POINT ( 'NONE',  ( 53.34494210428218963, 4.987020249080358347, 1.614082030464476292 ) ) ;
#19918 = DIRECTION ( 'NONE',  ( 1.000000000000000000, 3.125586771759065906E-16, 0.000000000000000000 ) ) ;
#19920 = DIRECTION ( 'NONE',  ( -3.489354422748178188E-15, 1.218509414717996091E-16, -1.000000000000000000 ) ) ;
#19919 = CARTESIAN_POINT ( 'NONE',  ( 48.39253357792949117, -1.341874354110733858, -3.874311046529112623 ) ) ;
#19921 = ORIENTED_EDGE ( 'NONE', *, *, #16715, .T. ) ;
#19922 = CARTESIAN_POINT ( 'NONE',  ( 61.25000000000003553, -0.8666666666660259866, -1.374595900215366040 ) ) ;
#19923 = CARTESIAN_POINT ( 'NONE',  ( 48.30000000000001847, -0.6304760106459033064, 3.950000000000021938 ) ) ;
#19924 = ORIENTED_EDGE ( 'NONE', *, *, #7359, .T. ) ;
#19926 = CARTESIAN_POINT ( 'NONE',  ( -60.59999999999998010, -2.414926673651788924, -1.060468536699751940 ) ) ;
#19925 = DIRECTION ( 'NONE',  ( 8.450433050631136626E-15, -0.6683962987616075546, -0.7438053426816615410 ) ) ;
#19927 = ORIENTED_EDGE ( 'NONE', *, *, #19886, .T. ) ;
#19928 = CARTESIAN_POINT ( 'NONE',  ( -60.43749999999996447, 3.238593381231845481, 2.874284765127022023 ) ) ;
#19929 = AXIS2_PLACEMENT_3D ( 'NONE', #23627, #21104, #4454 ) ;
#19930 = CARTESIAN_POINT ( 'NONE',  ( 57.04071222441830713, -0.7791709056946051204, 1.732885792771923672 ) ) ;
#19931 = EDGE_CURVE ( 'NONE', #26160, #19416, #12763, .T. ) ;
#19932 = CARTESIAN_POINT ( 'NONE',  ( 58.65263613458534309, 1.589467873455502778, -0.9947326234274815882 ) ) ;
#19933 = CARTESIAN_POINT ( 'NONE',  ( -54.72099364905386665, -0.2309624077929028074, -3.875409454552789956 ) ) ;
#19934 = CARTESIAN_POINT ( 'NONE',  ( 58.65000000000001990, 6.143261415694495821E-13, 3.111507638930570854E-58 ) ) ;
#19935 = LINE ( 'NONE', #12317, #22479 ) ;
#19936 = FACE_OUTER_BOUND ( 'NONE', #24462, .T. ) ;
#19937 = ORIENTED_EDGE ( 'NONE', *, *, #19645, .T. ) ;
#19938 = CARTESIAN_POINT ( 'NONE',  ( 15.74652664997094931, 3.345968172200292745, 4.250076229745635814 ) ) ;
#19939 = CARTESIAN_POINT ( 'NONE',  ( -60.60558231549867969, -2.497277651495709794, 0.9543206905132385343 ) ) ;
#19940 = CARTESIAN_POINT ( 'NONE',  ( -58.58155989232410832, 3.400000000000007905, -1.908076882137507950E-13 ) ) ;
#19941 = CIRCLE ( 'NONE', #18941, 2.624999999999998668 ) ;
#19942 = EDGE_CURVE ( 'NONE', #7645, #9785, #30291, .T. ) ;
#19943 = CARTESIAN_POINT ( 'NONE',  ( -56.63452994616203284, 2.358131988075197809E-14, -3.600000000000201261 ) ) ;
#19944 = CARTESIAN_POINT ( 'NONE',  ( 58.75000000000001421, 0.4991218602018681061, 1.863314270026655395 ) ) ;
#19945 = EDGE_CURVE ( 'NONE', #5179, #21368, #29831, .T. ) ;
#19946 = ORIENTED_EDGE ( 'NONE', *, *, #21694, .T. ) ;
#19947 = EDGE_LOOP ( 'NONE', ( #8377, #17925, #19381, #28300 ) ) ;
#19948 = UNCERTAINTY_MEASURE_WITH_UNIT (LENGTH_MEASURE( 1.000000000000000082E-05 ), #5741, 'distance_accuracy_value', 'NONE');
#19949 = ADVANCED_FACE ( 'NONE', ( #20503 ), #30663, .F. ) ;
#19950 = CARTESIAN_POINT ( 'NONE',  ( -77.29999999999998295, -3.473832742311974792E-15, 5.302342620690189014E-15 ) ) ;
#19951 = AXIS2_PLACEMENT_3D ( 'NONE', #12477, #24508, #22166 ) ;
#19953 = CARTESIAN_POINT ( 'NONE',  ( 33.47623932017462778, 1.734723475976807489E-15, 0.000000000000000000 ) ) ;
#19952 = CARTESIAN_POINT ( 'NONE',  ( 15.48686146417451148, -3.146183597690412448, -4.141717300434339499 ) ) ;
#19954 = ORIENTED_EDGE ( 'NONE', *, *, #7271, .T. ) ;
#19955 = VERTEX_POINT ( 'NONE', #15107 ) ;
#19956 = CARTESIAN_POINT ( 'NONE',  ( 51.25000000000002842, -0.9938153758920951208, 1.589954715908409977 ) ) ;
#19957 = CARTESIAN_POINT ( 'NONE',  ( 47.02510416483082167, -3.758927087870047146, 1.866445954014450903 ) ) ;
#19958 = ORIENTED_EDGE ( 'NONE', *, *, #17370, .F. ) ;
#19960 = CARTESIAN_POINT ( 'NONE',  ( -59.19999999999997442, 2.435569474727625305, 1.250136525132548693 ) ) ;
#19959 = CARTESIAN_POINT ( 'NONE',  ( -56.25952994616206126, -4.643455692769913008E-15, 3.599999999999798916 ) ) ;
#19961 = CARTESIAN_POINT ( 'NONE',  ( -54.39999999999996305, 1.557046979865791769, -3.273565289175131010 ) ) ;
#19962 = CIRCLE ( 'NONE', #24999, 0.4576450603546982632 ) ;
#19963 = DIRECTION ( 'NONE',  ( 2.459562394685749209E-16, -0.9510565162951544194, 0.3090169943749447312 ) ) ;
#19964 = EDGE_CURVE ( 'NONE', #3318, #31001, #28083, .T. ) ;
#19965 = CARTESIAN_POINT ( 'NONE',  ( 58.75000018595672913, -1.404395290251533313, -1.333791840693540731 ) ) ;
#19966 = CIRCLE ( 'NONE', #15413, 0.2500000000000002776 ) ;
#19967 = ORIENTED_EDGE ( 'NONE', *, *, #14341, .F. ) ;
#19968 = CARTESIAN_POINT ( 'NONE',  ( -56.57202994616203995, 2.078460969082674747, -3.600000000000191935 ) ) ;
#19969 = VECTOR ( 'NONE', #25677, 999.9999999999998863 ) ;
#19970 = CARTESIAN_POINT ( 'NONE',  ( 51.75611399313549299, 4.330462468343535321, -2.050000000000496758 ) ) ;
#19971 = PLANE ( 'NONE',  #15669 ) ;
#19972 = CARTESIAN_POINT ( 'NONE',  ( 15.49702763512084047, 0.05469410396135616914, 5.200000001156997342 ) ) ;
#19973 = CARTESIAN_POINT ( 'NONE',  ( 51.30607925897589183, -3.992076856964202669, 1.294425493480717115 ) ) ;
#19974 = FACE_OUTER_BOUND ( 'NONE', #7505, .T. ) ;
#19976 = CARTESIAN_POINT ( 'NONE',  ( -36.30347965937283305, -0.1138661108242699921, -5.199999999057708600 ) ) ;
#19975 = CARTESIAN_POINT ( 'NONE',  ( 31.35411506832756601, 7.935106539446550755, -1.425000000000109068 ) ) ;
#19977 = TOROIDAL_SURFACE ( 'NONE', #3270, 3.950000000000000178, 0.05000000000000000278 ) ;
#19978 = CARTESIAN_POINT ( 'NONE',  ( 51.25000000000001421, 0.9938153758931693726, -1.589954715908409755 ) ) ;
#19979 = CARTESIAN_POINT ( 'NONE',  ( 48.41845806530710661, 1.153441674035750708, -3.890342980189691158 ) ) ;
#19981 = CARTESIAN_POINT ( 'NONE',  ( 57.00000000000001421, -0.6999999999999999556, 2.452039967047845437 ) ) ;
#19980 = CARTESIAN_POINT ( 'NONE',  ( 15.48686146417449194, 4.911231426340504136, -1.712337380313421198 ) ) ;
#19982 = EDGE_CURVE ( 'NONE', #24785, #30539, #7994, .T. ) ;
#19983 = ORIENTED_EDGE ( 'NONE', *, *, #18277, .T. ) ;
#19984 = CARTESIAN_POINT ( 'NONE',  ( 58.64999999999999858, 1.834410884276644227, -0.3880228184651523526 ) ) ;
#19985 = DIRECTION ( 'NONE',  ( 3.696862594069216125E-15, 0.9356455129756975353, 0.3529411764705897570 ) ) ;
#19987 = PLANE ( 'NONE',  #5535 ) ;
#19986 = DIRECTION ( 'NONE',  ( 0.000000000000000000, 0.000000000000000000, -1.000000000000000000 ) ) ;
#19988 = CARTESIAN_POINT ( 'NONE',  ( 47.38244758155640568, -4.256411467774985802, 1.449592950257672985 ) ) ;
#19989 = ORIENTED_EDGE ( 'NONE', *, *, #10190, .F. ) ;
#19990 = FACE_OUTER_BOUND ( 'NONE', #16773, .T. ) ;
#19991 = CARTESIAN_POINT ( 'NONE',  ( 27.27214205000342062, 5.011961650406415281, -1.550000000000094857 ) ) ;
#19992 = ORIENTED_EDGE ( 'NONE', *, *, #13652, .T. ) ;
#19993 = VECTOR ( 'NONE', #22786, 1000.000000000000000 ) ;
#19994 = DIRECTION ( 'NONE',  ( 0.000000000000000000, 0.000000000000000000, -1.000000000000000000 ) ) ;
#19996 = ORIENTED_EDGE ( 'NONE', *, *, #2713, .T. ) ;
#19995 = B_SPLINE_CURVE_WITH_KNOTS ( 'NONE', 3,
 ( #25417, #23218, #16242, #27805, #11167, #3720 ),
 .UNSPECIFIED., .F., .F.,
 ( 4, 2, 4 ),
 ( 2.716379216518720479E-07, 0.0002832190672503200860, 0.0005661664965789883243 ),
 .UNSPECIFIED. ) ;
#19997 = ORIENTED_EDGE ( 'NONE', *, *, #11276, .T. ) ;
#19998 = CARTESIAN_POINT ( 'NONE',  ( 15.29449157529475301, 5.068523420888873865, 1.228242390833590658 ) ) ;
#19999 = ORIENTED_EDGE ( 'NONE', *, *, #18931, .F. ) ;
#20000 = PRESENTATION_STYLE_ASSIGNMENT (( #15565 ) ) ;
#20001 = CARTESIAN_POINT ( 'NONE',  ( 29.14728015088713420, 5.974878709855460102, 1.949999999999897815 ) ) ;
#20002 = EDGE_CURVE ( 'NONE', #7829, #15664, #22992, .T. ) ;
#20003 = CARTESIAN_POINT ( 'NONE',  ( -60.88452994616204705, 3.117691453623979481, 1.799999999999795985 ) ) ;
#20004 = ORIENTED_EDGE ( 'NONE', *, *, #29405, .T. ) ;
#20005 = CARTESIAN_POINT ( 'NONE',  ( -56.18749999999997868, -3.399999999999991029, -2.152687225432237971E-13 ) ) ;
#20006 = VERTEX_POINT ( 'NONE', #25066 ) ;
#20007 = CARTESIAN_POINT ( 'NONE',  ( 51.80000000000001137, 3.987918699320235572, -2.032049940491799322 ) ) ;
#20008 = AXIS2_PLACEMENT_3D ( 'NONE', #16201, #23475, #11443 ) ;
#20009 = CARTESIAN_POINT ( 'NONE',  ( 26.92903764425156510, 5.249711979699990927, 2.050000000000040679 ) ) ;
#20010 = ORIENTED_EDGE ( 'NONE', *, *, #19855, .F. ) ;
#20011 = AXIS2_PLACEMENT_3D ( 'NONE', #12233, #53, #196 ) ;
#20012 = CARTESIAN_POINT ( 'NONE',  ( 36.50000000000002132, 0.000000000000000000, 0.000000000000000000 ) ) ;
#20013 = CARTESIAN_POINT ( 'NONE',  ( 54.24037840390754184, 6.535103219670295616, -2.050000000000189004 ) ) ;
#20014 = DIRECTION ( 'NONE',  ( -1.983166172879301074E-16, 0.9119702176296790030, -0.4102564102564101312 ) ) ;
#20015 = CARTESIAN_POINT ( 'NONE',  ( -35.85663232820584057, -3.275050215668596998, 2.949461045527599801 ) ) ;
#20016 = TOROIDAL_SURFACE ( 'NONE', #8947, 0.4399999999999999467, 0.01000000000000000021 ) ;
#20017 = EDGE_CURVE ( 'NONE', #5117, #15357, #13395, .T. ) ;
#20018 = CARTESIAN_POINT ( 'NONE',  ( 57.02405634237670284, -0.7430569499193692140, 2.425812863566016997 ) ) ;
#20019 = CIRCLE ( 'NONE', #12917, 0.1000000000000028644 ) ;
#20020 = VECTOR ( 'NONE', #30202, 1000.000000000000000 ) ;
#20022 = DIRECTION ( 'NONE',  ( 1.000000000000000000, 0.000000000000000000, 0.000000000000000000 ) ) ;
#20021 = CARTESIAN_POINT ( 'NONE',  ( -57.22085481156723574, 2.489203624310592389, -2.804704140674919355 ) ) ;
#20023 = DIRECTION ( 'NONE',  ( 0.000000000000000000, -1.000000000000000000, -4.336808689942015369E-15 ) ) ;
#20024 = FACE_OUTER_BOUND ( 'NONE', #19351, .T. ) ;
#20025 = EDGE_CURVE ( 'NONE', #19387, #13619, #9883, .T. ) ;
#20026 = CARTESIAN_POINT ( 'NONE',  ( -54.47366401599046526, 1.505709097230404359, -3.303769268891089794 ) ) ;
#20027 = DIRECTION ( 'NONE',  ( -1.000000000000000000, -3.054025858079668409E-16, 2.042474015755241579E-16 ) ) ;
#20028 = EDGE_CURVE ( 'NONE', #29149, #30150, #24116, .T. ) ;
#20029 = EDGE_LOOP ( 'NONE', ( #4460, #23628, #27655, #5996 ) ) ;
#20030 = CARTESIAN_POINT ( 'NONE',  ( -54.49999999999997868, 1.549999999999999600, 3.332135201338624952 ) ) ;
#20031 = CIRCLE ( 'NONE', #30109, 2.750000000000000000 ) ;
#20032 = B_SPLINE_CURVE_WITH_KNOTS ( 'NONE', 3,
 ( #5339, #290, #19930, #2985, #9959, #19779, #29415, #24672, #17868, #754, #19634, #15321, #10582, #20258, #10260, #598 ),
 .UNSPECIFIED., .F., .F.,
 ( 4, 3, 3, 3, 3, 4 ),
 ( 0.000000000000000000, 1.391268354954338704E-05, 4.880039988305115829E-05, 8.637315450940535953E-05, 0.0001246458323646918982, 0.0001626605312951481396 ),
 .UNSPECIFIED. ) ;
#20033 = AXIS2_PLACEMENT_3D ( 'NONE', #1907, #30723, #21397 ) ;
#20034 = ORIENTED_EDGE ( 'NONE', *, *, #19627, .F. ) ;
#20035 = ORIENTED_EDGE ( 'NONE', *, *, #10892, .F. ) ;
#20036 = CARTESIAN_POINT ( 'NONE',  ( -59.18207606663301590, 2.383656014762451036, 1.250136525132548693 ) ) ;
#20037 = CARTESIAN_POINT ( 'NONE',  ( -57.17292740578359656, 1.073804522883521795, 3.225979517392336682 ) ) ;
#20039 = CARTESIAN_POINT ( 'NONE',  ( -59.42527672090727009, 2.245369935805367589, 1.420690871442056080 ) ) ;
#20038 = CARTESIAN_POINT ( 'NONE',  ( 15.32766723174652768, 4.698774973472825245, 2.676767126782138462 ) ) ;
#20040 = ORIENTED_EDGE ( 'NONE', *, *, #4106, .T. ) ;
#20041 = AXIS2_PLACEMENT_3D ( 'NONE', #24026, #19442, #31307 ) ;
#20042 = ORIENTED_EDGE ( 'NONE', *, *, #20443, .F. ) ;
#20043 = CARTESIAN_POINT ( 'NONE',  ( 54.19008868793212486, 6.697828837789025158, -2.050000000000189004 ) ) ;
#20044 = EDGE_LOOP ( 'NONE', ( #16575, #30421, #9181, #31019, #30864, #19363, #18652, #26700, #21004 ) ) ;
#20045 = AXIS2_PLACEMENT_3D ( 'NONE', #10517, #8440, #20490 ) ;
#20046 = B_SPLINE_CURVE_WITH_KNOTS ( 'NONE', 3,
 ( #14442, #12531, #19527, #27091, #29012, #2582, #14898, #15068, #24724, #2881, #3036, #12086, #12681, #22361, #21762, #7490, #50, #9713, #19373 ),
 .UNSPECIFIED., .F., .F.,
 ( 4, 3, 3, 3, 3, 3, 4 ),
 ( -7.770771407263729990E-06, 0.000000000000000000, 1.441088071712340062E-05, 4.839392028739892171E-05, 8.235972512776415120E-05, 0.0001163176750529216742, 0.0001502761185964958737 ),
 .UNSPECIFIED. ) ;
#20048 = DIRECTION ( 'NONE',  ( 3.491481338843133750E-15, 0.000000000000000000, 1.000000000000000000 ) ) ;
#20047 = VECTOR ( 'NONE', #29286, 1000.000000000000000 ) ;
#20049 = EDGE_CURVE ( 'NONE', #31043, #16826, #31115, .T. ) ;
#20050 = ORIENTED_EDGE ( 'NONE', *, *, #4817, .F. ) ;
#20051 = CARTESIAN_POINT ( 'NONE',  ( 30.23587923126627786, 6.713699170113216930, -2.050000000000235190 ) ) ;
#20052 = AXIS2_PLACEMENT_3D ( 'NONE', #12260, #4822, #26688 ) ;
#20053 =( BOUNDED_SURFACE ( )  B_SPLINE_SURFACE ( 3, 2, ( 
 ( #5276, #14929, #19402 ),
 ( #12256, #7205, #24301 ),
 ( #12401, #21941, #19719 ),
 ( #17183, #385, #14783 ),
 ( #16719, #11952, #16869 ),
 ( #7056, #26967, #21637 ),
 ( #9741, #31271, #7521 ),
 ( #2754, #29044, #9596 ),
 ( #11792, #19256, #4663 ),
 ( #2130, #17323, #9428 ) ),
 .UNSPECIFIED., .F., .F., .F. ) 
 B_SPLINE_SURFACE_WITH_KNOTS ( ( 4, 2, 2, 2, 4 ),
 ( 3, 3 ),
 ( 0.0001706658715697745971, 0.0002229276920781411762, 0.0002751895125865077554, 0.0003274513330948743074, 0.0003797131536032408595 ),
 ( 0.000000000000000000, 1.000000000000000000 ),
 .UNSPECIFIED. ) 
 GEOMETRIC_REPRESENTATION_ITEM ( )  RATIONAL_B_SPLINE_SURFACE ( (
 ( 1.000000000000000000, 0.7071067811873460451, 1.000000000000000000),
 ( 1.000000000000000000, 0.7375607040709752926, 1.000000000000000000),
 ( 1.000000000000000000, 0.7730431127433748939, 1.000000000000000000),
 ( 1.000000000000000000, 0.8321012486987983126, 1.000000000000000000),
 ( 1.000000000000000000, 0.8541932017406910216, 1.000000000000000000),
 ( 1.000000000000000000, 0.8545723906054343288, 1.000000000000000000),
 ( 1.000000000000000000, 0.8327032135043206384, 1.000000000000000000),
 ( 1.000000000000000000, 0.7734559727060463796, 1.000000000000000000),
 ( 1.000000000000000000, 0.7377766653994621837, 1.000000000000000000),
 ( 1.000000000000000000, 0.7071067811865494601, 1.000000000000000000) ) ) 
 REPRESENTATION_ITEM ( '' )  SURFACE ( )  );
#20054 = CARTESIAN_POINT ( 'NONE',  ( 51.15394434968256121, -0.9591183795338193985, 1.387856512383045970 ) ) ;
#20055 = DIRECTION ( 'NONE',  ( 0.000000000000000000, 0.000000000000000000, -1.000000000000000000 ) ) ;
#20056 = VERTEX_POINT ( 'NONE', #23809 ) ;
#20057 = AXIS2_PLACEMENT_3D ( 'NONE', #18403, #25364, #20328 ) ;
#20058 = CARTESIAN_POINT ( 'NONE',  ( 15.76623786017542628, -5.109611055794812451, -1.772889539330472441 ) ) ;
#20059 = CARTESIAN_POINT ( 'NONE',  ( -57.76905989232412963, 2.944486372867092250, 1.699999999999806111 ) ) ;
#20060 = ADVANCED_FACE ( 'NONE', ( #30767 ), #15944, .T. ) ;
#20061 = CARTESIAN_POINT ( 'NONE',  ( 54.23831472968566203, 6.535030234825930151, -2.050000000000189004 ) ) ;
#20062 = AXIS2_PLACEMENT_3D ( 'NONE', #25895, #1360, #23375 ) ;
#20063 = CARTESIAN_POINT ( 'NONE',  ( 51.90000000000001279, -4.241634596362392706, -1.073358427932568526 ) ) ;
#20064 = CARTESIAN_POINT ( 'NONE',  ( -59.19926633714428732, -2.436054758973382750, 1.249712944685305471 ) ) ;
#20065 = AXIS2_PLACEMENT_3D ( 'NONE', #8600, #18276, #22725 ) ;
#20066 = DIRECTION ( 'NONE',  ( 0.000000000000000000, 0.000000000000000000, 1.000000000000000000 ) ) ;
#20067 = CARTESIAN_POINT ( 'NONE',  ( -36.63359589171324870, -3.777141534544250501, -3.869853550719763557 ) ) ;
#20068 = B_SPLINE_CURVE_WITH_KNOTS ( 'NONE', 3,
 ( #29285, #26762, #16799, #27045, #17115, #7598, #5063, #19335, #9812, #462 ),
 .UNSPECIFIED., .F., .F.,
 ( 4, 3, 3, 4 ),
 ( 8.940560153363745023E-19, 6.454972243978038357E-05, 0.0001290994448803190853, 0.0002310882096523268108 ),
 .UNSPECIFIED. ) ;
#20069 = TOROIDAL_SURFACE ( 'NONE', #21592, 1.260000000000000009, 0.01000000000000000021 ) ;
#20070 = AXIS2_PLACEMENT_3D ( 'NONE', #26859, #12753, #22757 ) ;
#20071 = FACE_OUTER_BOUND ( 'NONE', #17303, .T. ) ;
#20072 = EDGE_CURVE ( 'NONE', #15120, #7615, #2791, .T. ) ;
#20073 = DIRECTION ( 'NONE',  ( 1.000000000000000000, 0.000000000000000000, 0.000000000000000000 ) ) ;
#20074 = EDGE_CURVE ( 'NONE', #2309, #26302, #16521, .T. ) ;
#20075 = ORIENTED_EDGE ( 'NONE', *, *, #5613, .F. ) ;
#20076 = DIRECTION ( 'NONE',  ( 0.000000000000000000, 0.000000000000000000, 1.000000000000000000 ) ) ;
#20077 = CARTESIAN_POINT ( 'NONE',  ( -36.56242893520730064, -3.350344226587728791, -4.246692235172065288 ) ) ;
#20078 = CARTESIAN_POINT ( 'NONE',  ( 54.41366571437522737, 6.718673005292171041, -0.9750000000001826095 ) ) ;
#20079 = ORIENTED_EDGE ( 'NONE', *, *, #27093, .F. ) ;
#20080 = DIRECTION ( 'NONE',  ( -1.000000000000000000, 1.219044193948983948E-29, -3.491481338843133355E-15 ) ) ;
#20081 = ORIENTED_EDGE ( 'NONE', *, *, #23601, .T. ) ;
#20082 = DIRECTION ( 'NONE',  ( 0.000000000000000000, 0.000000000000000000, 1.000000000000000000 ) ) ;
#20083 = CARTESIAN_POINT ( 'NONE',  ( -55.22085481156723574, -3.673546848079175753, -0.7533615035078071731 ) ) ;
#20085 = CARTESIAN_POINT ( 'NONE',  ( 51.52258228595268719, -3.791878011401587312, -1.561538262852857351 ) ) ;
#20084 = CARTESIAN_POINT ( 'NONE',  ( 64.00000000000001421, 1.163569835200988601E-28, -1.375000000000224931 ) ) ;
#20086 = CIRCLE ( 'NONE', #6419, 4.099999999999992539 ) ;
#20087 = ORIENTED_EDGE ( 'NONE', *, *, #19725, .T. ) ;
#20088 = CARTESIAN_POINT ( 'NONE',  ( -57.76905989232412963, 2.944486372867089141, 1.699999999999811218 ) ) ;
#20089 = CIRCLE ( 'NONE', #26154, 0.09999999999999972800 ) ;
#20090 = CARTESIAN_POINT ( 'NONE',  ( 61.25000000000004263, -2.079005547593161918, 1.932245437381540134E-15 ) ) ;
#20091 = EDGE_CURVE ( 'NONE', #24434, #2131, #3804, .T. ) ;
#20092 = CIRCLE ( 'NONE', #12988, 0.05000000000000012768 ) ;
#20093 = ORIENTED_EDGE ( 'NONE', *, *, #11052, .F. ) ;
#20095 = CARTESIAN_POINT ( 'NONE',  ( -54.49409853110120139, -1.525884777627348088, -4.047834655405394777 ) ) ;
#20094 = CARTESIAN_POINT ( 'NONE',  ( -77.28999999999996362, 0.2599193648183395489, 0.006474858487196256430 ) ) ;
#20096 = ORIENTED_EDGE ( 'NONE', *, *, #2038, .T. ) ;
#20097 = EDGE_LOOP ( 'NONE', ( #3667, #915, #17266, #29716 ) ) ;
#20098 = CARTESIAN_POINT ( 'NONE',  ( -58.99999999999997158, 3.673546848079180638, 0.7533615035078062849 ) ) ;
#20099 = CYLINDRICAL_SURFACE ( 'NONE', #21124, 3.750000000000000444 ) ;
#20100 = AXIS2_PLACEMENT_3D ( 'NONE', #20616, #30246, #5876 ) ;
#20101 = CARTESIAN_POINT ( 'NONE',  ( -54.49999999999997158, -2.730644924724235700, -2.351390379901977745 ) ) ;
#20102 = DIRECTION ( 'NONE',  ( 1.057355261547768637E-14, 0.000000000000000000, 1.000000000000000000 ) ) ;
#20103 = AXIS2_PLACEMENT_3D ( 'NONE', #19565, #17186, #26830 ) ;
#20104 = CARTESIAN_POINT ( 'NONE',  ( -55.38452994616205416, -3.117691453623976816, 1.799999999999791100 ) ) ;
#20105 = SPHERICAL_SURFACE ( 'NONE', #16993, 0.2500000000000000000 ) ;
#20106 = ADVANCED_FACE ( 'NONE', ( #31069 ), #15441, .T. ) ;
#20107 = ORIENTED_EDGE ( 'NONE', *, *, #31173, .T. ) ;
#20108 = ADVANCED_FACE ( 'NONE', ( #9076 ), #1618, .T. ) ;
#20109 = CARTESIAN_POINT ( 'NONE',  ( 15.29954477411524749, 2.199885872770226403, 4.939696258129626649 ) ) ;
#20110 = CIRCLE ( 'NONE', #24150, 0.1500000000000002720 ) ;
#20111 = CIRCLE ( 'NONE', #14022, 0.09999999999999972800 ) ;
#20112 = CARTESIAN_POINT ( 'NONE',  ( -55.17292740578361077, 2.256877952708270296, -2.542931754211924744 ) ) ;
#20113 = VECTOR ( 'NONE', #18095, 1000.000000000000000 ) ;
#20114 = CARTESIAN_POINT ( 'NONE',  ( -59.69999999999997442, 8.366749974758454467E-15, -2.120534355533670266E-13 ) ) ;
#20115 = EDGE_CURVE ( 'NONE', #24820, #30654, #8765, .T. ) ;
#20116 = EDGE_CURVE ( 'NONE', #22540, #5072, #30609, .T. ) ;
#20117 = CARTESIAN_POINT ( 'NONE',  ( -35.98952425903316765, 4.804073785499212157, -2.042134698606532517 ) ) ;
#20118 = CARTESIAN_POINT ( 'NONE',  ( -36.11692583559979397, 1.123735554575555406, 5.289358692618281843 ) ) ;
#20119 = CARTESIAN_POINT ( 'NONE',  ( 48.41280093284954944, 1.295960864328840279, -3.889961360030776749 ) ) ;
#20120 = EDGE_LOOP ( 'NONE', ( #24034, #15503, #28605, #13851, #6414, #24283 ) ) ;
#20121 = AXIS2_PLACEMENT_3D ( 'NONE', #22622, #8970, #21349 ) ;
#20122 = DIRECTION ( 'NONE',  ( 0.000000000000000000, 0.2008964009354152203, -0.9796124928211138450 ) ) ;
#20123 = AXIS2_PLACEMENT_3D ( 'NONE', #1054, #5972, #25271 ) ;
#20124 = VERTEX_POINT ( 'NONE', #30593 ) ;
#20125 = CIRCLE ( 'NONE', #9424, 1.875000000000001776 ) ;
#20126 = CARTESIAN_POINT ( 'NONE',  ( -59.14182443247880627, 2.482031228406460954, -0.9525887483575969927 ) ) ;
#20128 = DIRECTION ( 'NONE',  ( 0.000000000000000000, 0.000000000000000000, 1.000000000000000000 ) ) ;
#20127 = LINE ( 'NONE', #8221, #8426 ) ;
#20129 = ORIENTED_EDGE ( 'NONE', *, *, #10188, .F. ) ;
#20130 = EDGE_LOOP ( 'NONE', ( #30792, #23715, #17119, #29191 ) ) ;
#20131 = CARTESIAN_POINT ( 'NONE',  ( 47.07708546080149858, 8.766223091587903582, 1.549999999999835953 ) ) ;
#20132 = DIRECTION ( 'NONE',  ( -1.000000000000000000, -3.053848253006669023E-16, 2.042510438544995415E-16 ) ) ;
#20133 = EDGE_LOOP ( 'NONE', ( #5265, #17627 ) ) ;
#20135 = CARTESIAN_POINT ( 'NONE',  ( 51.78448386883093235, -4.158727452193214269, 1.045216533296355665 ) ) ;
#20134 = CARTESIAN_POINT ( 'NONE',  ( -56.50952994616203995, 3.117691453623994580, -1.800000000000187006 ) ) ;
#20136 = CYLINDRICAL_SURFACE ( 'NONE', #26070, 0.2500000000000000000 ) ;
#20137 = AXIS2_PLACEMENT_3D ( 'NONE', #3176, #8549, #641 ) ;
#20138 = CYLINDRICAL_SURFACE ( 'NONE', #16237, 2.000000000000000000 ) ;
#20139 = DIRECTION ( 'NONE',  ( 0.000000000000000000, 0.000000000000000000, 1.000000000000000000 ) ) ;
#20140 = AXIS2_PLACEMENT_3D ( 'NONE', #26023, #21788, #4334 ) ;
#20141 = CARTESIAN_POINT ( 'NONE',  ( 58.72200624034179839, -1.310319377726872903, -1.341335979947030799 ) ) ;
#20142 = AXIS2_PLACEMENT_3D ( 'NONE', #2393, #12338, #22186 ) ;
#20143 = EDGE_CURVE ( 'NONE', #9362, #76, #5315, .T. ) ;
#20144 = ORIENTED_EDGE ( 'NONE', *, *, #12487, .F. ) ;
#20145 = EDGE_CURVE ( 'NONE', #20943, #3021, #27062, .T. ) ;
#20146 = CARTESIAN_POINT ( 'NONE',  ( -60.69702994616205416, -2.078460969082657872, 3.599999999999776712 ) ) ;
#20147 = ADVANCED_FACE ( 'NONE', ( #23481 ), #7846, .F. ) ;
#20148 = CARTESIAN_POINT ( 'NONE',  ( 51.46757676178951613, 4.376162276235349147, -2.050000000000179234 ) ) ;
#20149 = FACE_OUTER_BOUND ( 'NONE', #996, .T. ) ;
#20150 = FACE_OUTER_BOUND ( 'NONE', #24821, .T. ) ;
#20151 = CARTESIAN_POINT ( 'NONE',  ( 33.47623932017462778, -5.377732432866642043, -0.5657657256215583574 ) ) ;
#20153 = FACE_OUTER_BOUND ( 'NONE', #14186, .T. ) ;
#20152 = CARTESIAN_POINT ( 'NONE',  ( -61.39999999999998437, -2.652806974455509170, 0.5026083527760007996 ) ) ;
#20154 = AXIS2_PLACEMENT_3D ( 'NONE', #1972, #28738, #14465 ) ;
#20155 = CARTESIAN_POINT ( 'NONE',  ( -62.07235880193731248, -2.517270094365763100, 0.1974334673667717810 ) ) ;
#20156 = CARTESIAN_POINT ( 'NONE',  ( -64.32138495697122949, 4.896393452479652361E-16, 2.651446950365857792E-15 ) ) ;
#20158 = CARTESIAN_POINT ( 'NONE',  ( -62.09999999999997300, -2.717421493829955459, -0.3515446183602667918 ) ) ;
#20157 = CARTESIAN_POINT ( 'NONE',  ( 58.75000000000000711, 1.655311165517640459, -1.077297519404308179 ) ) ;
#20159 = ORIENTED_EDGE ( 'NONE', *, *, #10257, .T. ) ;
#20160 = CARTESIAN_POINT ( 'NONE',  ( 50.35370852371426764, -1.309359793766436519, -3.864871860988134955 ) ) ;
#20161 = CARTESIAN_POINT ( 'NONE',  ( -67.88621053311027254, -5.990042905486032463E-16, 3.379566295451473069E-15 ) ) ;
#20163 = CYLINDRICAL_SURFACE ( 'NONE', #2496, 3.499999999999999556 ) ;
#20162 = CARTESIAN_POINT ( 'NONE',  ( 15.56274145962646571, 3.953287617511378471, -3.694739123711352047 ) ) ;
#20164 = LINE ( 'NONE', #10943, #28183 ) ;
#20165 = VERTEX_POINT ( 'NONE', #4955 ) ;
#20166 = DIRECTION ( 'NONE',  ( 1.000000000000000000, 1.047444401652940007E-14, 0.000000000000000000 ) ) ;
#20167 = CARTESIAN_POINT ( 'NONE',  ( -62.34999999999997300, 1.091670395932995432E-15, 2.248789515065420326E-15 ) ) ;
#20168 = ORIENTED_EDGE ( 'NONE', *, *, #460, .T. ) ;
#20169 = CARTESIAN_POINT ( 'NONE',  ( 15.32752150720754436, -4.698781674909509931, 2.676750094560135906 ) ) ;
#20170 = ORIENTED_EDGE ( 'NONE', *, *, #11832, .F. ) ;
#20171 = ORIENTED_EDGE ( 'NONE', *, *, #13640, .F. ) ;
#20172 = CARTESIAN_POINT ( 'NONE',  ( 15.71019289815286513, 5.349060760730924180, -0.7993770229878035538 ) ) ;
#20173 = DIRECTION ( 'NONE',  ( 0.000000000000000000, 1.000000000000000000, 3.491481338843130594E-15 ) ) ;
#20174 = EDGE_LOOP ( 'NONE', ( #2840, #8507, #9059, #28994, #6570, #12276 ) ) ;
#20175 =( NAMED_UNIT ( * ) SI_UNIT ( $, .STERADIAN. ) SOLID_ANGLE_UNIT ( ) );
#20176 = CARTESIAN_POINT ( 'NONE',  ( 52.05081297082752911, 4.366207722110991618, -1.447839973523495027 ) ) ;
#20177 = B_SPLINE_CURVE_WITH_KNOTS ( 'NONE', 3,
 ( #18690, #9513, #23593, #28813 ),
 .UNSPECIFIED., .F., .F.,
 ( 4, 4 ),
 ( 3.909146525865938448E-19, 0.0001543670095910078732 ),
 .UNSPECIFIED. ) ;
#20178 = CARTESIAN_POINT ( 'NONE',  ( -58.75952994616203284, 3.117691453623994580, -1.800000000000195000 ) ) ;
#20179 = ORIENTED_EDGE ( 'NONE', *, *, #9608, .F. ) ;
#20180 = CARTESIAN_POINT ( 'NONE',  ( 57.03612573316699041, 0.7785448249619018046, -1.733167030474859205 ) ) ;
#20181 = LINE ( 'NONE', #15397, #15719 ) ;
#20182 = AXIS2_PLACEMENT_3D ( 'NONE', #11696, #4092, #2031 ) ;
#20183 = CARTESIAN_POINT ( 'NONE',  ( 24.17629218427016013, 5.599093920977841421, 2.049999999999914557 ) ) ;
#20184 = VERTEX_POINT ( 'NONE', #19228 ) ;
#20185 = AXIS2_PLACEMENT_3D ( 'NONE', #25046, #25217, #25518 ) ;
#20186 = EDGE_CURVE ( 'NONE', #20985, #8353, #25550, .T. ) ;
#20187 = CIRCLE ( 'NONE', #23224, 1.000000000000000000 ) ;
#20188 =( BOUNDED_SURFACE ( )  B_SPLINE_SURFACE ( 3, 2, ( 
 ( #31050, #181, #9837 ),
 ( #19507, #29153, #17138 ),
 ( #23635, #24400, #12812 ),
 ( #19965, #10005, #29600 ),
 ( #24709, #29925, #22495 ),
 ( #5556, #20141, #22671 ),
 ( #20295, #7923, #10460 ),
 ( #29770, #8235, #17279 ),
 ( #5391, #22201, #12663 ),
 ( #17596, #22344, #5088 ) ),
 .UNSPECIFIED., .F., .F., .F. ) 
 B_SPLINE_SURFACE_WITH_KNOTS ( ( 4, 2, 2, 2, 4 ),
 ( 3, 3 ),
 ( 0.0001706658715698512231, 0.0002229276920781348066, 0.0002751895125864183629, 0.0003274513330947019193, 0.0003797131536029854757 ),
 ( 0.000000000000000000, 1.000000000000000000 ),
 .UNSPECIFIED. ) 
 GEOMETRIC_REPRESENTATION_ITEM ( )  RATIONAL_B_SPLINE_SURFACE ( (
 ( 1.000000000000000000, 0.7071067811873473774, 1.000000000000000000),
 ( 1.000000000000000000, 0.7375607040707745643, 1.000000000000000000),
 ( 1.000000000000000000, 0.7730431127434318483, 1.000000000000000000),
 ( 1.000000000000000000, 0.8321012486982067857, 1.000000000000000000),
 ( 1.000000000000000000, 0.8541932017400749588, 1.000000000000000000),
 ( 1.000000000000000000, 0.8545723906049677021, 1.000000000000000000),
 ( 1.000000000000000000, 0.8327032135039394989, 1.000000000000000000),
 ( 1.000000000000000000, 0.7734559727058835099, 1.000000000000000000),
 ( 1.000000000000000000, 0.7377766653993951262, 1.000000000000000000),
 ( 1.000000000000000000, 0.7071067811865511255, 1.000000000000000000) ) ) 
 REPRESENTATION_ITEM ( '' )  SURFACE ( )  );
#20189 = SPHERICAL_SURFACE ( 'NONE', #28928, 0.1000000000000000056 ) ;
#20190 = CARTESIAN_POINT ( 'NONE',  ( 60.82068433953624265, 0.6500001811784626993, 1.489337021788162296 ) ) ;
#20191 = CARTESIAN_POINT ( 'NONE',  ( 50.25000000000002842, -0.5380862305914007049, 2.008165151418990213 ) ) ;
#20192 = CARTESIAN_POINT ( 'NONE',  ( -44.59999999999996589, 1.400000000000023892, -3.959797974644837293 ) ) ;
#20193 = DIRECTION ( 'NONE',  ( 0.000000000000000000, 0.000000000000000000, 1.000000000000000000 ) ) ;
#20195 = CARTESIAN_POINT ( 'NONE',  ( -54.65400635094609072, 1.737685414808520568, -3.471684241605565102 ) ) ;
#20194 = CARTESIAN_POINT ( 'NONE',  ( -56.94184846062112371, 0.2309624077929111619, 3.875409454552790844 ) ) ;
#20196 = B_SPLINE_CURVE_WITH_KNOTS ( 'NONE', 3,
 ( #28496, #6649, #9191, #2202, #6800, #26117, #19179, #31021, #30537, #8844, #28182, #16153, #25804, #4111, #13750, #1720, #11389, #30719, #18695 ),
 .UNSPECIFIED., .F., .F.,
 ( 4, 3, 3, 3, 3, 3, 4 ),
 ( 0.000000000000000000, 2.270809125664990461E-05, 4.499850898804030560E-05, 6.557565265601914873E-05, 7.920624315363274039E-05, 8.325821076725717102E-05, 9.013793637923205450E-05 ),
 .UNSPECIFIED. ) ;
#20197 = CARTESIAN_POINT ( 'NONE',  ( 50.50000000000002132, -0.6462379109120514054, -4.048750000000023164 ) ) ;
#20198 = EDGE_CURVE ( 'NONE', #9408, #26742, #19691, .T. ) ;
#20199 = CARTESIAN_POINT ( 'NONE',  ( 58.75000000000000711, 1.253243060178337753, -1.394635017528379040 ) ) ;
#20200 = CARTESIAN_POINT ( 'NONE',  ( 48.46374521131294699, -1.419210040599374612, 3.846553521706499001 ) ) ;
#20201 = VERTEX_POINT ( 'NONE', #9857 ) ;
#20202 = CARTESIAN_POINT ( 'NONE',  ( -54.49454330418567594, 1.526701536696945638, 3.317245250669464518 ) ) ;
#20203 = ORIENTED_EDGE ( 'NONE', *, *, #14792, .F. ) ;
#20204 = CIRCLE ( 'NONE', #20728, 1.351996603031850208 ) ;
#20205 = ORIENTED_EDGE ( 'NONE', *, *, #9159, .F. ) ;
#20206 = DIRECTION ( 'NONE',  ( -1.000000000000000000, -0.000000000000000000, 3.491481338843133355E-15 ) ) ;
#20207 = PRODUCT ( 'Cap', 'Cap', '', ( #13591 ) ) ;
#20208 = CARTESIAN_POINT ( 'NONE',  ( -59.11042740578359656, -2.936324665650201560, -2.606018187048497747 ) ) ;
#20210 = CARTESIAN_POINT ( 'NONE',  ( -59.67491082927361390, 2.027450992888311543, 1.706680806714727883 ) ) ;
#20209 = CARTESIAN_POINT ( 'NONE',  ( -55.87499999999996447, 2.944486372867106905, -1.700000000000186029 ) ) ;
#20211 = EDGE_LOOP ( 'NONE', ( #4655, #9909, #5666, #23528 ) ) ;
#20212 = ORIENTED_EDGE ( 'NONE', *, *, #2752, .T. ) ;
#20213 = CARTESIAN_POINT ( 'NONE',  ( 54.12879229448595453, 6.030824283042129252, -2.034063242164690255 ) ) ;
#20214 = EDGE_LOOP ( 'NONE', ( #8194, #17848, #829, #9493, #16766, #16387, #3485, #14830, #747, #12296 ) ) ;
#20215 = DIRECTION ( 'NONE',  ( -0.000000000000000000, -1.000000000000000000, -0.000000000000000000 ) ) ;
#20216 = VERTEX_POINT ( 'NONE', #4784 ) ;
#20217 = CARTESIAN_POINT ( 'NONE',  ( 27.84544208489333172, 5.444976783748663784, -1.950000000000065459 ) ) ;
#20218 = ORIENTED_EDGE ( 'NONE', *, *, #27216, .T. ) ;
#20219 = LINE ( 'NONE', #10545, #7600 ) ;
#20220 = CIRCLE ( 'NONE', #28286, 2.050000000000000266 ) ;
#20221 = CARTESIAN_POINT ( 'NONE',  ( 58.65000000000003411, -1.253243060177392953, -1.394635017528123910 ) ) ;
#20222 = EDGE_CURVE ( 'NONE', #1083, #23320, #4810, .T. ) ;
#20223 = CIRCLE ( 'NONE', #9077, 3.200000000000000178 ) ;
#20224 = CARTESIAN_POINT ( 'NONE',  ( 15.41080140630285022, -4.895960019030861865, -2.323379425334049397 ) ) ;
#20225 = CARTESIAN_POINT ( 'NONE',  ( -57.20655989232410832, 1.962990915244748891, -3.400000000000194422 ) ) ;
#20226 = CARTESIAN_POINT ( 'NONE',  ( 47.21114320858165314, -3.753732476607509749, 1.652583012570356669 ) ) ;
#20227 = CARTESIAN_POINT ( 'NONE',  ( 47.38200087219854595, -3.967692247893680690, -1.365930198224970749 ) ) ;
#20228 = CIRCLE ( 'NONE', #26288, 3.499999999999999556 ) ;
#20229 = CARTESIAN_POINT ( 'NONE',  ( 48.45869172792486523, 1.344780351710889610, 3.858600739747802599 ) ) ;
#20230 = CARTESIAN_POINT ( 'NONE',  ( 58.75000000000000711, 1.666164585743217463, -1.106298139389324975 ) ) ;
#20231 = CARTESIAN_POINT ( 'NONE',  ( 29.12648003328355983, 5.963603948890924045, -1.950000000000100320 ) ) ;
#20232 = CIRCLE ( 'NONE', #11120, 1.850000000000000089 ) ;
#20233 = CARTESIAN_POINT ( 'NONE',  ( -58.65835481156723574, 4.108500314926515351, -1.367561758111408121 ) ) ;
#20234 = PLANE ( 'NONE',  #24642 ) ;
#20235 = CARTESIAN_POINT ( 'NONE',  ( 51.44193764627956256, -0.9752197701239264660, 1.304631266258929889 ) ) ;
#20236 = ORIENTED_EDGE ( 'NONE', *, *, #17397, .T. ) ;
#20237 = DIRECTION ( 'NONE',  ( 1.000000000000000000, 1.047444401652940007E-14, 0.000000000000000000 ) ) ;
#20238 = CARTESIAN_POINT ( 'NONE',  ( 54.44703553012594455, 6.360744381977848860, 0.9749999999998122391 ) ) ;
#20239 = ORIENTED_EDGE ( 'NONE', *, *, #22754, .T. ) ;
#20240 = CARTESIAN_POINT ( 'NONE',  ( 69.25000000000004263, 0.6441176470588245717, 1.707553061179924114 ) ) ;
#20241 = ORIENTED_EDGE ( 'NONE', *, *, #7620, .F. ) ;
#20242 =( BOUNDED_CURVE ( )  B_SPLINE_CURVE ( 2, ( #16287, #21215, #28317, #8817, #6624, #9165, #18826 ),
 .UNSPECIFIED., .F., .T. ) 
 B_SPLINE_CURVE_WITH_KNOTS ( ( 3, 2, 2, 3 ),
 ( 0.7554854200587094448, 0.7592592592592593004, 0.7777777777777777901, 0.7874476280263653649 ),
 .UNSPECIFIED. ) 
 CURVE ( )  GEOMETRIC_REPRESENTATION_ITEM ( )  RATIONAL_B_SPLINE_CURVE ( ( 0.9565230875206803818, 0.9726976765138894976, 1.000000000000000000, 0.8660254037844387076, 1.000000000000000000, 0.9300422287439487068, 0.9331444240391612022 ) ) 
 REPRESENTATION_ITEM ( '' )  );
#20243 = CARTESIAN_POINT ( 'NONE',  ( 15.61552784268253902, -0.4851603899461495728, -5.391500295856416436 ) ) ;
#20244 = CARTESIAN_POINT ( 'NONE',  ( -36.23324115033480552, -5.027926281937912023, 1.353187539901980152 ) ) ;
#20246 = CARTESIAN_POINT ( 'NONE',  ( 61.25000000000000711, 1.666164585742400117, 1.106298139391003632 ) ) ;
#20245 = DIRECTION ( 'NONE',  ( 1.000000000000000000, 0.000000000000000000, 0.000000000000000000 ) ) ;
#20247 = ADVANCED_FACE ( 'NONE', ( #14759 ), #29591, .T. ) ;
#20248 = ORIENTED_EDGE ( 'NONE', *, *, #29535, .T. ) ;
#20249 = CARTESIAN_POINT ( 'NONE',  ( 51.59739104186229497, -1.165722629540969058, -1.468576096419531574 ) ) ;
#20250 = CIRCLE ( 'NONE', #24281, 2.374999999999998668 ) ;
#20251 = DIRECTION ( 'NONE',  ( 0.000000000000000000, 0.000000000000000000, 1.000000000000000000 ) ) ;
#20252 = EDGE_LOOP ( 'NONE', ( #26312, #9366, #19967, #21952 ) ) ;
#20254 = CARTESIAN_POINT ( 'NONE',  ( -73.89999999999997726, -2.435524336289708093E-15, 4.607889071584891164E-15 ) ) ;
#20253 = CARTESIAN_POINT ( 'NONE',  ( 54.41366571437522026, 6.718673005292167488, 1.949999999999809663 ) ) ;
#20255 = VERTEX_POINT ( 'NONE', #26801 ) ;
#20256 = ORIENTED_EDGE ( 'NONE', *, *, #23186, .T. ) ;
#20257 = CARTESIAN_POINT ( 'NONE',  ( 53.91574522233626965, 6.672251602764244893, -1.774295313897662485 ) ) ;
#20258 = CARTESIAN_POINT ( 'NONE',  ( 56.95220615073115056, -0.7055010433615873655, 1.764201441664152270 ) ) ;
#20259 = FACE_OUTER_BOUND ( 'NONE', #20821, .T. ) ;
#20260 = CIRCLE ( 'NONE', #28330, 3.950000000000000178 ) ;
#20261 = EDGE_CURVE ( 'NONE', #29380, #20706, #12908, .T. ) ;
#20262 = FACE_OUTER_BOUND ( 'NONE', #22123, .T. ) ;
#20263 = DIRECTION ( 'NONE',  ( 0.7071067811865462405, 0.7068874824028876791, 0.01760929362890746239 ) ) ;
#20264 = EDGE_CURVE ( 'NONE', #1297, #1993, #508, .T. ) ;
#20265 = CARTESIAN_POINT ( 'NONE',  ( -54.75952994616206837, -4.643455692769931152E-15, 3.599999999999804245 ) ) ;
#20266 = EDGE_CURVE ( 'NONE', #8829, #13929, #14925, .T. ) ;
#20267 = EDGE_LOOP ( 'NONE', ( #24487, #19748, #28732, #24036 ) ) ;
#20268 = DIRECTION ( 'NONE',  ( 0.000000000000000000, -1.000000000000000000, -3.491481338843132961E-15 ) ) ;
#20269 = FACE_OUTER_BOUND ( 'NONE', #12123, .T. ) ;
#20270 = EDGE_CURVE ( 'NONE', #18295, #4290, #26649, .T. ) ;
#20271 = DIRECTION ( 'NONE',  ( -1.000000000000000000, -0.000000000000000000, -0.000000000000000000 ) ) ;
#20272 = CARTESIAN_POINT ( 'NONE',  ( -56.88452994616205416, -3.117691453623982145, 1.799999999999776890 ) ) ;
#20274 = CIRCLE ( 'NONE', #6610, 1.000000000000000000 ) ;
#20273 = CARTESIAN_POINT ( 'NONE',  ( 58.74999999999981526, -1.872332544500615370, 0.09997921184705542419 ) ) ;
#20275 = CARTESIAN_POINT ( 'NONE',  ( 27.51012318650851896, 5.457609198730995814, 2.049999999999903011 ) ) ;
#20276 = VERTEX_POINT ( 'NONE', #5106 ) ;
#20277 = DIRECTION ( 'NONE',  ( 0.000000000000000000, -0.3529411764705863708, 0.9356455129756987565 ) ) ;
#20278 = ORIENTED_EDGE ( 'NONE', *, *, #14263, .T. ) ;
#20279 = UNCERTAINTY_MEASURE_WITH_UNIT (LENGTH_MEASURE( 1.000000000000000082E-05 ), #24942, 'distance_accuracy_value', 'NONE');
#20280 = CARTESIAN_POINT ( 'NONE',  ( 47.10000000000002984, -3.550773357292059007, 2.049880134335656745 ) ) ;
#20282 = CARTESIAN_POINT ( 'NONE',  ( -67.33025350686975230, 2.149980434289362030, 0.05355822207392273160 ) ) ;
#20281 = CARTESIAN_POINT ( 'NONE',  ( 15.03925126672132961, -3.426725943139531605, -3.937891353488756963 ) ) ;
#20283 = EDGE_CURVE ( 'NONE', #28852, #22920, #29177, .T. ) ;
#20284 = VERTEX_POINT ( 'NONE', #7494 ) ;
#20285 = ORIENTED_EDGE ( 'NONE', *, *, #21867, .T. ) ;
#20286 = DIRECTION ( 'NONE',  ( 1.000000000000000000, 0.000000000000000000, -1.047444401652940007E-14 ) ) ;
#20287 = CARTESIAN_POINT ( 'NONE',  ( 23.27131915274573615, 6.595123925190214287, -1.425000000000080869 ) ) ;
#20288 = ORIENTED_EDGE ( 'NONE', *, *, #19445, .F. ) ;
#20290 = CYLINDRICAL_SURFACE ( 'NONE', #3905, 0.1000000000000001721 ) ;
#20289 = CARTESIAN_POINT ( 'NONE',  ( -57.88452994616205416, 3.117691453623979481, 1.799999999999806422 ) ) ;
#20291 = CARTESIAN_POINT ( 'NONE',  ( -58.79792740578360366, 3.330682475591789427, 0.6830477631804110494 ) ) ;
#20292 = LINE ( 'NONE', #6032, #22354 ) ;
#20293 = SHAPE_DEFINITION_REPRESENTATION ( #6837, #15725 ) ;
#20294 = EDGE_CURVE ( 'NONE', #5230, #16210, #23327, .T. ) ;
#20295 = CARTESIAN_POINT ( 'NONE',  ( 58.75000018803720536, -1.333992738916506271, -1.403930843796631578 ) ) ;
#20296 = FILL_AREA_STYLE ('',( #12664 ) ) ;
#20297 = ADVANCED_FACE ( 'NONE', ( #19376 ), #10884, .T. ) ;
#20298 = CIRCLE ( 'NONE', #22826, 0.05000000000000009298 ) ;
#20299 = EDGE_CURVE ( 'NONE', #5910, #14916, #17298, .T. ) ;
#20300 = VERTEX_POINT ( 'NONE', #22219 ) ;
#20301 = DIRECTION ( 'NONE',  ( 0.000000000000000000, -0.9996898646859344595, -0.02490330187381124133 ) ) ;
#20302 = CARTESIAN_POINT ( 'NONE',  ( 54.23267447929806906, 6.619944661321486734, -2.050000000000189004 ) ) ;
#20303 = CARTESIAN_POINT ( 'NONE',  ( -57.77499999999997016, 2.796048871338436190E-15, 1.138853883557972617E-16 ) ) ;
#20304 = CARTESIAN_POINT ( 'NONE',  ( 15.22780280894163063, -0.7747498539018873309, 5.363501450340581123 ) ) ;
#20305 = CARTESIAN_POINT ( 'NONE',  ( 41.48619405472009447, -151.3359592902261852, -1.550000000000163469 ) ) ;
#20307 = CARTESIAN_POINT ( 'NONE',  ( 47.09104525948223596, 9.165979422395388099, -2.050000000000163691 ) ) ;
#20306 = DIRECTION ( 'NONE',  ( -0.9993908270190957621, 0.03489949670250097613, 3.491481338843133355E-15 ) ) ;
#20308 = PRESENTATION_LAYER_ASSIGNMENT (  '', '', ( #1567 ) ) ;
#20309 = CARTESIAN_POINT ( 'NONE',  ( -59.29999999999997584, -0.7533615035078030653, 3.673546848079178417 ) ) ;
#20310 = CARTESIAN_POINT ( 'NONE',  ( -59.96464466094062828, 0.9714054848608624226, -4.736774497371789572 ) ) ;
#20312 = DIRECTION ( 'NONE',  ( 1.000000000000000000, 1.047444401652940007E-14, 0.000000000000000000 ) ) ;
#20311 = CARTESIAN_POINT ( 'NONE',  ( -59.49999999999997158, 2.944486372867082924, 1.699999999999817435 ) ) ;
#20313 = VERTEX_POINT ( 'NONE', #23960 ) ;
#20314 = DIRECTION ( 'NONE',  ( 9.824982518806699669E-15, 0.000000000000000000, 1.000000000000000000 ) ) ;
#20315 = CARTESIAN_POINT ( 'NONE',  ( -36.52679053911622020, 3.858136107555827810, -3.790289750283414527 ) ) ;
#20317 = CARTESIAN_POINT ( 'NONE',  ( 58.66107449606974455, -0.9081280691412084716, -1.640741681270376340 ) ) ;
#20316 = CARTESIAN_POINT ( 'NONE',  ( 51.25000000000002842, -0.9938153758920951208, -1.589954715908409977 ) ) ;
#20318 = PLANE ( 'NONE',  #889 ) ;
#20319 = EDGE_CURVE ( 'NONE', #7544, #21318, #29114, .T. ) ;
#20320 = ORIENTED_EDGE ( 'NONE', *, *, #21625, .T. ) ;
#20321 = CARTESIAN_POINT ( 'NONE',  ( 51.29777716379116725, 3.891287491069770343, 2.049999999999820410 ) ) ;
#20322 = CARTESIAN_POINT ( 'NONE',  ( -60.60807700862574166, -2.449477319984247892, -1.080610302189543459 ) ) ;
#20323 = EDGE_LOOP ( 'NONE', ( #8333, #30810 ) ) ;
#20324 = EDGE_CURVE ( 'NONE', #17296, #8955, #266, .T. ) ;
#20325 = CARTESIAN_POINT ( 'NONE',  ( 51.80000000000003979, 6.982261990806648555E-14, 4.499999999999857003 ) ) ;
#20326 = VERTEX_POINT ( 'NONE', #7326 ) ;
#20327 = CARTESIAN_POINT ( 'NONE',  ( 15.59055531549694074, 2.334444681449764136, -4.877899991435246108 ) ) ;
#20328 = DIRECTION ( 'NONE',  ( 9.329605248950888974E-15, -1.000000000000000000, 0.000000000000000000 ) ) ;
#20329 = ORIENTED_EDGE ( 'NONE', *, *, #6148, .T. ) ;
#20330 = SURFACE_STYLE_FILL_AREA ( #29642 ) ;
#20331 = CARTESIAN_POINT ( 'NONE',  ( -54.49999999999997868, 0.000000000000000000, 0.000000000000000000 ) ) ;
#20332 = CIRCLE ( 'NONE', #2108, 0.05000000000000008604 ) ;
#20333 = CARTESIAN_POINT ( 'NONE',  ( -59.44702994616203995, 4.156921938165313080, -1.958927657850919798E-13 ) ) ;
#20334 = ORIENTED_EDGE ( 'NONE', *, *, #19592, .F. ) ;
#20335 = CARTESIAN_POINT ( 'NONE',  ( 69.20000000000001705, -0.4500000000000000111, -1.988246715074081017 ) ) ;
#20336 = CARTESIAN_POINT ( 'NONE',  ( 58.75000000000000711, 1.106298139389943147, 1.666164585743605375 ) ) ;
#20337 = EDGE_CURVE ( 'NONE', #2793, #17885, #3321, .T. ) ;
#20338 = CARTESIAN_POINT ( 'NONE',  ( 26.61920844898531868, 5.219578738934654183, 1.949999999999841860 ) ) ;
#20339 = ORIENTED_EDGE ( 'NONE', *, *, #30815, .T. ) ;
#20340 = CIRCLE ( 'NONE', #20825, 2.750000000000000000 ) ;
#20341 = CARTESIAN_POINT ( 'NONE',  ( -55.24999999999996447, 2.023778652682505581E-14, -3.400000000000196643 ) ) ;
#20342 = DIRECTION ( 'NONE',  ( 1.000000000000000000, 1.047444401652940007E-14, 0.000000000000000000 ) ) ;
#20343 = LINE ( 'NONE', #29969, #12724 ) ;
#20344 = CARTESIAN_POINT ( 'NONE',  ( -44.49999999999999289, -1.499999999999999556, -4.029888335921975262 ) ) ;
#20345 = DIRECTION ( 'NONE',  ( 1.000000000000000000, -1.219044193948983948E-29, 3.491481338843133355E-15 ) ) ;
#20347 = DIRECTION ( 'NONE',  ( -0.6819983600624907050, 0.7313537016191778983, 2.168404344971033323E-15 ) ) ;
#20346 = CARTESIAN_POINT ( 'NONE',  ( -54.49999999999997868, 3.796242339859525868E-15, -5.550248518040434488E-16 ) ) ;
#20348 = CARTESIAN_POINT ( 'NONE',  ( 51.41935677334221566, 0.9814903265946437472, 1.432156770616830554 ) ) ;
#20349 = CARTESIAN_POINT ( 'NONE',  ( -59.60191903105513234, 2.337626997591227163, -1.248237806062581168 ) ) ;
#20350 = DIRECTION ( 'NONE',  ( 0.000000000000000000, 0.1576190026614809614, 0.9875000000000001554 ) ) ;
#20351 = CARTESIAN_POINT ( 'NONE',  ( 58.74160516400052501, 1.258299259017965355, -1.390091577294809699 ) ) ;
#20352 = CARTESIAN_POINT ( 'NONE',  ( 54.15673930838963912, 5.684321142249388892, 2.049999999999811529 ) ) ;
#20353 = TOROIDAL_SURFACE ( 'NONE', #8200, 4.600000000000000533, 0.5000000000000013323 ) ;
#20354 = B_SPLINE_CURVE_WITH_KNOTS ( 'NONE', 3,
 ( #21994, #5191, #29411, #24819, #10256, #26570, #5336 ),
 .UNSPECIFIED., .F., .F.,
 ( 4, 3, 4 ),
 ( 0.000000000000000000, 3.138403403613116213E-05, 4.417314921333021443E-05 ),
 .UNSPECIFIED. ) ;
#20355 = ORIENTED_EDGE ( 'NONE', *, *, #5828, .F. ) ;
#20356 = DIRECTION ( 'NONE',  ( 0.000000000000000000, 0.000000000000000000, 1.000000000000000000 ) ) ;
#20357 = ADVANCED_FACE ( 'NONE', ( #22513 ), #10780, .T. ) ;
#20358 = DIRECTION ( 'NONE',  ( -1.000000000000000000, 0.000000000000000000, 3.491481338843132961E-15 ) ) ;
#20359 = EDGE_CURVE ( 'NONE', #24008, #9539, #19834, .T. ) ;
#20360 = ORIENTED_EDGE ( 'NONE', *, *, #10592, .T. ) ;
#20361 = VERTEX_POINT ( 'NONE', #1128 ) ;
#20362 = EDGE_CURVE ( 'NONE', #27904, #13707, #8355, .T. ) ;
#20363 = CARTESIAN_POINT ( 'NONE',  ( -62.07342829042941901, -2.504415692620788114, -0.3217612745991157430 ) ) ;
#20364 = CARTESIAN_POINT ( 'NONE',  ( -59.54792740578360366, 3.330682475591789427, 0.6830477631804111605 ) ) ;
#20366 = CARTESIAN_POINT ( 'NONE',  ( -61.39639585615719142, -2.605025371766806153, 0.7093239484020297247 ) ) ;
#20365 = CARTESIAN_POINT ( 'NONE',  ( -55.99999999999995737, 2.023778652682506212E-14, -3.400000000000199307 ) ) ;
#20367 = ORIENTED_EDGE ( 'NONE', *, *, #3426, .T. ) ;
#20368 = VERTEX_POINT ( 'NONE', #3190 ) ;
#20369 = CARTESIAN_POINT ( 'NONE',  ( 54.22156662858499487, 6.014361416436350360, -2.050000000000191225 ) ) ;
#20370 = VERTEX_POINT ( 'NONE', #27096 ) ;
#20371 =( BOUNDED_CURVE ( )  B_SPLINE_CURVE ( 3, ( #17990, #6118, #28103, #3434 ),
 .UNSPECIFIED., .F., .T. ) 
 B_SPLINE_CURVE_WITH_KNOTS ( ( 4, 4 ),
 ( 1.570796326794895892, 3.141592653589791784 ),
 .UNSPECIFIED. ) 
 CURVE ( )  GEOMETRIC_REPRESENTATION_ITEM ( )  RATIONAL_B_SPLINE_CURVE ( ( 1.000000000000000000, 0.8047378541243652705, 0.8047378541243652705, 1.000000000000000000 ) ) 
 REPRESENTATION_ITEM ( '' )  );
#20372 = VERTEX_POINT ( 'NONE', #17920 ) ;
#20373 = CARTESIAN_POINT ( 'NONE',  ( 23.13461596521335650, 6.279931474728896568, -2.050000000000080647 ) ) ;
#20374 = VECTOR ( 'NONE', #1142, 1000.000000000000000 ) ;
#20375 = DIRECTION ( 'NONE',  ( -1.000000000000000000, -0.000000000000000000, -0.000000000000000000 ) ) ;
#20376 = EDGE_CURVE ( 'NONE', #15713, #13616, #29789, .T. ) ;
#20377 = CARTESIAN_POINT ( 'NONE',  ( -44.59999999999998721, -1.500000000000006661, 3.959797974644484242 ) ) ;
#20378 = CARTESIAN_POINT ( 'NONE',  ( -59.64405989232410832, -2.944486372867076263, -1.700000000000222222 ) ) ;
#20379 = CARTESIAN_POINT ( 'NONE',  ( 47.00000000000002842, -3.550773357292058563, 2.049880134335657189 ) ) ;
#20380 = DIRECTION ( 'NONE',  ( 0.000000000000000000, 1.224646799147353207E-16, 1.000000000000000000 ) ) ;
#20381 = CARTESIAN_POINT ( 'NONE',  ( 48.45343659158886851, 1.329326705022644051, 3.861343257506216098 ) ) ;
#20382 = CARTESIAN_POINT ( 'NONE',  ( 58.75000000000002132, -0.4991259882252805924, 1.863313159666098562 ) ) ;
#20384 = DIRECTION ( 'NONE',  ( -1.000000000000000000, -3.385297212316223527E-16, -2.459562394685754633E-16 ) ) ;
#20383 = CARTESIAN_POINT ( 'NONE',  ( -60.85363833753317664, -2.496020359703504443, 0.8457863545849919618 ) ) ;
#20385 = CARTESIAN_POINT ( 'NONE',  ( -44.49999999999997868, 8.366749974758269874E-15, -1.589829192029513996E-13 ) ) ;
#20386 = CARTESIAN_POINT ( 'NONE',  ( -58.81684846062111660, -0.2309624077929090247, -3.875409454552789512 ) ) ;
#20387 = FACE_OUTER_BOUND ( 'NONE', #12249, .T. ) ;
#20388 = VECTOR ( 'NONE', #15745, 1000.000000000000000 ) ;
#20389 = VERTEX_POINT ( 'NONE', #7950 ) ;
#20390 = CARTESIAN_POINT ( 'NONE',  ( 50.55256015243839585, -0.05146993878536944289, 0.7900664826958423426 ) ) ;
#20391 = CARTESIAN_POINT ( 'NONE',  ( 54.18344080464222401, 5.675363110172368053, 2.049999999999807532 ) ) ;
#20392 = VERTEX_POINT ( 'NONE', #19984 ) ;
#20393 = EDGE_CURVE ( 'NONE', #24580, #7153, #22983, .T. ) ;
#20394 = CARTESIAN_POINT ( 'NONE',  ( 51.12687253673779253, 0.9194130538826112975, -1.491219977510798378 ) ) ;
#20395 = VERTEX_POINT ( 'NONE', #27413 ) ;
#20396 = FACE_OUTER_BOUND ( 'NONE', #29907, .T. ) ;
#20397 = FACE_OUTER_BOUND ( 'NONE', #2085, .T. ) ;
#20399 = LINE ( 'NONE', #8338, #12145 ) ;
#20398 = CARTESIAN_POINT ( 'NONE',  ( 60.75000000000003553, -0.4999999999993604560, 1.718465885608478239 ) ) ;
#20400 = ORIENTED_EDGE ( 'NONE', *, *, #2460, .T. ) ;
#20401 = DIRECTION ( 'NONE',  ( 0.000000000000000000, 1.000000000000000000, 0.000000000000000000 ) ) ;
#20402 = CARTESIAN_POINT ( 'NONE',  ( 57.00000000000001421, -0.7049799947465446026, -1.816196764953787124 ) ) ;
#20403 = ORIENTED_EDGE ( 'NONE', *, *, #4535, .T. ) ;
#20405 = CARTESIAN_POINT ( 'NONE',  ( 56.95000000000001705, 0.000000000000000000, 0.000000000000000000 ) ) ;
#20404 = DIRECTION ( 'NONE',  ( 0.000000000000000000, 0.000000000000000000, -1.000000000000000000 ) ) ;
#20406 = DIRECTION ( 'NONE',  ( -0.000000000000000000, 0.2573099415204678775, -0.9663289263986324373 ) ) ;
#20407 = ORIENTED_EDGE ( 'NONE', *, *, #5661, .F. ) ;
#20408 = CARTESIAN_POINT ( 'NONE',  ( -36.68866260399460799, 5.321612844166190293, -0.9647713018066405022 ) ) ;
#20409 = CARTESIAN_POINT ( 'NONE',  ( 58.74160516400047527, 1.575205926126477696, -1.017053542743697303 ) ) ;
#20410 = EDGE_CURVE ( 'NONE', #26590, #8076, #5854, .T. ) ;
#20411 = CARTESIAN_POINT ( 'NONE',  ( -36.00201293083839005, -2.199885893005511850, 4.939696249117965898 ) ) ;
#20412 = DIRECTION ( 'NONE',  ( 0.000000000000000000, -1.000000000000000000, 0.000000000000000000 ) ) ;
#20414 = CARTESIAN_POINT ( 'NONE',  ( -55.32202994616205416, -4.156921938165296204, -2.115361882398036228E-13 ) ) ;
#20413 = AXIS2_PLACEMENT_3D ( 'NONE', #17406, #27052, #5368 ) ;
#20415 = AXIS2_PLACEMENT_3D ( 'NONE', #12536, #19985, #29179 ) ;
#20416 = ORIENTED_EDGE ( 'NONE', *, *, #26582, .F. ) ;
#20417 = CARTESIAN_POINT ( 'NONE',  ( 15.49676243306307200, 3.010474646410398414, 4.240315621469719076 ) ) ;
#20418 = ADVANCED_FACE ( 'NONE', ( #22840 ), #19495, .F. ) ;
#20419 = CARTESIAN_POINT ( 'NONE',  ( -60.64999999999998437, -2.511038422848939078, 0.9923134781793048198 ) ) ;
#20420 = CARTESIAN_POINT ( 'NONE',  ( 47.00000000000000711, 2.480048031931718505E-14, -4.200000000000156497 ) ) ;
#20421 = FACE_OUTER_BOUND ( 'NONE', #28223, .T. ) ;
#20422 = CARTESIAN_POINT ( 'NONE',  ( -56.38452994616205416, 3.117691453623977260, 1.799999999999815747 ) ) ;
#20423 = CARTESIAN_POINT ( 'NONE',  ( 58.74999981404336324, -1.953940384111413575, 0.08513245267583949283 ) ) ;
#20424 = CARTESIAN_POINT ( 'NONE',  ( 22.08710231755535958, 7.931663834300023197, 2.049999999999922995 ) ) ;
#20425 = ORIENTED_EDGE ( 'NONE', *, *, #18598, .T. ) ;
#20426 = ADVANCED_FACE ( 'NONE', ( #13005 ), #12038, .T. ) ;
#20427 = CARTESIAN_POINT ( 'NONE',  ( -77.28999999999996362, -3.470778894058966809E-15, 5.300300110251643219E-15 ) ) ;
#20428 = EDGE_LOOP ( 'NONE', ( #10678, #20780, #12877 ) ) ;
#20429 = CARTESIAN_POINT ( 'NONE',  ( -59.13174955718955772, 2.476889386167965945, -0.9565396329281473653 ) ) ;
#20430 = AXIS2_PLACEMENT_3D ( 'NONE', #584, #15151, #29718 ) ;
#20432 = LINE ( 'NONE', #6021, #19730 ) ;
#20431 = CARTESIAN_POINT ( 'NONE',  ( 48.44664364291948999, 1.310522848978987298, 3.864668279552719632 ) ) ;
#20433 = ORIENTED_EDGE ( 'NONE', *, *, #1043, .T. ) ;
#20434 = VERTEX_POINT ( 'NONE', #18866 ) ;
#20435 = CARTESIAN_POINT ( 'NONE',  ( -58.95655989232411542, -3.399999999999991029, -2.281093130107142867E-13 ) ) ;
#20436 = CARTESIAN_POINT ( 'NONE',  ( 30.51261366513613993, 7.487866468533194819, -1.425000000000106404 ) ) ;
#20437 = ORIENTED_EDGE ( 'NONE', *, *, #5908, .F. ) ;
#20439 = CARTESIAN_POINT ( 'NONE',  ( 33.47623932017462778, 1.734723475976807094E-15, 0.000000000000000000 ) ) ;
#20438 = CARTESIAN_POINT ( 'NONE',  ( -57.32202994616202574, 2.078460969082674747, -3.600000000000194600 ) ) ;
#20440 = CARTESIAN_POINT ( 'NONE',  ( -59.29792740578359656, -2.256877952708263635, 2.542931754211925188 ) ) ;
#20441 = CARTESIAN_POINT ( 'NONE',  ( 64.00000000000001421, 1.990051048615640789E-16, -1.625000000000225153 ) ) ;
#20442 = PRODUCT_CONTEXT ( 'NONE', #9144, 'mechanical' ) ;
#20443 = EDGE_CURVE ( 'NONE', #31166, #4296, #23448, .T. ) ;
#20444 = CARTESIAN_POINT ( 'NONE',  ( -61.39263535326296051, -2.625539631637058502, -0.6290288465273202734 ) ) ;
#20445 =( NAMED_UNIT ( * ) SI_UNIT ( $, .STERADIAN. ) SOLID_ANGLE_UNIT ( ) );
#20446 = ORIENTED_EDGE ( 'NONE', *, *, #6548, .T. ) ;
#20447 = CARTESIAN_POINT ( 'NONE',  ( 47.00000000000002132, -4.137078223593629644, -1.088692053889325440 ) ) ;
#20448 = CARTESIAN_POINT ( 'NONE',  ( 53.66376481541391996, 4.683274397263343047, -2.050000000000186784 ) ) ;
#20449 = DIRECTION ( 'NONE',  ( 1.000000000000000000, 1.047444401652940007E-14, 0.000000000000000000 ) ) ;
#20450 = VECTOR ( 'NONE', #16923, 1000.000000000000000 ) ;
#20451 = CARTESIAN_POINT ( 'NONE',  ( 15.03925126672132961, -2.199885893005945725, 4.939696249117685234 ) ) ;
#20452 = EDGE_CURVE ( 'NONE', #7041, #30150, #27882, .T. ) ;
#20453 = DIRECTION ( 'NONE',  ( -1.000000000000000000, -3.054025858079668409E-16, 2.042474015755241579E-16 ) ) ;
#20454 = CARTESIAN_POINT ( 'NONE',  ( 58.65263613458537151, -1.827305695290488030, -0.4205413283053403006 ) ) ;
#20455 = AXIS2_PLACEMENT_3D ( 'NONE', #20731, #24973, #15799 ) ;
#20456 = CIRCLE ( 'NONE', #13344, 0.1500000000000000777 ) ;
#20457 = DIRECTION ( 'NONE',  ( -1.387778780781445676E-14, 1.000000000000000000, 0.000000000000000000 ) ) ;
#20458 = CARTESIAN_POINT ( 'NONE',  ( 52.79212554374781519, 4.124817749204305883, -2.046663969066548905 ) ) ;
#20460 = CARTESIAN_POINT ( 'NONE',  ( -54.50000000000000000, 2.751381343271932067, -2.278180102673284413 ) ) ;
#20459 = DIRECTION ( 'NONE',  ( 0.000000000000000000, 0.000000000000000000, -1.000000000000000000 ) ) ;
#20461 = ORIENTED_EDGE ( 'NONE', *, *, #26690, .T. ) ;
#20462 = ADVANCED_FACE ( 'NONE', ( #9039 ), #16169, .T. ) ;
#20463 = DIRECTION ( 'NONE',  ( 1.000000000000000000, 1.047444401652940007E-14, 0.000000000000000000 ) ) ;
#20464 = ADVANCED_FACE ( 'NONE', ( #8862 ), #28591, .T. ) ;
#20465 = CARTESIAN_POINT ( 'NONE',  ( -36.40793637698146057, 3.917775493694425570, -3.727542820438198401 ) ) ;
#20467 = CARTESIAN_POINT ( 'NONE',  ( 47.19826578991445842, -3.901954665936025801, -1.539656138810913788 ) ) ;
#20466 = CARTESIAN_POINT ( 'NONE',  ( 15.03925126672125501, 3.779372838781817290, -3.883777296072506324 ) ) ;
#20469 = EDGE_CURVE ( 'NONE', #24563, #29552, #20626, .T. ) ;
#20468 = DIRECTION ( 'NONE',  ( 1.000000000000000000, 0.000000000000000000, -0.000000000000000000 ) ) ;
#20470 = ORIENTED_EDGE ( 'NONE', *, *, #26720, .T. ) ;
#20471 = B_SPLINE_CURVE_WITH_KNOTS ( 'NONE', 3,
 ( #2162, #24016, #26719, #28775, #5011, #11825, #2491, #29382, #7694, #14195, #19287, #23869, #16897, #21500, #16748, #26392, #4692, #26539, #2321 ),
 .UNSPECIFIED., .F., .F.,
 ( 4, 3, 3, 3, 3, 3, 4 ),
 ( 0.000000000000000000, 1.379880695094091716E-05, 1.586212677361243252E-05, 3.248035412973974761E-05, 5.074149073291455770E-05, 7.133938104856671239E-05, 9.012192312893275124E-05 ),
 .UNSPECIFIED. ) ;
#20472 = CARTESIAN_POINT ( 'NONE',  ( 53.05468381831884273, 8.377149132718326285, 2.049999999999815081 ) ) ;
#20473 = CARTESIAN_POINT ( 'NONE',  ( -60.60075002049966031, -2.435642456719447679, -1.068919490937977113 ) ) ;
#20474 = ORIENTED_EDGE ( 'NONE', *, *, #16268, .F. ) ;
#20475 = AXIS2_PLACEMENT_3D ( 'NONE', #11978, #21665, #16585 ) ;
#20476 = FACE_OUTER_BOUND ( 'NONE', #14062, .T. ) ;
#20477 = ORIENTED_EDGE ( 'NONE', *, *, #248, .T. ) ;
#20478 = CARTESIAN_POINT ( 'NONE',  ( 44.98443556292537693, -3.726179070414207928, -1.100000000000000089 ) ) ;
#20479 = CARTESIAN_POINT ( 'NONE',  ( 51.49472959044964426, 1.070956530528826889, -1.224612562803248483 ) ) ;
#20480 = EDGE_LOOP ( 'NONE', ( #4166, #9212, #11008, #14803 ) ) ;
#20481 = CARTESIAN_POINT ( 'NONE',  ( 52.00295751487188767, 4.370849658658843673, -1.433798655470523986 ) ) ;
#20482 = CARTESIAN_POINT ( 'NONE',  ( -56.39405989232412253, 2.944486372867106461, -1.700000000000187583 ) ) ;
#20483 = VERTEX_POINT ( 'NONE', #9206 ) ;
#20484 = CARTESIAN_POINT ( 'NONE',  ( 57.05000000000001847, 0.7794871794871796045, -1.732743413496389939 ) ) ;
#20485 = ORIENTED_EDGE ( 'NONE', *, *, #23340, .F. ) ;
#20486 = ORIENTED_EDGE ( 'NONE', *, *, #13713, .F. ) ;
#20487 = CARTESIAN_POINT ( 'NONE',  ( -58.49999999999997868, -2.944486372867089141, 1.699999999999781242 ) ) ;
#20488 = CARTESIAN_POINT ( 'NONE',  ( 61.00000000000001421, 0.8666666666673057406, 1.374595900215364930 ) ) ;
#20489 = CARTESIAN_POINT ( 'NONE',  ( -44.49999999999997868, -2.649999999999991918, -1.682353447508856999E-13 ) ) ;
#20490 = DIRECTION ( 'NONE',  ( 0.000000000000000000, 0.000000000000000000, -1.000000000000000000 ) ) ;
#20491 = MECHANICAL_DESIGN_GEOMETRIC_PRESENTATION_REPRESENTATION (  '', ( #26026 ), #1740 ) ;
#20492 = EDGE_CURVE ( 'NONE', #11981, #22245, #16347, .T. ) ;
#20493 = AXIS2_PLACEMENT_3D ( 'NONE', #15623, #3584, #22904 ) ;
#20494 = FACE_OUTER_BOUND ( 'NONE', #21990, .T. ) ;
#20495 = EDGE_CURVE ( 'NONE', #22739, #6559, #26960, .T. ) ;
#20496 = CARTESIAN_POINT ( 'NONE',  ( -56.97085481156723574, 1.184343223768591136, 3.558065644182727194 ) ) ;
#20497 = AXIS2_PLACEMENT_3D ( 'NONE', #27931, #25717, #23037 ) ;
#20498 = DIRECTION ( 'NONE',  ( 1.000000000000000000, -1.219044193948983948E-29, 3.491481338843133355E-15 ) ) ;
#20499 = CARTESIAN_POINT ( 'NONE',  ( -64.29999999999996874, 4.961699865966959239E-16, 2.647079050581693988E-15 ) ) ;
#20500 = DIRECTION ( 'NONE',  ( 1.000000000000000000, 0.000000000000000000, -0.000000000000000000 ) ) ;
#20501 = B_SPLINE_CURVE_WITH_KNOTS ( 'NONE', 3,
 ( #22792, #11525, #11343, #21028, #2163, #16271, #16598, #26074, #21201, #4694, #11826, #14035, #30667, #30833, #9303, #11679, #16751, #4385, #18967 ),
 .UNSPECIFIED., .F., .F.,
 ( 4, 3, 3, 3, 3, 3, 4 ),
 ( -1.485273975135215818E-06, 0.000000000000000000, 2.074191569004179043E-05, 3.882553518188196033E-05, 5.450508821808581838E-05, 6.929665250580413082E-05, 8.415228772525333491E-05 ),
 .UNSPECIFIED. ) ;
#20502 = CARTESIAN_POINT ( 'NONE',  ( 58.65000038048046349, 1.265626441015807568, -1.383507098107855438 ) ) ;
#20503 = FACE_OUTER_BOUND ( 'NONE', #29836, .T. ) ;
#20504 = AXIS2_PLACEMENT_3D ( 'NONE', #10497, #2738, #3199 ) ;
#20505 = ORIENTED_EDGE ( 'NONE', *, *, #7528, .T. ) ;
#20506 = DIRECTION ( 'NONE',  ( 1.000000000000000000, 0.000000000000000000, 0.000000000000000000 ) ) ;
#20507 = ADVANCED_FACE ( 'NONE', ( #8706 ), #20917, .T. ) ;
#20508 = CARTESIAN_POINT ( 'NONE',  ( 58.66107449606931823, -0.9668599424569509493, 1.606832818401507490 ) ) ;
#20509 = ORIENTED_EDGE ( 'NONE', *, *, #16163, .F. ) ;
#20510 = ORIENTED_EDGE ( 'NONE', *, *, #8640, .T. ) ;
#20511 = SURFACE_SIDE_STYLE ('',( #13660 ) ) ;
#20512 = DIRECTION ( 'NONE',  ( 1.000000000000000000, 0.000000000000000000, 0.000000000000000000 ) ) ;
#20514 = CARTESIAN_POINT ( 'NONE',  ( -59.60960479401909851, 2.008809929642550784, 1.728346801590697757 ) ) ;
#20513 = CARTESIAN_POINT ( 'NONE',  ( -55.62499999999998579, -3.920666489018346722E-15, 3.399999999999801403 ) ) ;
#20515 = ORIENTED_EDGE ( 'NONE', *, *, #5877, .T. ) ;
#20516 = VERTEX_POINT ( 'NONE', #1735 ) ;
#20517 = CIRCLE ( 'NONE', #11379, 159.6997717543496833 ) ;
#20518 = DIRECTION ( 'NONE',  ( 1.000000000000000000, -1.219044193948983948E-29, 3.491481338843133355E-15 ) ) ;
#20519 = VERTEX_POINT ( 'NONE', #13922 ) ;
#20520 = AXIS2_PLACEMENT_3D ( 'NONE', #18592, #14133, #28239 ) ;
#20521 = DIRECTION ( 'NONE',  ( 3.083952846180964840E-15, 0.000000000000000000, 1.000000000000000000 ) ) ;
#20522 = VERTEX_POINT ( 'NONE', #25817 ) ;
#20523 = CARTESIAN_POINT ( 'NONE',  ( 25.06719628372713160, 5.330953183978783372, -1.950000000000088107 ) ) ;
#20524 = DIRECTION ( 'NONE',  ( 0.000000000000000000, 0.000000000000000000, 1.000000000000000000 ) ) ;
#20525 = CARTESIAN_POINT ( 'NONE',  ( 47.10000000000003695, -3.609862487194767322, 1.947526779790813123 ) ) ;
#20526 = CARTESIAN_POINT ( 'NONE',  ( 47.03773326306244940, -4.256154442720823994, -1.015631899367381408 ) ) ;
#20527 = CIRCLE ( 'NONE', #1774, 2.100000000000000089 ) ;
#20528 = CARTESIAN_POINT ( 'NONE',  ( -59.70655989232412253, -3.925981830489445379, -2.260242286469037332E-13 ) ) ;
#20529 = CARTESIAN_POINT ( 'NONE',  ( 47.00000000000002842, -3.637377585518695611, 2.099877210782872705 ) ) ;
#20530 = EDGE_CURVE ( 'NONE', #28052, #21195, #13037, .T. ) ;
#20531 = CARTESIAN_POINT ( 'NONE',  ( -59.29999999999997584, 2.330309927981285032E-15, 4.253626757584724400E-16 ) ) ;
#20532 = EDGE_CURVE ( 'NONE', #1037, #28412, #14230, .T. ) ;
#20533 = DIRECTION ( 'NONE',  ( -1.000000000000000000, -3.054025858079668409E-16, 2.042474015755241579E-16 ) ) ;
#20534 = EDGE_CURVE ( 'NONE', #2594, #6393, #28986, .T. ) ;
#20535 = DIRECTION ( 'NONE',  ( -3.489354422748178977E-15, 1.218509414717996338E-16, -1.000000000000000000 ) ) ;
#20537 = CARTESIAN_POINT ( 'NONE',  ( 51.14630318392407560, -0.9364487020629673752, -1.503522130792586564 ) ) ;
#20536 = DIRECTION ( 'NONE',  ( 2.581436205204234499E-16, -0.9796124928211140670, -0.2008964009354146651 ) ) ;
#20538 = CIRCLE ( 'NONE', #9409, 4.275000000000000355 ) ;
#20539 = DIRECTION ( 'NONE',  ( 0.000000000000000000, 0.000000000000000000, -1.000000000000000000 ) ) ;
#20540 = CIRCLE ( 'NONE', #17493, 1.899999999999999911 ) ;
#20541 = DIRECTION ( 'NONE',  ( -0.000000000000000000, -0.000000000000000000, 1.000000000000000000 ) ) ;
#20542 = CARTESIAN_POINT ( 'NONE',  ( 51.40674769956039114, -0.9873535814794003329, 1.422142864483648461 ) ) ;
#20543 = EDGE_LOOP ( 'NONE', ( #21415, #26194, #7027, #25896 ) ) ;
#20544 = AXIS2_PLACEMENT_3D ( 'NONE', #11835, #12290, #31149 ) ;
#20545 = CARTESIAN_POINT ( 'NONE',  ( 54.44772160268976791, 6.353385485843105585, 1.624999999999810374 ) ) ;
#20546 = AXIS2_PLACEMENT_3D ( 'NONE', #1943, #11754, #11436 ) ;
#20547 = ORIENTED_EDGE ( 'NONE', *, *, #27619, .F. ) ;
#20548 = EDGE_CURVE ( 'NONE', #9481, #20395, #24074, .T. ) ;
#20549 = CARTESIAN_POINT ( 'NONE',  ( -59.65261300033996150, -3.078803759524879613, -1.467355461969038100 ) ) ;
#20550 =( BOUNDED_SURFACE ( )  B_SPLINE_SURFACE ( 3, 2, ( 
 ( #24651, #270, #2964 ),
 ( #7855, #29540, #2657 ),
 ( #7565, #17225, #12609 ),
 ( #15147, #5805, #23485 ),
 ( #10708, #9245, #28397 ),
 ( #22605, #30013, #6551 ),
 ( #11616, #13656, #30771 ),
 ( #24947, #13965, #25860 ) ),
 .UNSPECIFIED., .F., .F., .F. ) 
 B_SPLINE_SURFACE_WITH_KNOTS ( ( 4, 2, 2, 4 ),
 ( 3, 3 ),
 ( 0.001762834131042892915, 0.001945267826973966826, 0.002127701522905040520, 0.002492568914767187907 ),
 ( 0.000000000000000000, 1.000000000000000000 ),
 .UNSPECIFIED. ) 
 GEOMETRIC_REPRESENTATION_ITEM ( )  RATIONAL_B_SPLINE_SURFACE ( (
 ( 1.000000000000000000, 0.8699658093904940603, 1.000000000000000000),
 ( 1.000000000000000000, 0.8851796357839156748, 1.000000000000000000),
 ( 1.000000000000000000, 0.8977447492167196508, 1.000000000000000000),
 ( 1.000000000000000000, 0.9127836411835481556, 1.000000000000000000),
 ( 1.000000000000000000, 0.9151168517135812586, 1.000000000000000000),
 ( 1.000000000000000000, 0.9045976586032163924, 1.000000000000000000),
 ( 1.000000000000000000, 0.8745315534097299892, 1.000000000000000000),
 ( 1.000000000000000000, 0.8388746406931726352, 1.000000000000000000) ) ) 
 REPRESENTATION_ITEM ( '' )  SURFACE ( )  );
#20551 = ORIENTED_EDGE ( 'NONE', *, *, #5530, .T. ) ;
#20552 = CARTESIAN_POINT ( 'NONE',  ( 51.75611399313425665, 4.330462468336024884, 1.549999999999819300 ) ) ;
#20553 = CARTESIAN_POINT ( 'NONE',  ( -35.85663232820592583, -5.086913985776160274, 1.171642053949097262 ) ) ;
#20555 = CARTESIAN_POINT ( 'NONE',  ( 58.75000000000000711, 1.960427193528545109, 0.3958853607757182314 ) ) ;
#20554 = PLANE ( 'NONE',  #15019 ) ;
#20556 = ORIENTED_EDGE ( 'NONE', *, *, #28959, .F. ) ;
#20557 = DIRECTION ( 'NONE',  ( 3.489354422748178582E-15, -1.218509414717996338E-16, 1.000000000000000000 ) ) ;
#20558 = CARTESIAN_POINT ( 'NONE',  ( -61.34999999999997300, -2.515554072771550853, -0.7899129066418597578 ) ) ;
#20559 = AXIS2_PLACEMENT_3D ( 'NONE', #18938, #28580, #6892 ) ;
#20560 = ORIENTED_EDGE ( 'NONE', *, *, #1688, .F. ) ;
#20562 = DIRECTION ( 'NONE',  ( -1.000000000000000000, 1.219044193948983948E-29, -3.491481338843133355E-15 ) ) ;
#20561 = CARTESIAN_POINT ( 'NONE',  ( 50.29999999999825633, 1.391941090720882235, 3.849999999997240074 ) ) ;
#20563 = CYLINDRICAL_SURFACE ( 'NONE', #18527, 0.09999999999999982514 ) ;
#20564 = ORIENTED_EDGE ( 'NONE', *, *, #21330, .F. ) ;
#20565 = CARTESIAN_POINT ( 'NONE',  ( -36.22955757456081471, 4.863043649742752272, -1.860644097022596588 ) ) ;
#20566 = VECTOR ( 'NONE', #27258, 1000.000000000000000 ) ;
#20567 = CARTESIAN_POINT ( 'NONE',  ( -54.64405989232413674, -3.920666489018357767E-15, 3.399999999999804512 ) ) ;
#20568 = CARTESIAN_POINT ( 'NONE',  ( -35.85663232820584057, -2.199885893005967041, 4.939696249117680793 ) ) ;
#20569 = AXIS2_PLACEMENT_3D ( 'NONE', #28064, #10983, #858 ) ;
#20570 = CARTESIAN_POINT ( 'NONE',  ( 47.10000000000002274, -4.259181259350203419, 0.9999999999999995559 ) ) ;
#20571 = CARTESIAN_POINT ( 'NONE',  ( 57.00000000000001421, 0.6999999999999999556, -1.820027472320129736 ) ) ;
#20572 = CIRCLE ( 'NONE', #10446, 1.302039949377232331 ) ;
#20573 = ORIENTED_EDGE ( 'NONE', *, *, #23358, .T. ) ;
#20574 = CIRCLE ( 'NONE', #27125, 2.000000000000000000 ) ;
#20575 = EDGE_CURVE ( 'NONE', #14583, #3014, #2192, .T. ) ;
#20576 = CIRCLE ( 'NONE', #7400, 0.2000000000000000944 ) ;
#20577 = CARTESIAN_POINT ( 'NONE',  ( 15.29384114148384022, 2.734418404389609147, 4.440882220947752757 ) ) ;
#20578 = CARTESIAN_POINT ( 'NONE',  ( -60.59999999999997300, -2.481395594095113122, 0.9440358133373861760 ) ) ;
#20579 = CARTESIAN_POINT ( 'NONE',  ( 47.00000000000002132, -3.826179070414207573, -1.000000000000000000 ) ) ;
#20580 = AXIS2_PLACEMENT_3D ( 'NONE', #22268, #24170, #2937 ) ;
#20581 = AXIS2_PLACEMENT_3D ( 'NONE', #20624, #15998, #6049 ) ;
#20582 = CARTESIAN_POINT ( 'NONE',  ( -57.88452994616205416, 3.117691453623976816, 1.799999999999811973 ) ) ;
#20583 = AXIS2_PLACEMENT_3D ( 'NONE', #18755, #15458, #6701 ) ;
#20584 = CARTESIAN_POINT ( 'NONE',  ( 58.73371041428939066, -1.873417296527896792, -0.08026432063101406056 ) ) ;
#20585 = CARTESIAN_POINT ( 'NONE',  ( 48.46185180831791683, 1.426738236278596972, -3.843750512866276559 ) ) ;
#20586 = EDGE_LOOP ( 'NONE', ( #15463, #15865, #14650, #6821 ) ) ;
#20587 = EDGE_CURVE ( 'NONE', #24526, #585, #19342, .T. ) ;
#20588 = CARTESIAN_POINT ( 'NONE',  ( 58.73371041428912775, 1.582294810367057547, 1.006219588949640364 ) ) ;
#20589 = AXIS2_PLACEMENT_3D ( 'NONE', #8858, #18550, #21255 ) ;
#20590 = VERTEX_POINT ( 'NONE', #19022 ) ;
#20591 = CARTESIAN_POINT ( 'NONE',  ( -59.19495429951913223, 2.548385458854359964, -0.9469503383365888149 ) ) ;
#20593 = CARTESIAN_POINT ( 'NONE',  ( 48.30000000000001847, 2.428612866367529932E-14, -4.100000000000022737 ) ) ;
#20592 = CARTESIAN_POINT ( 'NONE',  ( -60.64999999999998437, 1.610824598944129570E-15, 1.901562740512771401E-15 ) ) ;
#20594 = CIRCLE ( 'NONE', #11464, 0.09999999999999992228 ) ;
#20595 = ORIENTED_EDGE ( 'NONE', *, *, #10551, .F. ) ;
#20596 = ORIENTED_EDGE ( 'NONE', *, *, #8315, .T. ) ;
#20597 = FACE_OUTER_BOUND ( 'NONE', #12574, .T. ) ;
#20598 = CIRCLE ( 'NONE', #28674, 160.1997717543138720 ) ;
#20599 = DIRECTION ( 'NONE',  ( 1.000000000000000000, -0.000000000000000000, -0.000000000000000000 ) ) ;
#20600 = CIRCLE ( 'NONE', #24109, 0.05000000000000012768 ) ;
#20602 = DIRECTION ( 'NONE',  ( -3.489354422748178582E-15, 1.218509414717996338E-16, -1.000000000000000000 ) ) ;
#20601 = CARTESIAN_POINT ( 'NONE',  ( -60.38452994616202574, 2.093608279459374244E-14, -3.600000000000214140 ) ) ;
#20603 = AXIS2_PLACEMENT_3D ( 'NONE', #15448, #25099, #20380 ) ;
#20604 = CARTESIAN_POINT ( 'NONE',  ( -55.98542740578361077, 0.7887156198831667409, -3.845940847736174728 ) ) ;
#20605 = CARTESIAN_POINT ( 'NONE',  ( -60.24999999999997868, 2.040177471463716435E-15, 6.193977072552205884E-16 ) ) ;
#20606 = CARTESIAN_POINT ( 'NONE',  ( 53.31624996668935523, 4.986115460562799306, -1.613809080173747912 ) ) ;
#20607 = AXIS2_PLACEMENT_3D ( 'NONE', #19352, #14414, #3862 ) ;
#20608 = ORIENTED_EDGE ( 'NONE', *, *, #22984, .T. ) ;
#20609 = AXIS2_PLACEMENT_3D ( 'NONE', #20084, #14992, #14692 ) ;
#20610 = ADVANCED_FACE ( 'NONE', ( #31035 ), #5071, .T. ) ;
#20611 = CARTESIAN_POINT ( 'NONE',  ( 47.03912372675481635, -4.170474612306438011, -1.019817338724548605 ) ) ;
#20612 = AXIS2_PLACEMENT_3D ( 'NONE', #13575, #3935, #4236 ) ;
#20613 = CARTESIAN_POINT ( 'NONE',  ( 53.34494210428216121, 4.987020249080381440, -2.050000000000185896 ) ) ;
#20614 = CARTESIAN_POINT ( 'NONE',  ( 58.75000000000003553, -1.996089927834302724, 0.1250000000000018041 ) ) ;
#20615 = CARTESIAN_POINT ( 'NONE',  ( 15.41217651307625047, -0.2668145608218825959, 5.199999998579027505 ) ) ;
#20616 = CARTESIAN_POINT ( 'NONE',  ( 47.10000000000002274, 6.982261990806648555E-14, -1.632474749424821370E-13 ) ) ;
#20617 = AXIS2_PLACEMENT_3D ( 'NONE', #22923, #5508, #20251 ) ;
#20618 = AXIS2_PLACEMENT_3D ( 'NONE', #16835, #2720, #10157 ) ;
#20620 = CARTESIAN_POINT ( 'NONE',  ( -36.22909104983143180, 0.6969927240739536289, -5.374332520738267505 ) ) ;
#20619 = DIRECTION ( 'NONE',  ( 1.000000000000000000, 3.385297212316223527E-16, 2.459562394685754633E-16 ) ) ;
#20621 = CIRCLE ( 'NONE', #21652, 4.700000000000000178 ) ;
#20622 = DIRECTION ( 'NONE',  ( -1.000000000000000000, -3.054025858079668409E-16, 2.042474015755241579E-16 ) ) ;
#20624 = CARTESIAN_POINT ( 'NONE',  ( 69.23535533905935324, 4.557543281186736018E-17, -7.252018534634969470E-13 ) ) ;
#20623 = CARTESIAN_POINT ( 'NONE',  ( 69.20000000000001705, -0.7500000000000000000, -1.988246715074081017 ) ) ;
#20625 = EDGE_LOOP ( 'NONE', ( #12106, #15043, #13934, #10635, #22912, #18635, #17427, #19890, #6170 ) ) ;
#20626 = LINE ( 'NONE', #4274, #17872 ) ;
#20627 = CARTESIAN_POINT ( 'NONE',  ( -44.59999999999998721, 1.499999999999996003, 3.959797974644454488 ) ) ;
#20628 = AXIS2_PLACEMENT_3D ( 'NONE', #15317, #8344, #8509 ) ;
#20630 = CARTESIAN_POINT ( 'NONE',  ( -59.65728261716281366, -2.366782727822243526, -1.230152085140890916 ) ) ;
#20629 = DIRECTION ( 'NONE',  ( -0.9993908270190956511, 0.03489949670250096919, 3.491481338843132961E-15 ) ) ;
#20631 = DIRECTION ( 'NONE',  ( 0.000000000000000000, 1.532429380227459806E-15, -1.000000000000000000 ) ) ;
#20632 = ORIENTED_EDGE ( 'NONE', *, *, #21461, .F. ) ;
#20633 = DIRECTION ( 'NONE',  ( 0.000000000000000000, 0.000000000000000000, 1.000000000000000000 ) ) ;
#20634 = CARTESIAN_POINT ( 'NONE',  ( -60.60214168571716442, -2.439458054579491719, -1.071672411231956223 ) ) ;
#20635 = CIRCLE ( 'NONE', #29210, 0.04999999999999989175 ) ;
#20636 = EDGE_LOOP ( 'NONE', ( #478, #3292, #7219, #19580 ) ) ;
#20637 = DIRECTION ( 'NONE',  ( 0.000000000000000000, 0.000000000000000000, 1.000000000000000000 ) ) ;
#20638 = ADVANCED_FACE ( 'NONE', ( #4742 ), #18696, .F. ) ;
#20639 = VERTEX_POINT ( 'NONE', #26600 ) ;
#20640 = DIRECTION ( 'NONE',  ( 0.000000000000000000, -0.3529411764705844834, 0.9356455129756994227 ) ) ;
#20641 = CARTESIAN_POINT ( 'NONE',  ( 48.00000000000001421, -4.387164041431065975, -1.383037119376926194 ) ) ;
#20642 = ORIENTED_EDGE ( 'NONE', *, *, #28568, .F. ) ;
#20643 = SURFACE_STYLE_USAGE ( .BOTH. , #8577 ) ;
#20644 = CARTESIAN_POINT ( 'NONE',  ( -56.19702994616206837, -2.078460969082662757, 3.599999999999788702 ) ) ;
#20645 = AXIS2_PLACEMENT_3D ( 'NONE', #10368, #6102, #22273 ) ;
#20646 = CARTESIAN_POINT ( 'NONE',  ( -57.51905989232412963, -2.944486372867088697, 1.699999999999784350 ) ) ;
#20647 = ORIENTED_EDGE ( 'NONE', *, *, #3003, .T. ) ;
#20648 = EDGE_LOOP ( 'NONE', ( #12343, #665, #16862 ) ) ;
#20649 = EDGE_LOOP ( 'NONE', ( #6016, #14094, #18210, #23211 ) ) ;
#20650 = EDGE_CURVE ( 'NONE', #27496, #20928, #2532, .T. ) ;
#20651 = CARTESIAN_POINT ( 'NONE',  ( -58.12499999999996447, 2.944486372867106905, -1.700000000000193801 ) ) ;
#20652 = EDGE_CURVE ( 'NONE', #14026, #22708, #4198, .T. ) ;
#20653 = DIRECTION ( 'NONE',  ( 2.614375865348241018E-16, -0.2008964009354148039, 0.9796124928211140670 ) ) ;
#20654 = CARTESIAN_POINT ( 'NONE',  ( 58.64999999999999858, 1.656030381686821151, 0.8799718970829721876 ) ) ;
#20656 = EDGE_CURVE ( 'NONE', #30388, #28184, #2217, .T. ) ;
#20655 = PLANE ( 'NONE',  #7397 ) ;
#20657 = CARTESIAN_POINT ( 'NONE',  ( -59.69999999999997442, 8.366749974758454467E-15, -2.120534355533670266E-13 ) ) ;
#20658 = AXIS2_PLACEMENT_3D ( 'NONE', #18153, #1040, #8308 ) ;
#20660 = CYLINDRICAL_SURFACE ( 'NONE', #25000, 1.625000000000000222 ) ;
#20659 = DIRECTION ( 'NONE',  ( 1.000000000000000000, 3.054025858079668409E-16, -2.042474015755241579E-16 ) ) ;
#20661 = SURFACE_STYLE_FILL_AREA ( #10981 ) ;
#20662 = CARTESIAN_POINT ( 'NONE',  ( 50.93312545610842790, 0.6352506689595308620, 1.438808137080896055 ) ) ;
#20663 = FACE_OUTER_BOUND ( 'NONE', #19390, .T. ) ;
#20664 = CARTESIAN_POINT ( 'NONE',  ( 58.73379417893117704, -1.662624490946059241, -0.8670685180647094148 ) ) ;
#20665 = ADVANCED_FACE ( 'NONE', ( #31204 ), #2388, .T. ) ;
#20666 = CARTESIAN_POINT ( 'NONE',  ( 53.14855870271264138, 8.298021504495151746, -2.050000000000184563 ) ) ;
#20667 = CARTESIAN_POINT ( 'NONE',  ( -59.29999999999998295, 2.783937418660473728, 2.481186825065970769 ) ) ;
#20668 = ORIENTED_EDGE ( 'NONE', *, *, #26816, .T. ) ;
#20669 = CARTESIAN_POINT ( 'NONE',  ( -54.49999999999999289, -3.325675108906214206, 0.8689164811911511688 ) ) ;
#20670 = DIRECTION ( 'NONE',  ( 1.047444401652940007E-14, 0.000000000000000000, 1.000000000000000000 ) ) ;
#20671 = ORIENTED_EDGE ( 'NONE', *, *, #11865, .F. ) ;
#20672 = CARTESIAN_POINT ( 'NONE',  ( 51.80000000000001137, 3.850000000000016520, -2.050000000000180123 ) ) ;
#20673 = DIRECTION ( 'NONE',  ( -1.000000000000000000, -3.053848253006669023E-16, 2.042510438544995415E-16 ) ) ;
#20675 = CARTESIAN_POINT ( 'NONE',  ( -61.39919102937896156, -2.604635884043592586, 0.7112281530754581693 ) ) ;
#20674 = CARTESIAN_POINT ( 'NONE',  ( -55.74999999999997868, 2.944486372867092250, 1.699999999999813438 ) ) ;
#20676 = ORIENTED_EDGE ( 'NONE', *, *, #13274, .F. ) ;
#20677 = ADVANCED_FACE ( 'NONE', ( #24525 ), #17884, .F. ) ;
#20678 = ORIENTED_EDGE ( 'NONE', *, *, #12535, .T. ) ;
#20679 = AXIS2_PLACEMENT_3D ( 'NONE', #6512, #16170, #25818 ) ;
#20680 = CYLINDRICAL_SURFACE ( 'NONE', #12893, 3.625000000000024869 ) ;
#20681 = PRESENTATION_LAYER_ASSIGNMENT (  '', '', ( #22192 ) ) ;
#20682 = ORIENTED_EDGE ( 'NONE', *, *, #27975, .T. ) ;
#20683 = CARTESIAN_POINT ( 'NONE',  ( -35.85663232820584057, -2.686240680702168593, 4.475885388010719446 ) ) ;
#20684 = ORIENTED_EDGE ( 'NONE', *, *, #24446, .F. ) ;
#20685 = CARTESIAN_POINT ( 'NONE',  ( 22.32354329421558958, 7.018810582754777982, -2.050000000000010036 ) ) ;
#20686 = ADVANCED_FACE ( 'NONE', ( #10601 ), #3154, .F. ) ;
#20687 = CARTESIAN_POINT ( 'NONE',  ( 61.25000000000002132, 6.415596960124259844E-13, 3.111507638930570854E-58 ) ) ;
#20688 = DIRECTION ( 'NONE',  ( -1.000000000000000000, -0.000000000000000000, 3.491481338843133355E-15 ) ) ;
#20689 = ORIENTED_EDGE ( 'NONE', *, *, #20359, .T. ) ;
#20690 = CARTESIAN_POINT ( 'NONE',  ( 46.90000000000002700, -4.227689052994015206, -1.125730994152046138 ) ) ;
#20691 = EDGE_CURVE ( 'NONE', #2745, #27904, #2696, .T. ) ;
#20692 = LINE ( 'NONE', #8767, #10886 ) ;
#20693 = CARTESIAN_POINT ( 'NONE',  ( 51.32247534403771994, -1.004558583830394314, 1.391720660572748791 ) ) ;
#20695 = EDGE_CURVE ( 'NONE', #8146, #16115, #20734, .T. ) ;
#20694 = CARTESIAN_POINT ( 'NONE',  ( 48.00000000000001421, -3.937842575352406005, 1.145831896685653328 ) ) ;
#20696 = CARTESIAN_POINT ( 'NONE',  ( 58.72427158855725793, 1.357477749119627264, 1.293556822995691302 ) ) ;
#20697 = CARTESIAN_POINT ( 'NONE',  ( 51.59739104186227365, 1.010292945603182169, 1.272765950230260401 ) ) ;
#20698 = CARTESIAN_POINT ( 'NONE',  ( 57.00529107662529782, 0.7231510886217332734, -1.801575813826951533 ) ) ;
#20700 = DIRECTION ( 'NONE',  ( 1.000000000000000000, 0.000000000000000000, -1.047444401652940007E-14 ) ) ;
#20699 = CARTESIAN_POINT ( 'NONE',  ( -60.87073935753531373, -2.544307234692274378, 0.9096008698628265110 ) ) ;
#20701 = CARTESIAN_POINT ( 'NONE',  ( 56.95000000000001705, 0.7000000000000000666, 2.452039967047845437 ) ) ;
#20702 = VECTOR ( 'NONE', #25458, 1000.000000000000000 ) ;
#20703 =( BOUNDED_CURVE ( )  B_SPLINE_CURVE ( 3, ( #30282, #28229, #30431, #6079 ),
 .UNSPECIFIED., .F., .T. ) 
 B_SPLINE_CURVE_WITH_KNOTS ( ( 4, 4 ),
 ( 5.208023207023585677, 5.331808265806120772 ),
 .UNSPECIFIED. ) 
 CURVE ( )  GEOMETRIC_REPRESENTATION_ITEM ( )  RATIONAL_B_SPLINE_CURVE ( ( 1.000000000000000000, 0.9987235124983906420, 0.9987235124983906420, 1.000000000000000000 ) ) 
 REPRESENTATION_ITEM ( '' )  );
#20704 = ORIENTED_EDGE ( 'NONE', *, *, #3963, .F. ) ;
#20705 = CARTESIAN_POINT ( 'NONE',  ( 54.16356081880782369, 5.682032782862182607, -2.050000000000188116 ) ) ;
#20706 = VERTEX_POINT ( 'NONE', #13120 ) ;
#20707 = CARTESIAN_POINT ( 'NONE',  ( -59.18666126818025930, -2.395858435315754154, 1.242435404725767523 ) ) ;
#20708 = VERTEX_POINT ( 'NONE', #15504 ) ;
#20709 = CARTESIAN_POINT ( 'NONE',  ( 51.80000000000002558, 8.700000000000107647, 2.049999999999819522 ) ) ;
#20710 = CARTESIAN_POINT ( 'NONE',  ( -59.03335481156722864, -4.108500314926510022, 1.367561758111407899 ) ) ;
#20711 = CIRCLE ( 'NONE', #986, 0.1000000000000000472 ) ;
#20713 = DIRECTION ( 'NONE',  ( 0.000000000000000000, -0.1576190026614809614, -0.9875000000000001554 ) ) ;
#20712 = DIRECTION ( 'NONE',  ( -1.000000000000000000, 1.219044193948984088E-29, -3.491481338843133750E-15 ) ) ;
#20714 = ORIENTED_EDGE ( 'NONE', *, *, #5955, .F. ) ;
#20715 = ADVANCED_FACE ( 'NONE', ( #949 ), #10439, .F. ) ;
#20716 = ORIENTED_EDGE ( 'NONE', *, *, #10120, .F. ) ;
#20717 = CARTESIAN_POINT ( 'NONE',  ( 30.93632708544912902, 7.271619894357248093, -2.050000000000106848 ) ) ;
#20718 = EDGE_CURVE ( 'NONE', #12947, #21492, #11285, .T. ) ;
#20719 = DIRECTION ( 'NONE',  ( 2.117927888850091331E-16, -0.02490330187381135929, 0.9996898646859343485 ) ) ;
#20720 = ORIENTED_EDGE ( 'NONE', *, *, #12866, .F. ) ;
#20721 = SPHERICAL_SURFACE ( 'NONE', #2917, 0.1000000000000000056 ) ;
#20722 = EDGE_CURVE ( 'NONE', #7502, #16804, #13286, .T. ) ;
#20723 = FACE_OUTER_BOUND ( 'NONE', #24575, .T. ) ;
#20724 = ORIENTED_EDGE ( 'NONE', *, *, #16828, .F. ) ;
#20725 = CARTESIAN_POINT ( 'NONE',  ( -36.31440869660545445, 4.962395293451402623, -1.554871187131892318 ) ) ;
#20726 = DIRECTION ( 'NONE',  ( 1.000000000000000000, -1.219044193948983948E-29, 3.491481338843133355E-15 ) ) ;
#20727 = AXIS2_PLACEMENT_3D ( 'NONE', #27069, #17753, #12513 ) ;
#20728 = AXIS2_PLACEMENT_3D ( 'NONE', #19800, #29434, #169 ) ;
#20729 = SURFACE_STYLE_USAGE ( .BOTH. , #11199 ) ;
#20730 = CARTESIAN_POINT ( 'NONE',  ( -35.85663232820584767, 4.383220986679566167, 0.4611378927910952386 ) ) ;
#20731 = CARTESIAN_POINT ( 'NONE',  ( 61.25000000000001421, 1.039502773796357360, 1.800471618825331355 ) ) ;
#20732 = CARTESIAN_POINT ( 'NONE',  ( 15.41170998834775219, 3.722832355337220456, 3.938244298533839505 ) ) ;
#20733 = CARTESIAN_POINT ( 'NONE',  ( -57.79792740578359656, -2.256877952708268076, 2.542931754211920303 ) ) ;
#20734 =( BOUNDED_CURVE ( )  B_SPLINE_CURVE ( 2, ( #22475, #24985, #1095, #18049, #25162 ),
 .UNSPECIFIED., .F., .T. ) 
 B_SPLINE_CURVE_WITH_KNOTS ( ( 3, 2, 3 ),
 ( 0.000000000000000000, 0.01851851851851851749, 0.02777777777777778317 ),
 .UNSPECIFIED. ) 
 CURVE ( )  GEOMETRIC_REPRESENTATION_ITEM ( )  RATIONAL_B_SPLINE_CURVE ( ( 1.000000000000000000, 0.8660254037844387076, 1.000000000000000000, 0.9330127018922192983, 0.9330127018922194093 ) ) 
 REPRESENTATION_ITEM ( '' )  );
#20735 = CARTESIAN_POINT ( 'NONE',  ( -56.56684846062113081, -0.2309624077929025854, -3.875409454552791733 ) ) ;
#20736 = CARTESIAN_POINT ( 'NONE',  ( 54.41366571437520605, 6.718673005292168376, -1.950000000000180256 ) ) ;
#20737 = LINE ( 'NONE', #27372, #958 ) ;
#20738 = LINE ( 'NONE', #30848, #7961 ) ;
#20739 = VERTEX_POINT ( 'NONE', #12645 ) ;
#20740 = CIRCLE ( 'NONE', #2541, 0.09999999999999850675 ) ;
#20741 = VECTOR ( 'NONE', #5401, 1000.000000000000000 ) ;
#20742 = CYLINDRICAL_SURFACE ( 'NONE', #18384, 0.2500000000000002220 ) ;
#20743 = ORIENTED_EDGE ( 'NONE', *, *, #15872, .T. ) ;
#20744 = CARTESIAN_POINT ( 'NONE',  ( 51.80000000000001137, -4.387164041431065975, -1.383037119376939739 ) ) ;
#20746 = DIRECTION ( 'NONE',  ( 3.491481338843133355E-15, 0.000000000000000000, 1.000000000000000000 ) ) ;
#20745 = CARTESIAN_POINT ( 'NONE',  ( 48.40130545986176003, 0.9107929593200400076, 3.923749358243191043 ) ) ;
#20747 = ORIENTED_EDGE ( 'NONE', *, *, #23377, .T. ) ;
#20748 = EDGE_CURVE ( 'NONE', #20372, #2467, #19411, .T. ) ;
#20749 = VERTEX_POINT ( 'NONE', #22180 ) ;
#20750 = DIRECTION ( 'NONE',  ( 0.000000000000000000, 0.000000000000000000, -1.000000000000000000 ) ) ;
#20751 = CIRCLE ( 'NONE', #23255, 0.05000000000000012768 ) ;
#20752 = ADVANCED_FACE ( 'NONE', ( #3310 ), #10744, .T. ) ;
#20753 = CARTESIAN_POINT ( 'NONE',  ( 26.19155409318044292, 5.638511060912941630, 1.424999999999907896 ) ) ;
#20754 = DIRECTION ( 'NONE',  ( 0.9993908270190957621, -0.03489949670250202390, -3.491481338843133355E-15 ) ) ;
#20755 = ORIENTED_EDGE ( 'NONE', *, *, #6748, .F. ) ;
#20756 = CARTESIAN_POINT ( 'NONE',  ( -57.17292740578359656, 1.073804522883521795, 3.225979517392336682 ) ) ;
#20757 = CARTESIAN_POINT ( 'NONE',  ( 57.00000000000001421, -0.7500000000000000000, 2.421260002560649660 ) ) ;
#20758 = APPLICATION_PROTOCOL_DEFINITION ( 'draft international standard', 'automotive_design', 1998, #4728 ) ;
#20759 = FACE_OUTER_BOUND ( 'NONE', #19853, .T. ) ;
#20760 = AXIS2_PLACEMENT_3D ( 'NONE', #3712, #30790, #16381 ) ;
#20761 = ORIENTED_EDGE ( 'NONE', *, *, #22642, .T. ) ;
#20762 = B_SPLINE_CURVE_WITH_KNOTS ( 'NONE', 3,
 ( #1397, #23731, #13400, #2023 ),
 .UNSPECIFIED., .F., .F.,
 ( 4, 4 ),
 ( 0.000000000000000000, 0.0003111614939246246819 ),
 .UNSPECIFIED. ) ;
#20763 = ADVANCED_FACE ( 'NONE', ( #8070 ), #14327, .T. ) ;
#20764 = CARTESIAN_POINT ( 'NONE',  ( 47.05865997105815524, -4.175606900721715142, -1.008275291528680784 ) ) ;
#20765 = CARTESIAN_POINT ( 'NONE',  ( -36.80043232705877898, 2.728070298465809618, -4.669343935538267765 ) ) ;
#20766 = CARTESIAN_POINT ( 'NONE',  ( -59.36201654190949029, 3.300626201927056247, 1.250136525132569787 ) ) ;
#20767 = DIRECTION ( 'NONE',  ( 3.489354422748178582E-15, -1.218509414717996338E-16, 1.000000000000000000 ) ) ;
#20768 = VECTOR ( 'NONE', #18924, 1000.000000000000000 ) ;
#20769 = CARTESIAN_POINT ( 'NONE',  ( 61.25000000000004263, -1.470078920827180724, -1.470078920827526892 ) ) ;
#20771 = CYLINDRICAL_SURFACE ( 'NONE', #31114, 0.05000000000000012768 ) ;
#20770 = CARTESIAN_POINT ( 'NONE',  ( 58.75000000000000000, 2.079005547593415937, 1.004182178118534636E-12 ) ) ;
#20772 = DIRECTION ( 'NONE',  ( -1.000000000000000000, -2.586136946169074517E-16, 0.000000000000000000 ) ) ;
#20774 = CARTESIAN_POINT ( 'NONE',  ( -62.09999999999997300, -2.692057237979972317, -0.3088123856379243470 ) ) ;
#20773 = CARTESIAN_POINT ( 'NONE',  ( -59.24999999999997158, -2.944486372867095803, 1.699999999999767919 ) ) ;
#20775 = VERTEX_POINT ( 'NONE', #27695 ) ;
#20776 = CARTESIAN_POINT ( 'NONE',  ( -62.06507697720029171, -2.652888718249335032, -0.3385697102886689458 ) ) ;
#20777 = DIRECTION ( 'NONE',  ( 2.461451434200951079E-12, 0.4531102586349436967, -0.8914544820234930889 ) ) ;
#20778 = CARTESIAN_POINT ( 'NONE',  ( -59.96464466094062828, 2.127325729886550933E-15, 5.611146207266455330E-16 ) ) ;
#20779 = DIRECTION ( 'NONE',  ( 0.000000000000000000, 0.000000000000000000, 1.000000000000000000 ) ) ;
#20780 = ORIENTED_EDGE ( 'NONE', *, *, #8075, .T. ) ;
#20781 = CARTESIAN_POINT ( 'NONE',  ( 51.87767605783387381, 8.699351266148434902, 2.049999999999819522 ) ) ;
#20782 = DIRECTION ( 'NONE',  ( -1.293068473084537258E-16, 1.000000000000000000, 0.000000000000000000 ) ) ;
#20783 = EDGE_CURVE ( 'NONE', #6738, #20184, #12961, .T. ) ;
#20784 = ORIENTED_EDGE ( 'NONE', *, *, #21026, .F. ) ;
#20785 = FACE_OUTER_BOUND ( 'NONE', #27349, .T. ) ;
#20786 = ORIENTED_EDGE ( 'NONE', *, *, #23921, .T. ) ;
#20787 = CARTESIAN_POINT ( 'NONE',  ( 58.75000000000003553, -1.960427193528316847, -0.3958853607747112036 ) ) ;
#20788 = DIRECTION ( 'NONE',  ( 1.000000000000000000, -1.219044193948983948E-29, 3.491481338843133355E-15 ) ) ;
#20789 = ORIENTED_EDGE ( 'NONE', *, *, #20911, .T. ) ;
#20790 = SHAPE_REPRESENTATION_RELATIONSHIP ( 'NONE' , 'NONE' ,  #25673, #12322 ) ;
#20791 = CIRCLE ( 'NONE', #9150, 3.625000000000000444 ) ;
#20792 = CARTESIAN_POINT ( 'NONE',  ( 21.98769535799031161, 7.920638968848361827, 1.949999999999923794 ) ) ;
#20793 = CARTESIAN_POINT ( 'NONE',  ( -56.33155989232412253, 3.925981830489463142, -1.858639063162819723E-13 ) ) ;
#20794 = EDGE_LOOP ( 'NONE', ( #16303, #27124, #17128, #25755 ) ) ;
#20795 = CARTESIAN_POINT ( 'NONE',  ( 58.65000000000001990, 6.143261415694495821E-13, 3.111507638930570854E-58 ) ) ;
#20796 = ORIENTED_EDGE ( 'NONE', *, *, #30159, .F. ) ;
#20797 = ORIENTED_EDGE ( 'NONE', *, *, #28892, .T. ) ;
#20798 = CARTESIAN_POINT ( 'NONE',  ( -55.99999999999995737, 2.023778652682506212E-14, -3.400000000000199307 ) ) ;
#20799 = CARTESIAN_POINT ( 'NONE',  ( 58.66107449606971613, 1.606832818401695340, 0.9668599424582843271 ) ) ;
#20800 = DIRECTION ( 'NONE',  ( 0.000000000000000000, 0.000000000000000000, -1.000000000000000000 ) ) ;
#20801 = FACE_OUTER_BOUND ( 'NONE', #3982, .T. ) ;
#20803 = DIRECTION ( 'NONE',  ( 1.000000000000000000, 3.054027077731387480E-16, -2.042479963029832083E-16 ) ) ;
#20802 = CARTESIAN_POINT ( 'NONE',  ( 58.75000000000002132, 6.153735859711025284E-13, 3.111507638930570854E-58 ) ) ;
#20804 = CARTESIAN_POINT ( 'NONE',  ( -35.85663232820584057, 3.056483311920803025, 4.206888370749761741 ) ) ;
#20805 = CARTESIAN_POINT ( 'NONE',  ( -44.59999999999996589, -1.557046979865753356, -3.273565289175108362 ) ) ;
#20806 = CARTESIAN_POINT ( 'NONE',  ( 68.94999999999998863, 1.401298464324817071E-42, -4.000000000000722977 ) ) ;
#20807 = CARTESIAN_POINT ( 'NONE',  ( 58.72200624034172023, -1.612834625124900834, -0.9564954546388050316 ) ) ;
#20808 = CARTESIAN_POINT ( 'NONE',  ( 56.95000043478394502, 0.7674401070440159955, -2.484784916619714679 ) ) ;
#20809 = CARTESIAN_POINT ( 'NONE',  ( -59.29999999999999005, -1.394046907339186792, 3.175855595397861553 ) ) ;
#20810 = ORIENTED_EDGE ( 'NONE', *, *, #20017, .T. ) ;
#20811 = CARTESIAN_POINT ( 'NONE',  ( -54.49999999999999289, -3.459683327251550811, -0.6431504214706185163 ) ) ;
#20812 = CARTESIAN_POINT ( 'NONE',  ( 58.75000000000000711, 1.077297519405726156, -1.655311165516502925 ) ) ;
#20813 = EDGE_CURVE ( 'NONE', #4204, #25278, #27978, .T. ) ;
#20814 = ORIENTED_EDGE ( 'NONE', *, *, #29742, .T. ) ;
#20815 = SURFACE_STYLE_USAGE ( .BOTH. , #20511 ) ;
#20816 = CYLINDRICAL_SURFACE ( 'NONE', #1637, 2.125000000000043521 ) ;
#20818 = CARTESIAN_POINT ( 'NONE',  ( 50.50000000000002132, 2.428612866367529932E-14, 0.000000000000000000 ) ) ;
#20817 = CARTESIAN_POINT ( 'NONE',  ( -58.06249999999997158, 3.925981830489463142, -1.919074514008873212E-13 ) ) ;
#20819 = ADVANCED_FACE ( 'NONE', ( #617 ), #14817, .T. ) ;
#20820 = ORIENTED_EDGE ( 'NONE', *, *, #15478, .T. ) ;
#20821 = EDGE_LOOP ( 'NONE', ( #28694, #27234, #13503, #4884 ) ) ;
#20822 = CARTESIAN_POINT ( 'NONE',  ( 51.80000000000001137, -3.994701997234045177, -2.069753729861391722 ) ) ;
#20823 = ORIENTED_EDGE ( 'NONE', *, *, #19699, .F. ) ;
#20824 = FACE_OUTER_BOUND ( 'NONE', #27023, .T. ) ;
#20825 = AXIS2_PLACEMENT_3D ( 'NONE', #3752, #23092, #11200 ) ;
#20826 = DIRECTION ( 'NONE',  ( -1.000000000000000000, -0.000000000000000000, 1.047444401652940007E-14 ) ) ;
#20827 = ORIENTED_EDGE ( 'NONE', *, *, #14885, .F. ) ;
#20828 = CARTESIAN_POINT ( 'NONE',  ( 23.38809389355835933, 6.107120497888152144, -2.050000000000081091 ) ) ;
#20829 = LINE ( 'NONE', #18156, #13145 ) ;
#20830 = DIRECTION ( 'NONE',  ( 1.000000000000000000, 3.054025858079668409E-16, -2.042474015755241579E-16 ) ) ;
#20831 = VERTEX_POINT ( 'NONE', #10278 ) ;
#20832 = ADVANCED_FACE ( 'NONE', ( #7901 ), #275, .F. ) ;
#20833 = CARTESIAN_POINT ( 'NONE',  ( 49.04999999999999716, 3.214697847761800597E-16, -2.625000000000512923 ) ) ;
#20834 = DIRECTION ( 'NONE',  ( 0.000000000000000000, 0.000000000000000000, -1.000000000000000000 ) ) ;
#20835 = CARTESIAN_POINT ( 'NONE',  ( -44.49999999999999289, 1.599999999999998090, 3.363870538531282151 ) ) ;
#20836 = CARTESIAN_POINT ( 'NONE',  ( 47.49328262214483232, -3.991926107141724245, 1.294864543653815314 ) ) ;
#20837 = CARTESIAN_POINT ( 'NONE',  ( 15.97944027357901042, 2.710596767400014429, 4.680923748383045258 ) ) ;
#20838 = AXIS2_PLACEMENT_3D ( 'NONE', #25730, #5132, #22093 ) ;
#20839 = FACE_OUTER_BOUND ( 'NONE', #2764, .T. ) ;
#20840 = CARTESIAN_POINT ( 'NONE',  ( 57.00320971560400096, 0.7176258130632211518, -1.806074485252040285 ) ) ;
#20842 = CARTESIAN_POINT ( 'NONE',  ( 51.69999998375428163, -4.079529477378105007, 2.128865254696994391 ) ) ;
#20841 = DIRECTION ( 'NONE',  ( 0.000000000000000000, 0.000000000000000000, 1.000000000000000000 ) ) ;
#20843 = EDGE_CURVE ( 'NONE', #7637, #13776, #16283, .T. ) ;
#20844 = AXIS2_PLACEMENT_3D ( 'NONE', #18529, #16632, #15974 ) ;
#20845 = DIRECTION ( 'NONE',  ( 3.489354422748178582E-15, -1.218509414717996338E-16, 1.000000000000000000 ) ) ;
#20846 = CARTESIAN_POINT ( 'NONE',  ( 58.66133336607601478, 1.348863877412731505, 1.302803168108652931 ) ) ;
#20847 = CARTESIAN_POINT ( 'NONE',  ( 51.25000000000002842, -0.9938153758920951208, 1.589954715908409977 ) ) ;
#20848 = ORIENTED_EDGE ( 'NONE', *, *, #16340, .F. ) ;
#20849 = CARTESIAN_POINT ( 'NONE',  ( 51.25000000000001421, 5.368159983410797313E-13, 3.111507638930570854E-58 ) ) ;
#20850 = ORIENTED_EDGE ( 'NONE', *, *, #3019, .T. ) ;
#20851 = EDGE_LOOP ( 'NONE', ( #24964, #27281, #5856, #28042, #28773, #2483 ) ) ;
#20852 = EDGE_CURVE ( 'NONE', #27277, #9570, #30690, .T. ) ;
#20853 = CARTESIAN_POINT ( 'NONE',  ( 50.91843332348674522, -3.908336253171006636, 1.238913932502388571 ) ) ;
#20854 = EDGE_LOOP ( 'NONE', ( #27357, #24256, #1068, #960 ) ) ;
#20855 = EDGE_CURVE ( 'NONE', #8913, #3555, #4239, .T. ) ;
#20856 = CARTESIAN_POINT ( 'NONE',  ( 53.66601923242430416, 4.681126589747570677, 2.049999999999812861 ) ) ;
#20857 = CARTESIAN_POINT ( 'NONE',  ( -57.65835481156723574, -0.8699069336946629871, 4.241846523238430144 ) ) ;
#20859 = CARTESIAN_POINT ( 'NONE',  ( 51.03845481666589734, -3.901365292554824560, -1.261477279112157568 ) ) ;
#20858 = DIRECTION ( 'NONE',  ( 3.489354422748178582E-15, -1.218509414717996338E-16, 1.000000000000000000 ) ) ;
#20860 = ADVANCED_FACE ( 'NONE', ( #25316 ), #15670, .F. ) ;
#20861 = ORIENTED_EDGE ( 'NONE', *, *, #14651, .F. ) ;
#20862 = ORIENTED_EDGE ( 'NONE', *, *, #23526, .F. ) ;
#20863 = DIRECTION ( 'NONE',  ( 1.000000000000000000, 3.054025858079668409E-16, -2.042474015755241579E-16 ) ) ;
#20864 = CARTESIAN_POINT ( 'NONE',  ( 67.99999999999998579, 4.867971026610729436E-16, -3.950000000000712497 ) ) ;
#20865 = ORIENTED_EDGE ( 'NONE', *, *, #30363, .F. ) ;
#20867 = CYLINDRICAL_SURFACE ( 'NONE', #25642, 1.000000000000000000 ) ;
#20866 = CARTESIAN_POINT ( 'NONE',  ( 34.50000000000001421, 0.000000000000000000, 0.000000000000000000 ) ) ;
#20868 = CARTESIAN_POINT ( 'NONE',  ( 48.00000000000001421, -3.657334280697314810, -2.105684202162501073 ) ) ;
#20869 = VERTEX_POINT ( 'NONE', #22947 ) ;
#20870 = CARTESIAN_POINT ( 'NONE',  ( -36.92362342067168868, 5.092377074781550661, -1.825725187625013346 ) ) ;
#20871 = CARTESIAN_POINT ( 'NONE',  ( 58.72419296898058860, 1.822284191843672074, -0.4419487341008165315 ) ) ;
#20872 =( NAMED_UNIT ( * ) PLANE_ANGLE_UNIT ( ) SI_UNIT ( $, .RADIAN. ) );
#20873 = CARTESIAN_POINT ( 'NONE',  ( 56.95000000000001705, 0.6820512820512817376, 1.773360101234997988 ) ) ;
#20874 = CARTESIAN_POINT ( 'NONE',  ( -56.69702994616203284, -2.078460969082631227, -3.600000000000207923 ) ) ;
#20875 = CARTESIAN_POINT ( 'NONE',  ( 60.94140446606686368, -0.5380862305903196807, -1.858165151418244010 ) ) ;
#20876 =( BOUNDED_CURVE ( )  B_SPLINE_CURVE ( 2, ( #8277, #17945, #28379, #9380, #14280, #20947, #19050, #23945, #21284 ),
 .UNSPECIFIED., .F., .T. ) 
 B_SPLINE_CURVE_WITH_KNOTS ( ( 3, 2, 2, 2, 3 ),
 ( 0.4166666666666666852, 0.4259259259259259300, 0.4444444444444444198, 0.4629629629629629650, 0.4722222222222222654 ),
 .UNSPECIFIED. ) 
 CURVE ( )  GEOMETRIC_REPRESENTATION_ITEM ( )  RATIONAL_B_SPLINE_CURVE ( ( 0.9330127018922194093, 0.9330127018922195203, 1.000000000000000000, 0.8660254037844387076, 1.000000000000000000, 0.8660254037844387076, 1.000000000000000000, 0.9330127018922189652, 0.9330127018922194093 ) ) 
 REPRESENTATION_ITEM ( '' )  );
#20877 = CIRCLE ( 'NONE', #1194, 2.700000000000000178 ) ;
#20878 = ADVANCED_FACE ( 'NONE', ( #1236 ), #10897, .F. ) ;
#20879 = CARTESIAN_POINT ( 'NONE',  ( -58.42292740578360366, -3.330682475591780101, -0.6830477631804265926 ) ) ;
#20881 = ADVANCED_FACE ( 'NONE', ( #11062 ), #20742, .F. ) ;
#20880 = CARTESIAN_POINT ( 'NONE',  ( 51.70000000000002416, 6.982261990806648555E-14, -1.793082891011605378E-13 ) ) ;
#20882 = LINE ( 'NONE', #30511, #16400 ) ;
#20883 = CARTESIAN_POINT ( 'NONE',  ( 52.27846493713558829, 4.392730452021146981, 1.555162895512434806 ) ) ;
#20884 = CARTESIAN_POINT ( 'NONE',  ( 48.37893541770432648, 0.9199776782966302413, -3.998258245321878235 ) ) ;
#20885 = ORIENTED_EDGE ( 'NONE', *, *, #28637, .F. ) ;
#20886 = CARTESIAN_POINT ( 'NONE',  ( 58.75000018595668649, 1.701752411747378568, 0.9248597378506533406 ) ) ;
#20887 = ORIENTED_EDGE ( 'NONE', *, *, #15693, .F. ) ;
#20888 = DIRECTION ( 'NONE',  ( 1.000000000000000000, 3.054025858079668409E-16, -2.042474015755241579E-16 ) ) ;
#20890 = CARTESIAN_POINT ( 'NONE',  ( 58.65000045311413857, -1.383426348886330537, 1.265716300432485841 ) ) ;
#20889 = CARTESIAN_POINT ( 'NONE',  ( 48.38950019258942348, 0.7811435014053292880, 4.027217152859519089 ) ) ;
#20891 = EDGE_LOOP ( 'NONE', ( #5286, #22202, #138, #29816 ) ) ;
#20892 = ORIENTED_EDGE ( 'NONE', *, *, #13911, .F. ) ;
#20893 = CARTESIAN_POINT ( 'NONE',  ( 50.25000000000002842, -0.5380862305904318132, -2.008165151418244143 ) ) ;
#20894 = CARTESIAN_POINT ( 'NONE',  ( -59.69999999999996021, 1.397030005794335672, -3.099726949734703751 ) ) ;
#20896 = DIRECTION ( 'NONE',  ( 0.000000000000000000, 0.9996898646859343485, 0.02490330187381124133 ) ) ;
#20895 = CARTESIAN_POINT ( 'NONE',  ( -60.94702994616203995, 4.156921938165313080, -2.011299877933566609E-13 ) ) ;
#20897 = ORIENTED_EDGE ( 'NONE', *, *, #20843, .F. ) ;
#20898 = CARTESIAN_POINT ( 'NONE',  ( -59.04792740578360366, -1.073804522883517132, -3.225979517392335350 ) ) ;
#20899 = AXIS2_PLACEMENT_3D ( 'NONE', #917, #10570, #24659 ) ;
#20900 = DIRECTION ( 'NONE',  ( 1.000000000000000000, 0.000000000000000000, 0.000000000000000000 ) ) ;
#20901 = SHAPE_DEFINITION_REPRESENTATION ( #37, #25673 ) ;
#20902 = CARTESIAN_POINT ( 'NONE',  ( 53.26700867189011745, 4.937278075622002937, -1.609149601427315890 ) ) ;
#20903 = CARTESIAN_POINT ( 'NONE',  ( 52.06628335902944826, 0.5434431642986583544, -1.718465885608440269 ) ) ;
#20904 = CARTESIAN_POINT ( 'NONE',  ( 64.25000000000001421, 1.163569835200988601E-28, -2.243276760206714411E-13 ) ) ;
#20905 = VERTEX_POINT ( 'NONE', #15957 ) ;
#20906 = DIRECTION ( 'NONE',  ( -1.000000000000000000, -3.054025858079668409E-16, 2.042474015755241579E-16 ) ) ;
#20907 =( BOUNDED_CURVE ( )  B_SPLINE_CURVE ( 3, ( #7324, #26799, #16995, #10162 ),
 .UNSPECIFIED., .F., .T. ) 
 B_SPLINE_CURVE_WITH_KNOTS ( ( 4, 4 ),
 ( 5.439460278842601859, 5.455963239578337287 ),
 .UNSPECIFIED. ) 
 CURVE ( )  GEOMETRIC_REPRESENTATION_ITEM ( )  RATIONAL_B_SPLINE_CURVE ( ( 1.000000000000000000, 0.9999773044860189586, 0.9999773044860189586, 1.000000000000000000 ) ) 
 REPRESENTATION_ITEM ( '' )  );
#20908 = CARTESIAN_POINT ( 'NONE',  ( -36.77443515226919857, 3.646557212684436777, -3.995389720703250713 ) ) ;
#20909 = CARTESIAN_POINT ( 'NONE',  ( 51.25000000000001421, 0.9938153758931693726, 1.589954715908409755 ) ) ;
#20910 = DIRECTION ( 'NONE',  ( 1.000000000000000000, 1.047444401652940007E-14, -0.000000000000000000 ) ) ;
#20911 = EDGE_CURVE ( 'NONE', #23157, #1451, #25620, .T. ) ;
#20912 = ADVANCED_FACE ( 'NONE', ( #31158 ), #2345, .T. ) ;
#20913 = CARTESIAN_POINT ( 'NONE',  ( 57.01549179440438309, -0.7366256376427431363, -2.429951667075468613 ) ) ;
#20916 = EDGE_CURVE ( 'NONE', #10216, #13616, #11202, .T. ) ;
#20915 = CARTESIAN_POINT ( 'NONE',  ( 58.65266784251149801, -1.792820108339197027, -0.5492726012740126729 ) ) ;
#20914 = CARTESIAN_POINT ( 'NONE',  ( 17.21035195517769267, -2.471857751707523654E-15, 0.000000000000000000 ) ) ;
#20917 = TOROIDAL_SURFACE ( 'NONE', #5717, 3.299999999999999822, 0.1000000000000000056 ) ;
#20918 = AXIS2_PLACEMENT_3D ( 'NONE', #16844, #28871, #13798 ) ;
#20919 = CARTESIAN_POINT ( 'NONE',  ( 47.00000000000000711, -3.933368109459638884, -2.186004417993338667 ) ) ;
#20921 = CARTESIAN_POINT ( 'NONE',  ( 60.87997700083089114, -0.6727827007652724678, 1.479885446458161669 ) ) ;
#20920 = CARTESIAN_POINT ( 'NONE',  ( -44.59999999999996589, -1.599999999999981215, -3.363870538531657850 ) ) ;
#20922 = ORIENTED_EDGE ( 'NONE', *, *, #5161, .T. ) ;
#20923 = CARTESIAN_POINT ( 'NONE',  ( 51.25000000000001421, 5.368152558471320595E-13, 1.875000000000001776 ) ) ;
#20924 = CARTESIAN_POINT ( 'NONE',  ( 58.75000000000002842, -1.039502773796089796, -1.650471618824325359 ) ) ;
#20926 = CARTESIAN_POINT ( 'NONE',  ( 47.86726225955752767, -4.031600731908414836, -1.173113608511841655 ) ) ;
#20925 = CARTESIAN_POINT ( 'NONE',  ( -59.19999999999996732, 2.580747833305914618, -0.9498634748674507078 ) ) ;
#20927 = CARTESIAN_POINT ( 'NONE',  ( 15.45522337368515409, -5.005099703116265175, 1.423440526321969157 ) ) ;
#20928 = VERTEX_POINT ( 'NONE', #14687 ) ;
#20929 = CARTESIAN_POINT ( 'NONE',  ( 53.05367528747408556, 8.375580747031632356, 2.049999999999815081 ) ) ;
#20930 = DIRECTION ( 'NONE',  ( 0.000000000000000000, -0.2008964009354147484, 0.9796124928211139560 ) ) ;
#20931 = EDGE_CURVE ( 'NONE', #13697, #7185, #18793, .T. ) ;
#20932 = ORIENTED_EDGE ( 'NONE', *, *, #9667, .T. ) ;
#20933 =( REPRESENTATION_RELATIONSHIP ('NONE','NONE', #7047, #18201 ) REPRESENTATION_RELATIONSHIP_WITH_TRANSFORMATION ( #149 )SHAPE_REPRESENTATION_RELATIONSHIP( ) );
#20934 = CARTESIAN_POINT ( 'NONE',  ( 58.75000000000000000, 2.079005547593415937, 1.004182178118534636E-12 ) ) ;
#20935 = VERTEX_POINT ( 'NONE', #16915 ) ;
#20936 = CARTESIAN_POINT ( 'NONE',  ( -59.69999999999995310, -2.472655081704904223, -2.581384084800625978 ) ) ;
#20937 = ORIENTED_EDGE ( 'NONE', *, *, #24517, .T. ) ;
#20938 = FILL_AREA_STYLE ('',( #13470 ) ) ;
#20939 = CARTESIAN_POINT ( 'NONE',  ( -54.69702994616206837, -2.078460969082657872, 3.599999999999797584 ) ) ;
#20940 = CARTESIAN_POINT ( 'NONE',  ( -55.70655989232410832, 1.962990915244748891, -3.400000000000189093 ) ) ;
#20941 = ORIENTED_EDGE ( 'NONE', *, *, #20270, .F. ) ;
#20942 = SURFACE_STYLE_FILL_AREA ( #21584 ) ;
#20943 = VERTEX_POINT ( 'NONE', #26558 ) ;
#20944 = VECTOR ( 'NONE', #18561, 1000.000000000000000 ) ;
#20945 = EDGE_LOOP ( 'NONE', ( #8846, #13057, #25933, #16192 ) ) ;
#20946 = CARTESIAN_POINT ( 'NONE',  ( -58.18749999999995737, 1.962990915244749557, -3.400000000000197531 ) ) ;
#20947 = CARTESIAN_POINT ( 'NONE',  ( -57.56249999999997158, 4.108500314926514463, -1.367561758111401238 ) ) ;
#20948 = CARTESIAN_POINT ( 'NONE',  ( 51.80000000000002558, 4.286401202180091907, 1.833837317107078313 ) ) ;
#20949 = CARTESIAN_POINT ( 'NONE',  ( 51.90000000000001279, 1.734723475976807094E-15, -4.275000000000000355 ) ) ;
#20950 = AXIS2_PLACEMENT_3D ( 'NONE', #12449, #17224, #28629 ) ;
#20951 = LINE ( 'NONE', #29971, #13987 ) ;
#20952 = EDGE_CURVE ( 'NONE', #24423, #4345, #16877, .T. ) ;
#20953 = DIRECTION ( 'NONE',  ( 0.000000000000000000, 0.000000000000000000, 1.000000000000000000 ) ) ;
#20955 = AXIS2_PLACEMENT_3D ( 'NONE', #28812, #16782, #4723 ) ;
#20954 = DIRECTION ( 'NONE',  ( 1.000000000000000000, -0.000000000000000000, -1.047444401652940007E-14 ) ) ;
#20956 = CARTESIAN_POINT ( 'NONE',  ( -59.68687113065863059, 2.402179451507872709, -1.230958653213889198 ) ) ;
#20957 = CARTESIAN_POINT ( 'NONE',  ( 15.41080140630216810, 5.326563020867391529, -0.9981196555231990342 ) ) ;
#20958 = CARTESIAN_POINT ( 'NONE',  ( -59.65432904196666186, -2.186231771939587620, 1.524642732528142197 ) ) ;
#20959 = CARTESIAN_POINT ( 'NONE',  ( 50.40000000000001990, 2.428612866367529932E-14, 0.000000000000000000 ) ) ;
#20960 = TOROIDAL_SURFACE ( 'NONE', #6779, 2.729289321881338548, 0.05000000000000000278 ) ;
#20961 = CARTESIAN_POINT ( 'NONE',  ( 50.38699024846547303, 1.088846059295805135, -3.899771020632008423 ) ) ;
#20962 = VERTEX_POINT ( 'NONE', #6776 ) ;
#20963 = CARTESIAN_POINT ( 'NONE',  ( 61.25000000000002132, 6.415596960124259844E-13, 3.111507638930570854E-58 ) ) ;
#20964 = CARTESIAN_POINT ( 'NONE',  ( -36.14504829323105639, -1.093755498983980612, -5.295967089285813501 ) ) ;
#20965 = EDGE_CURVE ( 'NONE', #8534, #7227, #12298, .T. ) ;
#20966 = ORIENTED_EDGE ( 'NONE', *, *, #3445, .T. ) ;
#20967 = CARTESIAN_POINT ( 'NONE',  ( 51.29331479884403677, 1.002608958138274442, 1.584424273060084376 ) ) ;
#20968 = CIRCLE ( 'NONE', #18438, 0.1000000000000000333 ) ;
#20969 = FACE_BOUND ( 'NONE', #21281, .T. ) ;
#20970 = CARTESIAN_POINT ( 'NONE',  ( -60.93749999999997868, 1.962990915244722689, 3.399999999999791633 ) ) ;
#20971 = VERTEX_POINT ( 'NONE', #11844 ) ;
#20972 = ORIENTED_EDGE ( 'NONE', *, *, #24547, .F. ) ;
#20973 = DIRECTION ( 'NONE',  ( 1.000000000000000000, 3.054025858079668409E-16, -2.042474015755241579E-16 ) ) ;
#20974 = ORIENTED_EDGE ( 'NONE', *, *, #18853, .T. ) ;
#20975 = CARTESIAN_POINT ( 'NONE',  ( 51.11922224408084503, 0.9310536428531384079, -1.338077479438677830 ) ) ;
#20976 = DIRECTION ( 'NONE',  ( -1.000000000000000000, -3.054025858079668409E-16, 2.042474015755241579E-16 ) ) ;
#20977 = ORIENTED_EDGE ( 'NONE', *, *, #10257, .F. ) ;
#20978 = CARTESIAN_POINT ( 'NONE',  ( 23.93127868632186050, 5.811091648296249801, -2.050000000000082867 ) ) ;
#20979 = DIRECTION ( 'NONE',  ( -1.404304041445553711E-15, 0.9030524935654929974, 0.4295302013422866994 ) ) ;
#20980 = AXIS2_PLACEMENT_3D ( 'NONE', #6094, #15744, #25394 ) ;
#20982 = EDGE_CURVE ( 'NONE', #22436, #24250, #1172, .T. ) ;
#20981 = CIRCLE ( 'NONE', #23502, 2.874999999999999112 ) ;
#20983 = CARTESIAN_POINT ( 'NONE',  ( 58.45000000000001705, -0.8000000000000001554, 1.778341924377873973 ) ) ;
#20984 = ORIENTED_EDGE ( 'NONE', *, *, #23356, .F. ) ;
#20985 = VERTEX_POINT ( 'NONE', #274 ) ;
#20986 = DIRECTION ( 'NONE',  ( -1.000000000000000000, -3.053848253006669023E-16, 2.042510438544995415E-16 ) ) ;
#20987 = CARTESIAN_POINT ( 'NONE',  ( -55.74999999999997868, 2.944486372867090473, 1.699999999999816547 ) ) ;
#20989 = CARTESIAN_POINT ( 'NONE',  ( 57.00057550097274373, -0.8023623105721646720, -2.473098203180232879 ) ) ;
#20988 = AXIS2_PLACEMENT_3D ( 'NONE', #28291, #23538, #21191 ) ;
#20990 = CARTESIAN_POINT ( 'NONE',  ( 51.25000000000001421, 1.100000000000537215, -1.996089927833914146 ) ) ;
#20991 = CARTESIAN_POINT ( 'NONE',  ( 58.74160516400055343, 1.390091577294495062, 1.258299259018362815 ) ) ;
#20992 = EDGE_CURVE ( 'NONE', #10297, #12844, #21833, .T. ) ;
#20993 = DIRECTION ( 'NONE',  ( -1.000000000000000000, 1.219044193948983948E-29, -3.491481338843133355E-15 ) ) ;
#20994 = AXIS2_PLACEMENT_3D ( 'NONE', #24427, #19701, #17164 ) ;
#20995 = CARTESIAN_POINT ( 'NONE',  ( -59.23418654921033522, -3.153953023162030078, 1.269874138521803975 ) ) ;
#20996 = SURFACE_SIDE_STYLE ('',( #18629 ) ) ;
#20997 = EDGE_CURVE ( 'NONE', #8754, #5843, #29986, .T. ) ;
#20998 = PRODUCT_DEFINITION_SHAPE ( 'NONE', 'NONE',  #31327 ) ;
#20999 = DIRECTION ( 'NONE',  ( 0.000000000000000000, 0.000000000000000000, -1.000000000000000000 ) ) ;
#21000 = DIRECTION ( 'NONE',  ( 0.000000000000000000, 0.000000000000000000, 1.000000000000000000 ) ) ;
#21001 = DIRECTION ( 'NONE',  ( -1.000000000000000000, -0.000000000000000000, -0.000000000000000000 ) ) ;
#21002 = ORIENTED_EDGE ( 'NONE', *, *, #18313, .T. ) ;
#21003 = CIRCLE ( 'NONE', #12412, 1.000000000000000000 ) ;
#21004 = ORIENTED_EDGE ( 'NONE', *, *, #5279, .T. ) ;
#21005 = ORIENTED_EDGE ( 'NONE', *, *, #2248, .F. ) ;
#21006 = EDGE_CURVE ( 'NONE', #11687, #19238, #22933, .T. ) ;
#21007 = CARTESIAN_POINT ( 'NONE',  ( 51.30663577364959593, -3.991980709735059918, 1.294710393269015603 ) ) ;
#21008 = EDGE_LOOP ( 'NONE', ( #7785, #30276, #22440, #15437, #24139, #25 ) ) ;
#21009 = CARTESIAN_POINT ( 'NONE',  ( 53.87894805006524734, 4.971284855691957993, 2.049999999999811973 ) ) ;
#21010 = AXIS2_PLACEMENT_3D ( 'NONE', #10178, #5593, #12547 ) ;
#21011 = CARTESIAN_POINT ( 'NONE',  ( -57.09585481156723574, 3.673546848079182414, 0.7533615035078063960 ) ) ;
#21013 = CARTESIAN_POINT ( 'NONE',  ( -36.48821680285229263, 2.849134329833883594, 4.601168830303214108 ) ) ;
#21012 = DIRECTION ( 'NONE',  ( 0.000000000000000000, -1.000000000000000000, -3.491481338843137694E-15 ) ) ;
#21014 = VERTEX_POINT ( 'NONE', #20240 ) ;
#21015 = ORIENTED_EDGE ( 'NONE', *, *, #14820, .T. ) ;
#21016 = CARTESIAN_POINT ( 'NONE',  ( -54.49999999999997868, 2.270506450603774156E-15, 4.375000000000000000 ) ) ;
#21017 = ORIENTED_EDGE ( 'NONE', *, *, #24226, .T. ) ;
#21018 = DIRECTION ( 'NONE',  ( 3.002035892788117459E-16, -0.9996898646859343485, -0.02490330187381123786 ) ) ;
#21019 = EDGE_LOOP ( 'NONE', ( #22235, #9716, #12072, #25826 ) ) ;
#21021 = DIRECTION ( 'NONE',  ( 1.000000000000000000, 0.000000000000000000, 0.000000000000000000 ) ) ;
#21020 = FACE_OUTER_BOUND ( 'NONE', #10543, .T. ) ;
#21022 = AXIS2_PLACEMENT_3D ( 'NONE', #29596, #19500, #24395 ) ;
#21023 = DIRECTION ( 'NONE',  ( 0.000000000000000000, 0.000000000000000000, -1.000000000000000000 ) ) ;
#21024 = VERTEX_POINT ( 'NONE', #435 ) ;
#21025 = FACE_OUTER_BOUND ( 'NONE', #13353, .T. ) ;
#21026 = EDGE_CURVE ( 'NONE', #3612, #950, #9282, .T. ) ;
#21027 = FACE_BOUND ( 'NONE', #12292, .T. ) ;
#21028 = CARTESIAN_POINT ( 'NONE',  ( -54.49998431799114940, -1.548747819918198987, -3.331336553795240185 ) ) ;
#21029 = CARTESIAN_POINT ( 'NONE',  ( 58.45000000000001705, 0.8000000000000000444, 2.471260002560650371 ) ) ;
#21030 = CARTESIAN_POINT ( 'NONE',  ( -57.44702994616203284, -2.078460969082631227, -3.600000000000210587 ) ) ;
#21031 = AXIS2_PLACEMENT_3D ( 'NONE', #15167, #3134, #27500 ) ;
#21032 = CARTESIAN_POINT ( 'NONE',  ( 51.83867713794252552, 0.3186276668619861807, 4.343079704710790523 ) ) ;
#21033 = AXIS2_PLACEMENT_3D ( 'NONE', #3149, #12790, #10432 ) ;
#21034 = AXIS2_PLACEMENT_3D ( 'NONE', #9394, #16208, #6854 ) ;
#21035 = ADVANCED_FACE ( 'NONE', ( #3118 ), #31011, .T. ) ;
#21036 = DIRECTION ( 'NONE',  ( 1.000000000000000000, -0.000000000000000000, -0.000000000000000000 ) ) ;
#21037 = EDGE_CURVE ( 'NONE', #31243, #15189, #18890, .T. ) ;
#21038 = CARTESIAN_POINT ( 'NONE',  ( 50.50000002742975624, 0.7904052113207085117, -4.025738854575411807 ) ) ;
#21039 = EDGE_CURVE ( 'NONE', #20519, #16970, #5950, .T. ) ;
#21040 = CIRCLE ( 'NONE', #11411, 4.199999999999954881 ) ;
#21041 = AXIS2_PLACEMENT_3D ( 'NONE', #17837, #27471, #25097 ) ;
#21042 = CARTESIAN_POINT ( 'NONE',  ( -56.73542740578360366, 0.7887156198831762888, -3.845940847736172064 ) ) ;
#21043 =( GEOMETRIC_REPRESENTATION_CONTEXT ( 3 ) GLOBAL_UNCERTAINTY_ASSIGNED_CONTEXT ( ( #12647 ) ) GLOBAL_UNIT_ASSIGNED_CONTEXT ( ( #8744, #3857, #1623 ) ) REPRESENTATION_CONTEXT ( 'NONE', 'WORKASPACE' ) );
#21044 = DIRECTION ( 'NONE',  ( -1.000000000000000000, 0.000000000000000000, 1.047444401652940007E-14 ) ) ;
#21045 = ORIENTED_EDGE ( 'NONE', *, *, #5760, .F. ) ;
#21046 = CARTESIAN_POINT ( 'NONE',  ( 51.80000000000001847, 2.428612866367529932E-14, -1.808587333520743709E-13 ) ) ;
#21047 = CARTESIAN_POINT ( 'NONE',  ( -36.48821680285185920, -0.3995010896672921419, 5.397102918580241493 ) ) ;
#21048 = CARTESIAN_POINT ( 'NONE',  ( 59.00000000000005684, 1.401298464324817071E-42, 2.999999999999382272 ) ) ;
#21049 = VERTEX_POINT ( 'NONE', #27188 ) ;
#21050 = ADVANCED_FACE ( 'NONE', ( #15306 ), #24807, .F. ) ;
#21051 = CARTESIAN_POINT ( 'NONE',  ( 58.65263613458531466, 1.656197658589030342, 0.8791532451981106666 ) ) ;
#21052 = ORIENTED_EDGE ( 'NONE', *, *, #8987, .T. ) ;
#21053 = DIRECTION ( 'NONE',  ( 1.000000000000000000, 0.000000000000000000, 4.738179285253040686E-16 ) ) ;
#21054 = CARTESIAN_POINT ( 'NONE',  ( 58.66118217212467556, -1.313877211063203987, 1.337770226785896854 ) ) ;
#21055 = EDGE_LOOP ( 'NONE', ( #3309, #20887, #29841, #63 ) ) ;
#21056 = TOROIDAL_SURFACE ( 'NONE', #11428, 1.524417381223824197, 0.05000000000000000278 ) ;
#21057 = ORIENTED_EDGE ( 'NONE', *, *, #30622, .T. ) ;
#21058 = DIRECTION ( 'NONE',  ( 0.000000000000000000, -0.2008964009354147484, 0.9796124928211139560 ) ) ;
#21059 = DIRECTION ( 'NONE',  ( 0.000000000000000000, 0.000000000000000000, -1.000000000000000000 ) ) ;
#21060 = AXIS2_PLACEMENT_3D ( 'NONE', #13043, #20500, #27916 ) ;
#21061 = CARTESIAN_POINT ( 'NONE',  ( -44.59999999999997300, -6.102218906431391608E-14, -1.870876429524648473E-13 ) ) ;
#21062 = ORIENTED_EDGE ( 'NONE', *, *, #3470, .T. ) ;
#21063 = CARTESIAN_POINT ( 'NONE',  ( -54.99999999999997868, -2.489203624310585283, 2.804704140674916690 ) ) ;
#21065 = ADVANCED_FACE ( 'NONE', ( #5808 ), #26870, .F. ) ;
#21064 = COLOUR_RGB ( '', 0.09019608, 0.27058824, 0.51372549) ;
#21066 = CARTESIAN_POINT ( 'NONE',  ( -36.81959771849334828, 2.696520634775258607, 4.691964194339944605 ) ) ;
#21067 = APPLICATION_PROTOCOL_DEFINITION ( 'draft international standard', 'automotive_design', 1998, #5898 ) ;
#21068 = AXIS2_PLACEMENT_3D ( 'NONE', #27592, #3388, #22718 ) ;
#21069 = CARTESIAN_POINT ( 'NONE',  ( 53.38896854193014008, 5.061769990941914266, -1.621051239797380195 ) ) ;
#21070 = CARTESIAN_POINT ( 'NONE',  ( -61.34999999999997300, -2.565134197206211386, 0.6652717868084008224 ) ) ;
#21071 = CIRCLE ( 'NONE', #1832, 1.000000000000000000 ) ;
#21072 = ADVANCED_FACE ( 'NONE', ( #24489 ), #17228, .F. ) ;
#21073 = CARTESIAN_POINT ( 'NONE',  ( 50.30000000000001847, -1.391941090707485396, -3.850000000000022737 ) ) ;
#21074 = VERTEX_POINT ( 'NONE', #10397 ) ;
#21075 = CARTESIAN_POINT ( 'NONE',  ( -35.85663232820583346, -4.683225679163351529, -2.703237727951242952 ) ) ;
#21076 = CIRCLE ( 'NONE', #14043, 0.5000000000000013323 ) ;
#21077 = CARTESIAN_POINT ( 'NONE',  ( -35.85663232820601820, 4.018128179617554530, -3.618665901676620500 ) ) ;
#21078 = ADVANCED_FACE ( 'NONE', ( #1061 ), #22441, .F. ) ;
#21079 = CARTESIAN_POINT ( 'NONE',  ( -59.37241364122699849, 3.319464018575120967, 1.250136525132569787 ) ) ;
#21080 = DIRECTION ( 'NONE',  ( 3.352440544655105674E-15, 0.2793919678926571892, 0.9601771338024399638 ) ) ;
#21081 = ADVANCED_FACE ( 'NONE', ( #29543 ), #16367, .T. ) ;
#21082 = AXIS2_PLACEMENT_3D ( 'NONE', #6935, #7092, #19291 ) ;
#21083 = AXIS2_PLACEMENT_3D ( 'NONE', #28722, #2589, #16845 ) ;
#21084 = CARTESIAN_POINT ( 'NONE',  ( 15.71019289815287223, 0.8926979523208264933, -5.334280177567949366 ) ) ;
#21085 = AXIS2_PLACEMENT_3D ( 'NONE', #7283, #14400, #24380 ) ;
#21087 = CARTESIAN_POINT ( 'NONE',  ( 58.75000000000004263, -1.782657835994226003, -0.5811678240974800236 ) ) ;
#21086 = DIRECTION ( 'NONE',  ( 0.000000000000000000, 0.000000000000000000, 1.000000000000000000 ) ) ;
#21088 = AXIS2_PLACEMENT_3D ( 'NONE', #1869, #11539, #30845 ) ;
#21089 = CARTESIAN_POINT ( 'NONE',  ( 47.49107765765781153, -4.380148595134368605, -1.408962902656728744 ) ) ;
#21090 = CIRCLE ( 'NONE', #9444, 3.625000000000028866 ) ;
#21092 = CARTESIAN_POINT ( 'NONE',  ( 17.21035195517769267, -5.407411300779135566, 6.622168941172392137E-16 ) ) ;
#21091 = CARTESIAN_POINT ( 'NONE',  ( 49.00000000000004974, 3.520859547548639454E-16, 2.874999999999486189 ) ) ;
#21093 = ORIENTED_EDGE ( 'NONE', *, *, #14805, .F. ) ;
#21094 = CARTESIAN_POINT ( 'NONE',  ( 60.88446240048057945, -0.4999999999993621769, -1.718465885608439603 ) ) ;
#21095 = AXIS2_PLACEMENT_3D ( 'NONE', #1767, #19828, #12362 ) ;
#21096 = AXIS2_PLACEMENT_3D ( 'NONE', #8133, #17805, #537 ) ;
#21097 = CARTESIAN_POINT ( 'NONE',  ( 65.00000000000005684, -1.025519176787267142E-28, 4.049999999999319478 ) ) ;
#21099 = CARTESIAN_POINT ( 'NONE',  ( -36.26369610968610857, 4.878538113278829691, 1.812957040858136804 ) ) ;
#21098 = DIRECTION ( 'NONE',  ( 1.000000000000000000, 0.000000000000000000, 0.000000000000000000 ) ) ;
#21100 = DIRECTION ( 'NONE',  ( -1.047444401652940007E-14, 0.000000000000000000, -1.000000000000000000 ) ) ;
#21101 = ORIENTED_EDGE ( 'NONE', *, *, #2688, .T. ) ;
#21102 = ORIENTED_EDGE ( 'NONE', *, *, #12567, .F. ) ;
#21103 = CARTESIAN_POINT ( 'NONE',  ( -36.48174642952978530, -5.008501212420972237, 2.048848402342071218 ) ) ;
#21104 = DIRECTION ( 'NONE',  ( 0.03489949670250203084, 0.9993908270190957621, -3.673133589935336920E-30 ) ) ;
#21105 = EDGE_LOOP ( 'NONE', ( #20932, #201, #3693 ) ) ;
#21106 = DIRECTION ( 'NONE',  ( 0.000000000000000000, 0.000000000000000000, 1.000000000000000000 ) ) ;
#21107 = AXIS2_PLACEMENT_3D ( 'NONE', #23125, #30526, #25793 ) ;
#21108 = EDGE_LOOP ( 'NONE', ( #8041, #8519, #12253, #27618, #26737, #12012, #18765 ) ) ;
#21109 = EDGE_CURVE ( 'NONE', #4801, #14417, #7766, .T. ) ;
#21110 = CARTESIAN_POINT ( 'NONE',  ( 58.64999999999999147, 1.872332544501833507, -0.09997921184724641031 ) ) ;
#21111 = EDGE_LOOP ( 'NONE', ( #18328, #798, #698, #5767, #28509, #16221 ) ) ;
#21112 = EDGE_CURVE ( 'NONE', #13515, #25588, #24966, .T. ) ;
#21113 = CARTESIAN_POINT ( 'NONE',  ( -55.63452994616205416, 3.117691453623977704, 1.799999999999817524 ) ) ;
#21114 = CARTESIAN_POINT ( 'NONE',  ( -57.26905989232410832, 2.023778652682507790E-14, -3.400000000000203304 ) ) ;
#21115 = ORIENTED_EDGE ( 'NONE', *, *, #331, .T. ) ;
#21116 = CIRCLE ( 'NONE', #3912, 2.000000000000000000 ) ;
#21117 = EDGE_CURVE ( 'NONE', #25822, #4862, #17270, .T. ) ;
#21118 = ORIENTED_EDGE ( 'NONE', *, *, #859, .T. ) ;
#21119 = ORIENTED_EDGE ( 'NONE', *, *, #3069, .T. ) ;
#21120 = AXIS2_PLACEMENT_3D ( 'NONE', #927, #22311, #29887 ) ;
#21121 = CIRCLE ( 'NONE', #9981, 4.199999999999993072 ) ;
#21122 = CARTESIAN_POINT ( 'NONE',  ( -59.81249999999995026, -1.962990915244707368, -3.400000000000219291 ) ) ;
#21123 = VECTOR ( 'NONE', #21250, 999.9999999999998863 ) ;
#21124 = AXIS2_PLACEMENT_3D ( 'NONE', #22630, #21998, #930 ) ;
#21125 = DIRECTION ( 'NONE',  ( 0.000000000000000000, 1.000000000000000000, 3.491481338843133355E-15 ) ) ;
#21126 = CARTESIAN_POINT ( 'NONE',  ( 22.25735896772342315, 7.137076052088946909, -1.425000000000077538 ) ) ;
#21127 = CARTESIAN_POINT ( 'NONE',  ( 51.59739104186229497, -1.010292945602101256, -1.272765950230260623 ) ) ;
#21129 = DIRECTION ( 'NONE',  ( -3.491481338843133355E-15, -3.491481338843133355E-15, 1.000000000000000000 ) ) ;
#21128 = DIRECTION ( 'NONE',  ( -1.000000000000000000, -3.054025858079668409E-16, 2.042474015755241579E-16 ) ) ;
#21130 = AXIS2_PLACEMENT_3D ( 'NONE', #21197, #21021, #4378 ) ;
#21131 = CIRCLE ( 'NONE', #7469, 0.09999999999999982514 ) ;
#21132 = DIRECTION ( 'NONE',  ( -0.9396926207859088720, -0.008517430876163569961, 0.3419140708011006446 ) ) ;
#21133 = DIRECTION ( 'NONE',  ( -1.000000000000000000, -0.000000000000000000, -0.000000000000000000 ) ) ;
#21134 = CARTESIAN_POINT ( 'NONE',  ( -36.81959771849334828, -2.696520634775307457, -4.691964194339934835 ) ) ;
#21135 = CARTESIAN_POINT ( 'NONE',  ( 57.04415282905778639, 0.8156862745098041323, 2.468735688885368873 ) ) ;
#21136 = CARTESIAN_POINT ( 'NONE',  ( 50.56948141424500420, -0.1019060742254479235, 1.190674082256532262 ) ) ;
#21137 = CARTESIAN_POINT ( 'NONE',  ( 60.99772080470438596, -0.5608984830164329694, 1.857935446186627093 ) ) ;
#21138 = VERTEX_POINT ( 'NONE', #2968 ) ;
#21140 = CARTESIAN_POINT ( 'NONE',  ( -54.49999999999997868, 0.9643027244899942119, -4.702139965541348055 ) ) ;
#21139 = CARTESIAN_POINT ( 'NONE',  ( 65.00000000000001421, -1.025519176787267142E-28, -6.808388610744108654E-13 ) ) ;
#21141 = CARTESIAN_POINT ( 'NONE',  ( 47.00000000000002132, 2.478823385132571406E-14, 4.100000000000022737 ) ) ;
#21142 = AXIS2_PLACEMENT_3D ( 'NONE', #4686, #21668, #9623 ) ;
#21143 = ORIENTED_EDGE ( 'NONE', *, *, #19790, .F. ) ;
#21144 = VECTOR ( 'NONE', #23997, 1000.000000000000000 ) ;
#21145 = CARTESIAN_POINT ( 'NONE',  ( 22.54717926605044198, 7.740376438784147162, -1.425000000000078204 ) ) ;
#21146 = CARTESIAN_POINT ( 'NONE',  ( -59.56249999999996447, 3.925981830489463142, -1.971446734091520023E-13 ) ) ;
#21147 = ORIENTED_EDGE ( 'NONE', *, *, #25539, .F. ) ;
#21148 = VERTEX_POINT ( 'NONE', #12612 ) ;
#21149 = CARTESIAN_POINT ( 'NONE',  ( 15.48609859788819598, 4.910307320510450602, 1.715181477143260969 ) ) ;
#21150 = ORIENTED_EDGE ( 'NONE', *, *, #23059, .T. ) ;
#21151 = EDGE_CURVE ( 'NONE', #23938, #4123, #12310, .T. ) ;
#21152 = CARTESIAN_POINT ( 'NONE',  ( 58.65000045311390409, -1.663878723406634785, 0.8645309767543464252 ) ) ;
#21153 = CARTESIAN_POINT ( 'NONE',  ( 51.25000000000002132, 1.836970198722195229E-16, 1.374999999999822586 ) ) ;
#21154 = ORIENTED_EDGE ( 'NONE', *, *, #25467, .T. ) ;
#21155 = DIRECTION ( 'NONE',  ( 0.000000000000000000, 0.000000000000000000, 1.000000000000000000 ) ) ;
#21156 = CARTESIAN_POINT ( 'NONE',  ( 52.20711756518983293, 0.5000000000005468959, 1.807104036850122109 ) ) ;
#21157 = CIRCLE ( 'NONE', #25176, 159.6997717543496833 ) ;
#21158 = DIRECTION ( 'NONE',  ( 0.000000000000000000, -0.2008964009354147762, 0.9796124928211140670 ) ) ;
#21159 = VERTEX_POINT ( 'NONE', #20394 ) ;
#21160 = ORIENTED_EDGE ( 'NONE', *, *, #18205, .F. ) ;
#21161 = AXIS2_PLACEMENT_3D ( 'NONE', #30657, #28297, #20404 ) ;
#21162 = CIRCLE ( 'NONE', #5455, 1.487500000000000933 ) ;
#21163 = DIRECTION ( 'NONE',  ( 1.000000000000000000, 3.053848253006669023E-16, -2.042510438544995415E-16 ) ) ;
#21164 = FACE_OUTER_BOUND ( 'NONE', #6129, .T. ) ;
#21165 = DIRECTION ( 'NONE',  ( 0.000000000000000000, 0.000000000000000000, -1.000000000000000000 ) ) ;
#21166 = ORIENTED_EDGE ( 'NONE', *, *, #26426, .F. ) ;
#21167 = DIRECTION ( 'NONE',  ( 0.000000000000000000, 1.000000000000000000, 3.491481338843130594E-15 ) ) ;
#21168 = DIRECTION ( 'NONE',  ( -1.000000000000000000, -3.054025858079668409E-16, 2.042474015755241579E-16 ) ) ;
#21169 = B_SPLINE_CURVE_WITH_KNOTS ( 'NONE', 3,
 ( #18204, #27845, #25456, #6156, #22469, #15807 ),
 .UNSPECIFIED., .F., .F.,
 ( 4, 2, 4 ),
 ( 0.000000000000000000, 0.0001620412083492953114, 0.0003240824166985906227 ),
 .UNSPECIFIED. ) ;
#21170 = EDGE_CURVE ( 'NONE', #10512, #24580, #31028, .T. ) ;
#21171 = DIRECTION ( 'NONE',  ( 0.000000000000000000, 0.8914544820233750722, 0.4531102586351760109 ) ) ;
#21172 = CARTESIAN_POINT ( 'NONE',  ( 58.75000000000002132, -0.6121634413826990695, 1.877732920581024700 ) ) ;
#21174 = CARTESIAN_POINT ( 'NONE',  ( -54.39999999999999147, 1.433333333333330906, 4.054078878802625852 ) ) ;
#21173 = CARTESIAN_POINT ( 'NONE',  ( 58.72200907981793705, -0.5299537992501781591, -1.799145225589202424 ) ) ;
#21175 = CARTESIAN_POINT ( 'NONE',  ( -59.63966108275621281, -2.141766704520198239, 1.560556113508256182 ) ) ;
#21176 = CARTESIAN_POINT ( 'NONE',  ( 46.89999999999999858, -4.241634596362394483, 1.073358427932564529 ) ) ;
#21177 = CYLINDRICAL_SURFACE ( 'NONE', #3168, 0.05000000000000012768 ) ;
#21178 = CARTESIAN_POINT ( 'NONE',  ( 48.00000000000001421, -3.908336260473453727, -1.238913909466087482 ) ) ;
#21179 = ORIENTED_EDGE ( 'NONE', *, *, #11797, .F. ) ;
#21180 = CIRCLE ( 'NONE', #7514, 4.000000000000022204 ) ;
#21181 = CIRCLE ( 'NONE', #26218, 1.875000000000001776 ) ;
#21182 = EDGE_LOOP ( 'NONE', ( #28290, #10249, #9216, #23854, #10098, #4613, #27960, #19457, #26672, #20897, #31009, #828, #11031, #23086, #28289, #840, #24611, #19843, #12378, #28992, #28841, #19548 ) ) ;
#21183 = CARTESIAN_POINT ( 'NONE',  ( 51.83857334934266703, 0.3198555306840176748, -4.342911177030791769 ) ) ;
#21184 = ORIENTED_EDGE ( 'NONE', *, *, #6438, .F. ) ;
#21185 = CARTESIAN_POINT ( 'NONE',  ( 52.10572631149718603, 8.700000001568275465, 2.049999999999818190 ) ) ;
#21186 = B_SPLINE_CURVE_WITH_KNOTS ( 'NONE', 3,
 ( #656, #54, #4956, #5417, #5251, #15073, #29328, #22062, #3043, #7639, #24275, #7329, #12686, #2587, #21918, #2884 ),
 .UNSPECIFIED., .F., .F.,
 ( 4, 2, 2, 2, 2, 2, 2, 4 ),
 ( 0.000000000000000000, 0.0004351083927046461137, 0.0008702167854092922273, 0.001740433570818584455, 0.002175541963523229972, 0.002610650356227875706, 0.003045758748932521440, 0.003480867141637167175 ),
 .UNSPECIFIED. ) ;
#21187 = CARTESIAN_POINT ( 'NONE',  ( -56.65835481156724285, -3.238593381231841928, -2.874284765127022467 ) ) ;
#21189 = CARTESIAN_POINT ( 'NONE',  ( 50.91898013251472577, -3.908336255397554915, -1.238913925478770661 ) ) ;
#21188 = DIRECTION ( 'NONE',  ( 0.03489949670250097613, 0.9993908270190957621, 0.000000000000000000 ) ) ;
#21190 = EDGE_LOOP ( 'NONE', ( #1704, #22242, #22523, #1659, #25323, #24629, #7113 ) ) ;
#21191 = DIRECTION ( 'NONE',  ( 0.000000000000000000, 0.000000000000000000, -1.000000000000000000 ) ) ;
#21192 = ORIENTED_EDGE ( 'NONE', *, *, #487, .F. ) ;
#21193 = ADVANCED_FACE ( 'NONE', ( #30181 ), #19530, .T. ) ;
#21194 = DIRECTION ( 'NONE',  ( -1.000000000000000000, 0.000000000000000000, 0.000000000000000000 ) ) ;
#21195 = VERTEX_POINT ( 'NONE', #11179 ) ;
#21197 = CARTESIAN_POINT ( 'NONE',  ( -35.85663232820584057, -0.9159215771380563309, 4.311190327365815200 ) ) ;
#21196 = CARTESIAN_POINT ( 'NONE',  ( 50.38490132722630932, 1.114141714781645254, 3.896173399896523559 ) ) ;
#21198 = ORIENTED_EDGE ( 'NONE', *, *, #10472, .T. ) ;
#21199 = CARTESIAN_POINT ( 'NONE',  ( 53.35811189124944320, 7.919971434358604512, 1.887106088948682592 ) ) ;
#21200 = CARTESIAN_POINT ( 'NONE',  ( 58.75000000000000000, 1.932246131438033254, -0.4087173687832941216 ) ) ;
#21201 = CARTESIAN_POINT ( 'NONE',  ( -54.49181037333889321, -1.522049374736507144, -3.314263409011525940 ) ) ;
#21202 = CARTESIAN_POINT ( 'NONE',  ( 50.25000000000001421, 0.5380862305914526633, -1.858165151417984218 ) ) ;
#21203 = CARTESIAN_POINT ( 'NONE',  ( -59.82202994616204705, -4.156921938165296204, -2.272478542645976661E-13 ) ) ;
#21204 = B_SPLINE_CURVE_WITH_KNOTS ( 'NONE', 3,
 ( #26512, #30629, #28270, #13830, #4520, #11801 ),
 .UNSPECIFIED., .F., .F.,
 ( 4, 2, 4 ),
 ( 0.000000000000000000, 0.0001000270069601567446, 0.0002000540139203134892 ),
 .UNSPECIFIED. ) ;
#21205 = CARTESIAN_POINT ( 'NONE',  ( 51.80000000000001137, 1.280326109884211361, 4.104114837514009295 ) ) ;
#21206 = MECHANICAL_DESIGN_GEOMETRIC_PRESENTATION_REPRESENTATION (  '', ( #16140 ), #6025 ) ;
#21207 = AXIS2_PLACEMENT_3D ( 'NONE', #18906, #11923, #23666 ) ;
#21208 = EDGE_CURVE ( 'NONE', #28852, #624, #25964, .T. ) ;
#21209 = CARTESIAN_POINT ( 'NONE',  ( -60.48535533905928219, 1.968299342331293196E-15, 6.674684237050104391E-16 ) ) ;
#21210 = CARTESIAN_POINT ( 'NONE',  ( 50.40000000000001279, 0.6462379109120997001, -4.048750000000022276 ) ) ;
#21211 = CARTESIAN_POINT ( 'NONE',  ( -56.98542740578360366, -3.725040285533366191, 1.239922660687670986 ) ) ;
#21212 = CARTESIAN_POINT ( 'NONE',  ( -55.61505354137802470, 3.400000000000011902, -0.9110272542660020623 ) ) ;
#21213 = ORIENTED_EDGE ( 'NONE', *, *, #7165, .F. ) ;
#21214 = CARTESIAN_POINT ( 'NONE',  ( 58.65000000000001990, 6.143261415694495821E-13, 3.111507638930570854E-58 ) ) ;
#21215 = CARTESIAN_POINT ( 'NONE',  ( -59.49819002796308354, 3.306248072576822405, -1.473410355870489630 ) ) ;
#21216 = CARTESIAN_POINT ( 'NONE',  ( -36.39645873810206211, 0.5233326973447959274, 5.388419908789453316 ) ) ;
#21217 = FACE_OUTER_BOUND ( 'NONE', #31126, .T. ) ;
#21218 = ORIENTED_EDGE ( 'NONE', *, *, #21109, .T. ) ;
#21219 = CARTESIAN_POINT ( 'NONE',  ( -57.12499999999997868, -6.418945959278930492E-15, 3.399999999999796518 ) ) ;
#21220 = ORIENTED_EDGE ( 'NONE', *, *, #24488, .T. ) ;
#21221 = CARTESIAN_POINT ( 'NONE',  ( 15.03925126672132784, 4.945493884734782242, 1.606888370749786521 ) ) ;
#21223 = CARTESIAN_POINT ( 'NONE',  ( 58.72427158855744267, -1.293556822995290512, 1.357477749118862542 ) ) ;
#21222 = CARTESIAN_POINT ( 'NONE',  ( 58.75000000694006275, 0.9860766835998435731, -1.658042653847561887 ) ) ;
#21224 = ORIENTED_EDGE ( 'NONE', *, *, #14395, .T. ) ;
#21225 = DIRECTION ( 'NONE',  ( 1.057355261547768637E-14, 0.000000000000000000, 1.000000000000000000 ) ) ;
#21226 =( GEOMETRIC_REPRESENTATION_CONTEXT ( 3 ) GLOBAL_UNCERTAINTY_ASSIGNED_CONTEXT ( ( #27224 ) ) GLOBAL_UNIT_ASSIGNED_CONTEXT ( ( #21276, #8878, #11110 ) ) REPRESENTATION_CONTEXT ( 'NONE', 'WORKASPACE' ) );
#21227 = EDGE_CURVE ( 'NONE', #7031, #19651, #13314, .T. ) ;
#21228 = DIRECTION ( 'NONE',  ( 0.000000000000000000, 1.000000000000000000, 0.000000000000000000 ) ) ;
#21230 = CARTESIAN_POINT ( 'NONE',  ( 58.75000000000000711, 0.8980135333485337323, 1.749295403805501525 ) ) ;
#21229 = CARTESIAN_POINT ( 'NONE',  ( 51.67554083669129739, -4.150097527438617817, -1.728039211945292530 ) ) ;
#21231 = ADVANCED_FACE ( 'NONE', ( #4055 ), #6439, .T. ) ;
#21232 = ORIENTED_EDGE ( 'NONE', *, *, #25559, .T. ) ;
#21233 = CARTESIAN_POINT ( 'NONE',  ( -54.93749999999997158, -4.108500314926507357, 1.367561758111405901 ) ) ;
#21234 = CARTESIAN_POINT ( 'NONE',  ( 47.10000000000002274, -4.276948333784438283, -0.9210526315789475671 ) ) ;
#21235 = EDGE_CURVE ( 'NONE', #23968, #13697, #23959, .T. ) ;
#21236 = DIRECTION ( 'NONE',  ( 1.000000000000000000, 1.047444401652940007E-14, 0.000000000000000000 ) ) ;
#21237 = FACE_OUTER_BOUND ( 'NONE', #1557, .T. ) ;
#21238 = FACE_BOUND ( 'NONE', #7247, .T. ) ;
#21239 = CARTESIAN_POINT ( 'NONE',  ( -54.49999999999997868, 1.549999999999999600, -4.064480286580312907 ) ) ;
#21240 = ORIENTED_EDGE ( 'NONE', *, *, #19685, .F. ) ;
#21241 = EDGE_CURVE ( 'NONE', #30858, #26147, #15694, .T. ) ;
#21242 = DIRECTION ( 'NONE',  ( -1.047444401652940007E-14, 0.000000000000000000, -1.000000000000000000 ) ) ;
#21243 = CIRCLE ( 'NONE', #15660, 0.1000000000000000472 ) ;
#21244 = CARTESIAN_POINT ( 'NONE',  ( -36.30424252565904908, 3.146183597690369815, -4.141717300434357263 ) ) ;
#21245 = CARTESIAN_POINT ( 'NONE',  ( 58.75000000000002132, -0.6373668173473671095, 1.895722432253304168 ) ) ;
#21246 = DIRECTION ( 'NONE',  ( -1.000000000000000000, 1.219044193948983948E-29, -3.491481338843133355E-15 ) ) ;
#21247 = DIRECTION ( 'NONE',  ( -1.000000000000000000, -3.053848253006669023E-16, 2.042510438544995415E-16 ) ) ;
#21248 = CIRCLE ( 'NONE', #25781, 0.1500000000000001887 ) ;
#21249 = CIRCLE ( 'NONE', #14143, 0.4576450603546999840 ) ;
#21251 = DIRECTION ( 'NONE',  ( 3.489354422748178582E-15, -1.218509414717996338E-16, 1.000000000000000000 ) ) ;
#21250 = DIRECTION ( 'NONE',  ( -3.002035892788117459E-16, 0.9996898646859344595, 0.02490330187381124133 ) ) ;
#21252 = EDGE_CURVE ( 'NONE', #28206, #24348, #5142, .T. ) ;
#21254 = CIRCLE ( 'NONE', #12124, 0.05000000000000012768 ) ;
#21253 = CARTESIAN_POINT ( 'NONE',  ( 47.86761800069044881, -4.417905785811086616, -1.285520522240110930 ) ) ;
#21256 = CARTESIAN_POINT ( 'NONE',  ( -62.09999999999997300, -2.749147127886318653, -0.06848408015297871576 ) ) ;
#21255 = DIRECTION ( 'NONE',  ( 0.000000000000000000, 0.9996898646859343485, 0.02490330187381123439 ) ) ;
#21257 = ORIENTED_EDGE ( 'NONE', *, *, #14084, .T. ) ;
#21258 = DIRECTION ( 'NONE',  ( -3.002035892788117459E-16, 0.9996898646859344595, 0.02490330187381124133 ) ) ;
#21259 = CARTESIAN_POINT ( 'NONE',  ( -67.99999999999997158, -3.266925685480267300E-16, 2.202315069465532498E-15 ) ) ;
#21260 = B_SPLINE_CURVE_WITH_KNOTS ( 'NONE', 3,
 ( #16708, #5121, #4802, #24432, #10039, #23977, #2743, #12389, #22079, #14462, #19707, #14154, #23828, #2118, #9413, #11781, #2272, #11937, #21624, #31260, #29809, #20481, #17791, #20176, #8122, #30104 ),
 .UNSPECIFIED., .F., .F.,
 ( 4, 2, 2, 2, 2, 2, 2, 2, 2, 2, 2, 2, 4 ),
 ( -0.001582486880272674767, -0.001533040430800264656, -0.001483593981327854545, -0.001384701082383033889, -0.001186915284493391927, -0.0007913436887141038836, -2.004971555299647767E-07, 0.0007909426944030439541, 0.001186514290182330480, 0.001384300088071973092, 0.001483192987016789411, 0.001532639436489198221, 0.001582085885961606597 ),
 .UNSPECIFIED. ) ;
#21262 = CARTESIAN_POINT ( 'NONE',  ( -36.76447480099743359, 5.297368390263413218, 1.087079755157708272 ) ) ;
#21261 = LINE ( 'NONE', #2219, #5906 ) ;
#21263 = CARTESIAN_POINT ( 'NONE',  ( 15.49676243306310219, -4.963067629822646154, 1.552801941062276425 ) ) ;
#21264 = ORIENTED_EDGE ( 'NONE', *, *, #7852, .F. ) ;
#21265 = VERTEX_POINT ( 'NONE', #2473 ) ;
#21266 = FACE_OUTER_BOUND ( 'NONE', #24257, .T. ) ;
#21267 = CARTESIAN_POINT ( 'NONE',  ( 57.05000000000001847, 0.7794871794871796045, -1.732743413496389939 ) ) ;
#21268 = ADVANCED_FACE ( 'NONE', ( #4831 ), #27503, .T. ) ;
#21269 = EDGE_LOOP ( 'NONE', ( #8164, #19383, #19156, #21045, #1007 ) ) ;
#21270 = EDGE_CURVE ( 'NONE', #10008, #4687, #212, .T. ) ;
#21271 = FACE_OUTER_BOUND ( 'NONE', #5627, .T. ) ;
#21272 = ORIENTED_EDGE ( 'NONE', *, *, #13024, .F. ) ;
#21273 = EDGE_CURVE ( 'NONE', #27565, #9758, #4363, .T. ) ;
#21274 = CARTESIAN_POINT ( 'NONE',  ( 58.73379417893114152, 1.873409305146914283, -0.08040888200754815751 ) ) ;
#21275 = ORIENTED_EDGE ( 'NONE', *, *, #16608, .F. ) ;
#21276 =( LENGTH_UNIT ( ) NAMED_UNIT ( * ) SI_UNIT ( .MILLI., .METRE. ) );
#21277 = CARTESIAN_POINT ( 'NONE',  ( 64.25000000000001421, 1.163569835200988601E-28, -2.243276760206714411E-13 ) ) ;
#21278 = ORIENTED_EDGE ( 'NONE', *, *, #20319, .T. ) ;
#21279 = ORIENTED_EDGE ( 'NONE', *, *, #26257, .F. ) ;
#21280 = AXIS2_PLACEMENT_3D ( 'NONE', #20983, #13989, #16073 ) ;
#21281 = EDGE_LOOP ( 'NONE', ( #13459, #7309 ) ) ;
#21282 = AXIS2_PLACEMENT_3D ( 'NONE', #19749, #10372, #9918 ) ;
#21283 = CARTESIAN_POINT ( 'NONE',  ( -59.12499999999996447, -2.944486372867076707, -1.700000000000220446 ) ) ;
#21284 = CARTESIAN_POINT ( 'NONE',  ( -57.68749999999996447, 0.7533615035078072841, -3.673546848079177085 ) ) ;
#21285 = CARTESIAN_POINT ( 'NONE',  ( 22.20257169554297150, 7.242789023567405060, -1.425000000000076872 ) ) ;
#21286 = CARTESIAN_POINT ( 'NONE',  ( 58.75000000000002132, 6.153735859711025284E-13, 3.111507638930570854E-58 ) ) ;
#21287 = CARTESIAN_POINT ( 'NONE',  ( -58.37486116251334067, -1.737685414808511020, 3.471684241605569099 ) ) ;
#21289 = CARTESIAN_POINT ( 'NONE',  ( -44.59999999999996589, 1.400000000000021450, -3.363870538531645860 ) ) ;
#21288 = CARTESIAN_POINT ( 'NONE',  ( -36.89831264271882105, 5.047763082740440055, -1.943828653492478242 ) ) ;
#21290 = EDGE_CURVE ( 'NONE', #20300, #7995, #27480, .T. ) ;
#21291 = CARTESIAN_POINT ( 'NONE',  ( 46.99404308269125607, -4.272100939101181716, 0.9440912809989528975 ) ) ;
#21292 = DIRECTION ( 'NONE',  ( 0.000000000000000000, -1.000000000000000000, 0.000000000000000000 ) ) ;
#21293 = FACE_OUTER_BOUND ( 'NONE', #21335, .T. ) ;
#21294 = CARTESIAN_POINT ( 'NONE',  ( 58.74160516400029763, -1.668397168087478510, -0.8556415768453068393 ) ) ;
#21295 = CARTESIAN_POINT ( 'NONE',  ( -54.49999999999997868, 8.366749974758489177E-15, -2.216533082070116467E-13 ) ) ;
#21296 = EDGE_CURVE ( 'NONE', #9375, #10212, #9752, .T. ) ;
#21297 = CARTESIAN_POINT ( 'NONE',  ( 53.14824221617038802, 8.298223012065058413, 2.049999999999815081 ) ) ;
#21298 = ORIENTED_EDGE ( 'NONE', *, *, #15150, .T. ) ;
#21300 = FACE_OUTER_BOUND ( 'NONE', #30220, .T. ) ;
#21299 = CARTESIAN_POINT ( 'NONE',  ( 50.59602332238209499, -0.1408342061598474859, 0.8215393206232036727 ) ) ;
#21301 = CARTESIAN_POINT ( 'NONE',  ( -61.34999999999997300, -2.614490477541997926, 0.4599799668244957118 ) ) ;
#21302 = VECTOR ( 'NONE', #7976, 1000.000000000000114 ) ;
#21303 = B_SPLINE_CURVE_WITH_KNOTS ( 'NONE', 3,
 ( #5113, #24571, #10491, #5730, #5423, #15381 ),
 .UNSPECIFIED., .F., .F.,
 ( 4, 2, 4 ),
 ( 0.000000000000000000, 0.0003974125641964876884, 0.0007948251283929753767 ),
 .UNSPECIFIED. ) ;
#21304 = ORIENTED_EDGE ( 'NONE', *, *, #28431, .T. ) ;
#21305 = CARTESIAN_POINT ( 'NONE',  ( 58.75000000000002132, -0.5380862305903428844, -2.008165151418244143 ) ) ;
#21306 = CARTESIAN_POINT ( 'NONE',  ( 60.82166330297963697, 0.6500000603371848262, -1.489337074527656180 ) ) ;
#21307 = CARTESIAN_POINT ( 'NONE',  ( -60.31249999999996447, 3.925981830489463142, -1.997632844132843428E-13 ) ) ;
#21308 = EDGE_LOOP ( 'NONE', ( #25688, #11288 ) ) ;
#21309 = ORIENTED_EDGE ( 'NONE', *, *, #24815, .F. ) ;
#21310 = CARTESIAN_POINT ( 'NONE',  ( 15.17214319754861229, 4.804073785499177518, 2.042134698606610677 ) ) ;
#21311 = ORIENTED_EDGE ( 'NONE', *, *, #25422, .T. ) ;
#21312 = CARTESIAN_POINT ( 'NONE',  ( 58.65263613458529335, -1.589467873454749158, 0.9947326234267183098 ) ) ;
#21313 = CARTESIAN_POINT ( 'NONE',  ( -54.50952994616204705, -3.117691453623963938, -1.800000000000204770 ) ) ;
#21314 = ORIENTED_EDGE ( 'NONE', *, *, #24978, .T. ) ;
#21315 = CARTESIAN_POINT ( 'NONE',  ( 17.21035195517767846, 24.59258869922086532, 0.000000000000000000 ) ) ;
#21316 = CARTESIAN_POINT ( 'NONE',  ( 58.66107449606942481, -1.874988011598432092, -0.03390886286852046877 ) ) ;
#21317 = CYLINDRICAL_SURFACE ( 'NONE', #21792, 0.1000000000000000472 ) ;
#21318 = VERTEX_POINT ( 'NONE', #21484 ) ;
#21319 = ORIENTED_EDGE ( 'NONE', *, *, #21290, .F. ) ;
#21320 = CARTESIAN_POINT ( 'NONE',  ( -58.68749999999997158, -4.108500314926509134, 1.367561758111400128 ) ) ;
#21321 = CARTESIAN_POINT ( 'NONE',  ( -62.09999999999997300, -2.729900678946055148, 0.2118983792693960311 ) ) ;
#21322 = DIRECTION ( 'NONE',  ( 5.713464585390589802E-15, -0.5454670984325608041, -0.8381322357048218707 ) ) ;
#21323 = VERTEX_POINT ( 'NONE', #28593 ) ;
#21324 = B_SPLINE_CURVE_WITH_KNOTS ( 'NONE', 3,
 ( #22967, #20447, #1257, #13597, #29929, #5870, #30072, #18376, #20611, #13434, #20764, #23134, #1423, #8093, #11083, #8390 ),
 .UNSPECIFIED., .F., .F.,
 ( 4, 3, 3, 3, 3, 4 ),
 ( 0.000000000000000000, 3.843454199181275667E-05, 7.602611568626176531E-05, 0.0001118455301991773924, 0.0001459326773459512306, 0.0001653157283245149816 ),
 .UNSPECIFIED. ) ;
#21325 = DIRECTION ( 'NONE',  ( -0.8262273428075421755, -0.5633368246415177971, 0.000000000000000000 ) ) ;
#21326 = CARTESIAN_POINT ( 'NONE',  ( 56.95150694030147775, 0.7014737422875408912, 1.765795469766037185 ) ) ;
#21327 = CARTESIAN_POINT ( 'NONE',  ( 57.05000000000001847, 0.7794871794871796045, 1.732743413496389939 ) ) ;
#21328 = DIRECTION ( 'NONE',  ( -7.604267291953127011E-15, 0.000000000000000000, -1.000000000000000000 ) ) ;
#21329 = CARTESIAN_POINT ( 'NONE',  ( 58.72419296898096519, -0.9760445624805118570, 1.601054456121152381 ) ) ;
#21330 = EDGE_CURVE ( 'NONE', #24678, #26348, #30813, .T. ) ;
#21331 = CARTESIAN_POINT ( 'NONE',  ( -44.49999999999999289, 1.514093959731539263, 3.183260039818184506 ) ) ;
#21332 = EDGE_CURVE ( 'NONE', #560, #17756, #11551, .T. ) ;
#21333 = DIRECTION ( 'NONE',  ( 0.000000000000000000, -2.168404344971008868E-16, -1.000000000000000000 ) ) ;
#21334 = CARTESIAN_POINT ( 'NONE',  ( 61.25000000000002132, 6.415596960124259844E-13, 3.111507638930570854E-58 ) ) ;
#21335 = EDGE_LOOP ( 'NONE', ( #24570, #7753, #8191, #21257 ) ) ;
#21336 = COLOUR_RGB ( '', 0.66274510, 0.83137255, 0.94901961) ;
#21337 = CIRCLE ( 'NONE', #11710, 1.875000000000001776 ) ;
#21338 = CARTESIAN_POINT ( 'NONE',  ( -54.44999999999997442, 0.000000000000000000, 0.000000000000000000 ) ) ;
#21339 = VERTEX_POINT ( 'NONE', #29797 ) ;
#21340 = CARTESIAN_POINT ( 'NONE',  ( 54.23225718638638426, 5.947176913004134313, 2.049999999999810640 ) ) ;
#21341 = CARTESIAN_POINT ( 'NONE',  ( -55.48542740578360366, -3.725040285533364859, 1.239922660687674760 ) ) ;
#21343 = CARTESIAN_POINT ( 'NONE',  ( -35.98952425903311791, 3.426725954212571423, 3.937891351789597039 ) ) ;
#21342 = CYLINDRICAL_SURFACE ( 'NONE', #19600, 0.1499999999999999667 ) ;
#21344 = ORIENTED_EDGE ( 'NONE', *, *, #5257, .T. ) ;
#21345 = VERTEX_POINT ( 'NONE', #22991 ) ;
#21346 = CARTESIAN_POINT ( 'NONE',  ( 56.95000000000001705, 0.6999999999999998446, 1.820027472320129514 ) ) ;
#21347 = ORIENTED_EDGE ( 'NONE', *, *, #11625, .T. ) ;
#21348 = EDGE_CURVE ( 'NONE', #2309, #11630, #16092, .T. ) ;
#21349 = DIRECTION ( 'NONE',  ( 0.000000000000000000, -1.065814103640152803E-14, 1.000000000000000000 ) ) ;
#21350 = ORIENTED_EDGE ( 'NONE', *, *, #11625, .F. ) ;
#21352 = CYLINDRICAL_SURFACE ( 'NONE', #23153, 2.100000000000000089 ) ;
#21351 = CARTESIAN_POINT ( 'NONE',  ( 58.66133336607565241, -1.607522887371482856, 0.9657121834149411388 ) ) ;
#21353 = ORIENTED_EDGE ( 'NONE', *, *, #21690, .T. ) ;
#21354 = CARTESIAN_POINT ( 'NONE',  ( 52.35021482935074744, 8.543783160579959457, 1.945426946893610953 ) ) ;
#21355 = CARTESIAN_POINT ( 'NONE',  ( 58.73379417893106336, 1.788763080992656462, -0.5625430232385030260 ) ) ;
#21356 = CARTESIAN_POINT ( 'NONE',  ( 48.00000000000002842, -4.387164041431067751, 1.383037119376590685 ) ) ;
#21357 = AXIS2_PLACEMENT_3D ( 'NONE', #11161, #16236, #13994 ) ;
#21358 = FACE_OUTER_BOUND ( 'NONE', #5543, .T. ) ;
#21359 = CARTESIAN_POINT ( 'NONE',  ( -58.50952994616205416, -4.643455692769885398E-15, 3.599999999999791367 ) ) ;
#21360 = CARTESIAN_POINT ( 'NONE',  ( 51.88790733220172058, 0.01048319233286296517, 4.374313010691237125 ) ) ;
#21361 = VECTOR ( 'NONE', #27288, 1000.000000000000114 ) ;
#21362 = CARTESIAN_POINT ( 'NONE',  ( -59.19999999999997442, -3.222669219888746550, 1.250136525132528931 ) ) ;
#21363 = CARTESIAN_POINT ( 'NONE',  ( -56.53335481156723574, 0.7533615035078095046, -3.673546848079178861 ) ) ;
#21364 = CARTESIAN_POINT ( 'NONE',  ( -58.04792740578360366, 3.330682475591786318, 0.6830477631804268146 ) ) ;
#21365 = EDGE_CURVE ( 'NONE', #6138, #4566, #23970, .T. ) ;
#21366 = DIRECTION ( 'NONE',  ( -1.000000000000000000, -0.000000000000000000, 3.491481338843133355E-15 ) ) ;
#21367 = EDGE_CURVE ( 'NONE', #4534, #7685, #15866, .T. ) ;
#21368 = VERTEX_POINT ( 'NONE', #17623 ) ;
#21369 = CARTESIAN_POINT ( 'NONE',  ( 51.80000000000002558, 6.475000000000061817, 1.949999999999818767 ) ) ;
#21370 = CARTESIAN_POINT ( 'NONE',  ( -36.31440869660544735, -0.05469410396133057850, 5.200000001157072838 ) ) ;
#21371 = CARTESIAN_POINT ( 'NONE',  ( 51.25000000000001421, 5.365856345722919090E-13, -1.875000000000001776 ) ) ;
#21372 = ORIENTED_EDGE ( 'NONE', *, *, #25455, .T. ) ;
#21373 = DIRECTION ( 'NONE',  ( -1.000000000000000000, 0.000000000000000000, 0.000000000000000000 ) ) ;
#21374 = ORIENTED_EDGE ( 'NONE', *, *, #13531, .T. ) ;
#21375 = DIRECTION ( 'NONE',  ( 0.5633368246414944824, 0.8262273428075580517, 0.000000000000000000 ) ) ;
#21377 = FACE_OUTER_BOUND ( 'NONE', #11975, .T. ) ;
#21376 = CARTESIAN_POINT ( 'NONE',  ( -35.85663232820584057, 1.123735532908288315, 5.289358697221541838 ) ) ;
#21378 = ORIENTED_EDGE ( 'NONE', *, *, #30738, .F. ) ;
#21379 = ORIENTED_EDGE ( 'NONE', *, *, #27672, .F. ) ;
#21380 = CYLINDRICAL_SURFACE ( 'NONE', #16944, 0.2500000000000000000 ) ;
#21381 = EDGE_CURVE ( 'NONE', #13894, #1995, #24881, .T. ) ;
#21382 = CYLINDRICAL_SURFACE ( 'NONE', #10097, 159.6997717543496833 ) ;
#21384 = CARTESIAN_POINT ( 'NONE',  ( 58.66118217212486030, 0.9521303665439819763, 1.615348343402630560 ) ) ;
#21383 = CARTESIAN_POINT ( 'NONE',  ( 58.75000000000003553, -1.800471618824212694, -1.039502773796582069 ) ) ;
#21385 = ORIENTED_EDGE ( 'NONE', *, *, #14326, .T. ) ;
#21386 = CARTESIAN_POINT ( 'NONE',  ( -60.23542740578359656, 2.936324665650206889, 2.606018187048499524 ) ) ;
#21387 = CARTESIAN_POINT ( 'NONE',  ( -57.22499999999997300, 2.964020293532818446E-15, 1.549317489258312010E-18 ) ) ;
#21388 = DIRECTION ( 'NONE',  ( -1.000000000000000000, -0.000000000000000000, 3.491481338843133355E-15 ) ) ;
#21389 =( BOUNDED_CURVE ( )  B_SPLINE_CURVE ( 2, ( #6120, #20386, #30174, #30009, #3892, #8490, #11026, #1654, #8779 ),
 .UNSPECIFIED., .F., .T. ) 
 B_SPLINE_CURVE_WITH_KNOTS ( ( 3, 2, 2, 2, 3 ),
 ( 0.6944444444444445308, 0.7037037037037037202, 0.7222222222222222099, 0.7407407407407406996, 0.7500000000000000000 ),
 .UNSPECIFIED. ) 
 CURVE ( )  GEOMETRIC_REPRESENTATION_ITEM ( )  RATIONAL_B_SPLINE_CURVE ( ( 0.9330127018922194093, 0.9330127018922197424, 1.000000000000000000, 0.8660254037844387076, 1.000000000000000000, 0.8660254037844387076, 1.000000000000000000, 0.9330127018922194093, 0.9330127018922194093 ) ) 
 REPRESENTATION_ITEM ( '' )  );
#21390 = CARTESIAN_POINT ( 'NONE',  ( -59.18749999999996447, 0.7533615035078157218, -3.673546848079175309 ) ) ;
#21392 = CARTESIAN_POINT ( 'NONE',  ( -54.49608498031047787, 1.530604779201329535, -4.051096982736679841 ) ) ;
#21391 = AXIS2_PLACEMENT_3D ( 'NONE', #21334, #28434, #11804 ) ;
#21393 = ORIENTED_EDGE ( 'NONE', *, *, #16178, .F. ) ;
#21394 = CARTESIAN_POINT ( 'NONE',  ( -57.06249999999997158, -3.238593381231830381, -2.874284765127031793 ) ) ;
#21395 = CARTESIAN_POINT ( 'NONE',  ( 48.99999999999999289, 3.490243377569955075E-16, -2.825000000000512212 ) ) ;
#21396 = CARTESIAN_POINT ( 'NONE',  ( 48.40000000000001990, 0.6304760106459518232, 3.950000000000022826 ) ) ;
#21397 = DIRECTION ( 'NONE',  ( 1.000000000000000000, 5.172273892338149033E-16, 0.000000000000000000 ) ) ;
#21398 = LINE ( 'NONE', #31025, #7853 ) ;
#21399 = EDGE_CURVE ( 'NONE', #28721, #22270, #1321, .T. ) ;
#21401 = DIRECTION ( 'NONE',  ( -0.000000000000000000, 1.000000000000000000, 0.000000000000000000 ) ) ;
#21400 = CARTESIAN_POINT ( 'NONE',  ( -55.28335481156723574, -4.108500314926509134, 1.367561758111407011 ) ) ;
#21402 = CARTESIAN_POINT ( 'NONE',  ( 47.21146949041553142, -4.227727696248180678, -1.816297733665433567 ) ) ;
#21404 = CARTESIAN_POINT ( 'NONE',  ( 50.34665981758796960, -1.329038565861417220, -3.861394075523871816 ) ) ;
#21403 = CARTESIAN_POINT ( 'NONE',  ( 50.25000000000001421, 0.5000000000005263567, 1.863080903344386030 ) ) ;
#21405 = ORIENTED_EDGE ( 'NONE', *, *, #3546, .T. ) ;
#21406 = CARTESIAN_POINT ( 'NONE',  ( 52.13000000000001677, 0.5000000000005460077, 1.718465885608440491 ) ) ;
#21407 = AXIS2_PLACEMENT_3D ( 'NONE', #19576, #2297, #2466 ) ;
#21409 = DIRECTION ( 'NONE',  ( -1.000000000000000000, -3.054025858079668409E-16, 2.042474015755241579E-16 ) ) ;
#21408 = CARTESIAN_POINT ( 'NONE',  ( 16.07279755198655025, -2.910597594660164322, -4.559461819278072703 ) ) ;
#21410 = CARTESIAN_POINT ( 'NONE',  ( 69.20000000000004547, -0.7500000000000000000, 1.988246715072631732 ) ) ;
#21411 = ORIENTED_EDGE ( 'NONE', *, *, #5441, .F. ) ;
#21412 = ORIENTED_EDGE ( 'NONE', *, *, #31187, .T. ) ;
#21413 = CARTESIAN_POINT ( 'NONE',  ( 50.34130827207516745, -1.344780351710843425, 3.858600739747801711 ) ) ;
#21414 = EDGE_CURVE ( 'NONE', #5901, #15234, #2716, .T. ) ;
#21415 = ORIENTED_EDGE ( 'NONE', *, *, #24099, .F. ) ;
#21416 = CARTESIAN_POINT ( 'NONE',  ( 56.97354279652698494, 0.7803351525568237301, -2.480154250529269522 ) ) ;
#21417 = DIRECTION ( 'NONE',  ( 1.000000000000000000, 1.047444401652940007E-14, 0.000000000000000000 ) ) ;
#21418 = ORIENTED_EDGE ( 'NONE', *, *, #25276, .T. ) ;
#21419 = CARTESIAN_POINT ( 'NONE',  ( 58.74999999999999289, 1.872332544501826845, -0.09997921184724604948 ) ) ;
#21420 = VERTEX_POINT ( 'NONE', #10946 ) ;
#21421 = CARTESIAN_POINT ( 'NONE',  ( 51.77489583516923233, -3.758927087870047146, -1.866445954014795516 ) ) ;
#21422 = ORIENTED_EDGE ( 'NONE', *, *, #16478, .F. ) ;
#21423 = EDGE_CURVE ( 'NONE', #7964, #16445, #30839, .T. ) ;
#21424 = ORIENTED_EDGE ( 'NONE', *, *, #10812, .F. ) ;
#21425 = CARTESIAN_POINT ( 'NONE',  ( -60.31249999999996447, 3.925981830489463142, -1.997632844132843428E-13 ) ) ;
#21426 = CARTESIAN_POINT ( 'NONE',  ( 48.30000000000001847, -0.6462379109120514054, 4.048750000000023164 ) ) ;
#21427 = CARTESIAN_POINT ( 'NONE',  ( 51.80000000000002558, 4.350000000000017408, 1.550321101314541927 ) ) ;
#21428 = CARTESIAN_POINT ( 'NONE',  ( -44.59999999999998721, -1.600000000000004530, 3.363870538531271936 ) ) ;
#21429 = CIRCLE ( 'NONE', #18385, 1.000000000000000000 ) ;
#21430 = DIRECTION ( 'NONE',  ( -1.000000000000000000, -0.000000000000000000, 3.491481338843133355E-15 ) ) ;
#21431 = EDGE_CURVE ( 'NONE', #5143, #12299, #27269, .T. ) ;
#21433 = DIRECTION ( 'NONE',  ( 3.384826294588897856E-15, 1.776356839400250465E-15, 1.000000000000000000 ) ) ;
#21432 = DIRECTION ( 'NONE',  ( 0.000000000000000000, 0.000000000000000000, 1.000000000000000000 ) ) ;
#21434 = EDGE_CURVE ( 'NONE', #27455, #20775, #11252, .T. ) ;
#21435 = EDGE_CURVE ( 'NONE', #17963, #26911, #11739, .T. ) ;
#21436 = CARTESIAN_POINT ( 'NONE',  ( 46.90000000000002700, -4.227689052994015206, 1.125730994152047471 ) ) ;
#21437 = CARTESIAN_POINT ( 'NONE',  ( -73.89999999999997726, -1.349581317326014052, -0.03361945752964041328 ) ) ;
#21438 = CARTESIAN_POINT ( 'NONE',  ( 15.41217651307625225, 5.027944117024030213, -1.353132643598505380 ) ) ;
#21439 = VERTEX_POINT ( 'NONE', #13618 ) ;
#21440 = DIRECTION ( 'NONE',  ( 0.000000000000000000, 0.000000000000000000, 1.000000000000000000 ) ) ;
#21441 = CARTESIAN_POINT ( 'NONE',  ( 69.20000000000001705, -0.7500000000000000000, -1.988246715074081017 ) ) ;
#21442 = ORIENTED_EDGE ( 'NONE', *, *, #6157, .T. ) ;
#21444 = CARTESIAN_POINT ( 'NONE',  ( 50.30000000000001847, -1.391941090707491835, 3.850000000000022293 ) ) ;
#21443 = CARTESIAN_POINT ( 'NONE',  ( 48.30268563551750560, -0.9333771270347004378, 3.994943142064449670 ) ) ;
#21445 = CARTESIAN_POINT ( 'NONE',  ( 54.37322582291520234, 5.989334736793181513, -2.026384253567227400 ) ) ;
#21446 = CARTESIAN_POINT ( 'NONE',  ( 59.35000000000002984, 1.401298464324817071E-42, -6.216582523810200043E-13 ) ) ;
#21447 = ORIENTED_EDGE ( 'NONE', *, *, #24207, .T. ) ;
#21448 = CARTESIAN_POINT ( 'NONE',  ( 22.72662675107781993, 7.272876594663812533, 1.424999999999920330 ) ) ;
#21449 = AXIS2_PLACEMENT_3D ( 'NONE', #28034, #3978, #20930 ) ;
#21450 = CARTESIAN_POINT ( 'NONE',  ( 51.67569715750386905, -4.150085526745833420, 1.728112049830016206 ) ) ;
#21451 = CARTESIAN_POINT ( 'NONE',  ( -54.50952994616204705, -3.117691453623963938, -1.800000000000204770 ) ) ;
#21452 = ORIENTED_EDGE ( 'NONE', *, *, #14514, .F. ) ;
#21453 = ORIENTED_EDGE ( 'NONE', *, *, #15259, .T. ) ;
#21454 = DIRECTION ( 'NONE',  ( -1.000000000000000000, -2.586136946169074517E-16, 0.000000000000000000 ) ) ;
#21455 = ORIENTED_EDGE ( 'NONE', *, *, #1043, .F. ) ;
#21456 = LINE ( 'NONE', #21930, #6074 ) ;
#21457 = CARTESIAN_POINT ( 'NONE',  ( -58.07202994616203995, 2.078460969082674747, -3.600000000000197709 ) ) ;
#21458 = EDGE_LOOP ( 'NONE', ( #27465, #8752, #23495, #1629, #25359, #3821, #6495 ) ) ;
#21459 = DIRECTION ( 'NONE',  ( 0.000000000000000000, 0.2008964009354147762, -0.9796124928211139560 ) ) ;
#21460 = DIRECTION ( 'NONE',  ( 2.459562394685749702E-16, -0.9510565162951545304, 0.3090169943749447312 ) ) ;
#21461 = EDGE_CURVE ( 'NONE', #4123, #19150, #13931, .T. ) ;
#21462 = DIRECTION ( 'NONE',  ( 0.000000000000000000, -1.000000000000000000, -0.000000000000000000 ) ) ;
#21463 = ORIENTED_EDGE ( 'NONE', *, *, #29611, .T. ) ;
#21464 = EDGE_LOOP ( 'NONE', ( #8259, #12702, #26877, #12769, #18020 ) ) ;
#21465 = DIRECTION ( 'NONE',  ( 0.000000000000000000, -0.2008964009354147484, 0.9796124928211139560 ) ) ;
#21466 = ADVANCED_FACE ( 'NONE', ( #4284 ), #23455, .T. ) ;
#21467 = CARTESIAN_POINT ( 'NONE',  ( -71.49999999999998579, -0.4218824419643727452, 2.057186234924342827 ) ) ;
#21468 = FACE_OUTER_BOUND ( 'NONE', #20649, .T. ) ;
#21469 = ORIENTED_EDGE ( 'NONE', *, *, #16270, .T. ) ;
#21470 = CARTESIAN_POINT ( 'NONE',  ( -61.14517784068949879, -2.578482729018109598, 0.8069458425966854476 ) ) ;
#21471 = CARTESIAN_POINT ( 'NONE',  ( 61.25000000000001421, 0.5000000000006414869, 1.807104036850122109 ) ) ;
#21472 = CARTESIAN_POINT ( 'NONE',  ( 48.30000000000001847, 2.428612866367529932E-14, 0.000000000000000000 ) ) ;
#21473 = FACE_OUTER_BOUND ( 'NONE', #11543, .T. ) ;
#21474 = ADVANCED_FACE ( 'NONE', ( #30410 ), #25504, .F. ) ;
#21475 = B_SPLINE_CURVE_WITH_KNOTS ( 'NONE', 3,
 ( #28842, #25713, #18288, #4020, #26307, #2076, #12063, #21416, #23934, #11741, #18441, #7154, #4755, #2227, #16818, #11891 ),
 .UNSPECIFIED., .F., .F.,
 ( 4, 3, 3, 3, 3, 4 ),
 ( 0.000000000000000000, 2.806063833126217928E-05, 6.345755872418550124E-05, 9.706205683209630718E-05, 0.0001297115041001252684, 0.0001622821609780518274 ),
 .UNSPECIFIED. ) ;
#21476 = EDGE_CURVE ( 'NONE', #17704, #28363, #24452, .T. ) ;
#21477 = CARTESIAN_POINT ( 'NONE',  ( 51.80021594609809199, -4.243814194680251894, 1.064485530476970032 ) ) ;
#21478 = CARTESIAN_POINT ( 'NONE',  ( -55.81249999999997868, -0.7533615035078013999, 3.673546848079176641 ) ) ;
#21479 = CARTESIAN_POINT ( 'NONE',  ( 51.80000000000002558, 4.350000000000017408, 1.495827530165114050 ) ) ;
#21480 = VECTOR ( 'NONE', #10265, 1000.000000000000000 ) ;
#21481 = ORIENTED_EDGE ( 'NONE', *, *, #2115, .F. ) ;
#21482 = VECTOR ( 'NONE', #16611, 1000.000000000000000 ) ;
#21483 = ORIENTED_EDGE ( 'NONE', *, *, #29061, .F. ) ;
#21484 = CARTESIAN_POINT ( 'NONE',  ( 61.00000000000002842, -0.8666666666660278739, 1.374595900215364930 ) ) ;
#21485 = ORIENTED_EDGE ( 'NONE', *, *, #18229, .F. ) ;
#21486 = CARTESIAN_POINT ( 'NONE',  ( 63.50000000000000000, 0.7500000000000000000, -1.988246715074021731 ) ) ;
#21487 = CARTESIAN_POINT ( 'NONE',  ( -60.84585481156722864, 3.673546848079181970, 0.7533615035078072841 ) ) ;
#21489 = CARTESIAN_POINT ( 'NONE',  ( -36.50489844130379424, 3.461789369942879002, 4.158232265984318055 ) ) ;
#21488 = DIRECTION ( 'NONE',  ( 0.000000000000000000, 0.000000000000000000, 1.000000000000000000 ) ) ;
#21490 = VERTEX_POINT ( 'NONE', #1443 ) ;
#21491 = ORIENTED_EDGE ( 'NONE', *, *, #5923, .T. ) ;
#21492 = VERTEX_POINT ( 'NONE', #28687 ) ;
#21493 = CYLINDRICAL_SURFACE ( 'NONE', #5966, 0.2500000000000000000 ) ;
#21494 = VERTEX_POINT ( 'NONE', #21267 ) ;
#21496 = FACE_OUTER_BOUND ( 'NONE', #23678, .T. ) ;
#21495 = CARTESIAN_POINT ( 'NONE',  ( 50.46980263351819929, 1.141995257496368987, 3.938405479918978713 ) ) ;
#21497 = ORIENTED_EDGE ( 'NONE', *, *, #30915, .F. ) ;
#21498 = DIRECTION ( 'NONE',  ( 0.000000000000000000, 0.000000000000000000, -1.000000000000000000 ) ) ;
#21499 = EDGE_CURVE ( 'NONE', #22540, #27746, #19847, .T. ) ;
#21500 = CARTESIAN_POINT ( 'NONE',  ( 57.00630022123013418, 0.7249518695496515175, 1.800067615291236711 ) ) ;
#21501 = ADVANCED_FACE ( 'NONE', ( #1591 ), #18875, .T. ) ;
#21502 = CARTESIAN_POINT ( 'NONE',  ( 15.03925126672133139, -5.086913985776138958, -1.171642053949127460 ) ) ;
#21503 = CARTESIAN_POINT ( 'NONE',  ( 57.05000000000001137, 0.7500000000000002220, -1.746008434843742796 ) ) ;
#21504 = CIRCLE ( 'NONE', #20504, 4.700000000000000178 ) ;
#21505 = ADVANCED_FACE ( 'NONE', ( #26145 ), #5766, .F. ) ;
#21506 = CARTESIAN_POINT ( 'NONE',  ( -55.94702994616203995, -2.078460969082631227, -3.600000000000205258 ) ) ;
#21507 = CARTESIAN_POINT ( 'NONE',  ( 49.00000000000000000, -0.5000000000000000000, -1.988246715073869408 ) ) ;
#21508 = LINE ( 'NONE', #19293, #30674 ) ;
#21509 = DIRECTION ( 'NONE',  ( 1.000000000000000000, 0.000000000000000000, -0.000000000000000000 ) ) ;
#21510 = AXIS2_PLACEMENT_3D ( 'NONE', #26973, #5457, #5281 ) ;
#21511 = DIRECTION ( 'NONE',  ( 0.000000000000000000, 1.000000000000000000, 0.000000000000000000 ) ) ;
#21512 = EDGE_CURVE ( 'NONE', #8618, #36, #23784, .T. ) ;
#21513 = DIRECTION ( 'NONE',  ( 1.000000000000000000, -0.000000000000000000, -1.047444401652940007E-14 ) ) ;
#21514 = AXIS2_PLACEMENT_3D ( 'NONE', #667, #26812, #19547 ) ;
#21515 = ORIENTED_EDGE ( 'NONE', *, *, #14511, .T. ) ;
#21516 = CARTESIAN_POINT ( 'NONE',  ( 57.05000000000001137, -0.8156862745098039102, -2.468735688885371982 ) ) ;
#21517 = CARTESIAN_POINT ( 'NONE',  ( -35.85663232820601820, -1.123735532908291423, 5.289358697221548944 ) ) ;
#21518 = CARTESIAN_POINT ( 'NONE',  ( 53.90752842026361691, 6.075960936770284704, -7.641258220787705557E-08 ) ) ;
#21519 = ORIENTED_EDGE ( 'NONE', *, *, #24581, .T. ) ;
#21520 = DIRECTION ( 'NONE',  ( -1.000000000000000000, 0.000000000000000000, 1.047444401652940007E-14 ) ) ;
#21521 = ORIENTED_EDGE ( 'NONE', *, *, #8089, .T. ) ;
#21522 = VECTOR ( 'NONE', #25136, 1000.000000000000000 ) ;
#21524 = CARTESIAN_POINT ( 'NONE',  ( 41.48619405471885102, -151.3359592902621955, 1.949999999999835865 ) ) ;
#21523 = CARTESIAN_POINT ( 'NONE',  ( 51.03947097432633484, -4.379874851678565939, -1.406750166670766689 ) ) ;
#21525 = B_SPLINE_SURFACE_WITH_KNOTS ( 'NONE', 3, 1, ( 
 ( #31294, #7545 ),
 ( #5005, #16892 ),
 ( #19426, #29071 ),
 ( #12139, #24011 ),
 ( #2776, #19281 ),
 ( #26847, #24326 ),
 ( #14662, #26711 ),
 ( #2943, #2313 ),
 ( #24177, #5155 ) ),
 .UNSPECIFIED., .F., .F., .F.,
 ( 4, 1, 1, 1, 1, 1, 4 ),
 ( 2, 2 ),
 ( 0.000000000000000000, 0.08990530927501938496, 0.2069505209790863942, 0.2957249676700259844, 0.5865340158044511920, 0.7553074047937105018, 0.9940797213269729760 ),
 ( 0.000000000000000000, 1.000000000000000000 ),
 .UNSPECIFIED. ) ;
#21526 = EDGE_LOOP ( 'NONE', ( #20477, #23311, #21929, #28642 ) ) ;
#21527 = ORIENTED_EDGE ( 'NONE', *, *, #8420, .T. ) ;
#21528 = LINE ( 'NONE', #2668, #7786 ) ;
#21529 = LINE ( 'NONE', #28482, #3525 ) ;
#21531 = CARTESIAN_POINT ( 'NONE',  ( 34.50000000000001421, 3.245314017740485962E-16, 2.649999999999999911 ) ) ;
#21530 = DIRECTION ( 'NONE',  ( -3.002035892788116966E-16, 0.9996898646859343485, 0.02490330187381124133 ) ) ;
#21532 = VERTEX_POINT ( 'NONE', #15850 ) ;
#21533 = CARTESIAN_POINT ( 'NONE',  ( -55.24999999999997868, 3.673546848079180638, 0.7533615035078055078 ) ) ;
#21534 = CARTESIAN_POINT ( 'NONE',  ( 61.23883361641895817, 0.8947175514080812908, 1.757895546655339869 ) ) ;
#21535 = CARTESIAN_POINT ( 'NONE',  ( 46.99306361170634716, -4.271975761602691435, -0.9446694106403947799 ) ) ;
#21536 = AXIS2_PLACEMENT_3D ( 'NONE', #18896, #2094, #6847 ) ;
#21537 = CARTESIAN_POINT ( 'NONE',  ( -36.89831264271879263, 3.408535483610504180, 4.200031884472282151 ) ) ;
#21538 = EDGE_CURVE ( 'NONE', #28113, #23361, #28504, .T. ) ;
#21539 = AXIS2_PLACEMENT_3D ( 'NONE', #4009, #13797, #23335 ) ;
#21540 = CARTESIAN_POINT ( 'NONE',  ( -61.36728013402707660, -2.617907752630248108, -0.6089896480292835701 ) ) ;
#21541 = FACE_OUTER_BOUND ( 'NONE', #9737, .T. ) ;
#21542 = EDGE_CURVE ( 'NONE', #29879, #29844, #22950, .T. ) ;
#21543 = CARTESIAN_POINT ( 'NONE',  ( 58.65000000000000568, 1.469015551796266195, 1.320082690054878549 ) ) ;
#21544 = TOROIDAL_SURFACE ( 'NONE', #22633, 2.150000000000000355, 0.05000000000000000278 ) ;
#21545 = ORIENTED_EDGE ( 'NONE', *, *, #476, .F. ) ;
#21546 = AXIS2_PLACEMENT_3D ( 'NONE', #27797, #12785, #8057 ) ;
#21547 = CARTESIAN_POINT ( 'NONE',  ( -57.24999999999996447, -2.489203624310589280, 2.804704140674913138 ) ) ;
#21548 = CIRCLE ( 'NONE', #3818, 0.09999999999999997780 ) ;
#21549 = CARTESIAN_POINT ( 'NONE',  ( 15.29384114148387397, -3.378548217643446705, 3.972894518062632940 ) ) ;
#21550 = CARTESIAN_POINT ( 'NONE',  ( 48.50000000000002132, 1.426739617975221641, -3.843750000000023093 ) ) ;
#21551 = DIRECTION ( 'NONE',  ( 1.000000000000000000, -0.000000000000000000, -1.047444401652940007E-14 ) ) ;
#21552 = CARTESIAN_POINT ( 'NONE',  ( 50.83686442967773900, 8.734989671305513070, 2.049999999999822631 ) ) ;
#21553 = EDGE_CURVE ( 'NONE', #5904, #10453, #30562, .T. ) ;
#21555 = CARTESIAN_POINT ( 'NONE',  ( 58.75000000000004263, -1.871930101356778842, -0.6019471833004125250 ) ) ;
#21554 = CARTESIAN_POINT ( 'NONE',  ( -62.14999999999998437, 1.152747360993128871E-15, 2.207939306294521009E-15 ) ) ;
#21556 = AXIS2_PLACEMENT_3D ( 'NONE', #29425, #24520, #2997 ) ;
#21557 = CARTESIAN_POINT ( 'NONE',  ( 47.73526966676922001, -4.311876499822751896, -1.282612398564092704 ) ) ;
#21559 = LINE ( 'NONE', #23299, #12460 ) ;
#21558 = DIRECTION ( 'NONE',  ( -1.000000000000000000, -1.047444401652940007E-14, -0.000000000000000000 ) ) ;
#21560 = CIRCLE ( 'NONE', #10418, 2.750000000000000000 ) ;
#21561 = ORIENTED_EDGE ( 'NONE', *, *, #17901, .T. ) ;
#21562 = CARTESIAN_POINT ( 'NONE',  ( 58.74999999305998699, -1.856692759305439644, 0.5240691109004367298 ) ) ;
#21563 = FACE_OUTER_BOUND ( 'NONE', #16444, .T. ) ;
#21565 = FACE_OUTER_BOUND ( 'NONE', #2946, .T. ) ;
#21564 = FACE_OUTER_BOUND ( 'NONE', #4376, .T. ) ;
#21566 = CARTESIAN_POINT ( 'NONE',  ( 15.81621483022863472, -5.330414537250523388, 0.9106291984478885881 ) ) ;
#21567 = STYLED_ITEM ( 'NONE', ( #16758 ), #15127 ) ;
#21568 = VERTEX_POINT ( 'NONE', #11889 ) ;
#21569 = ORIENTED_EDGE ( 'NONE', *, *, #9569, .T. ) ;
#21570 = CARTESIAN_POINT ( 'NONE',  ( 51.16322424031762495, -0.9520424791877071247, -1.480283991513583697 ) ) ;
#21571 = VECTOR ( 'NONE', #27729, 1000.000000000000000 ) ;
#21572 =( BOUNDED_CURVE ( )  B_SPLINE_CURVE ( 2, ( #27499, #24668, #7581, #29410, #17380, #5664, #5819, #5335, #12773 ),
 .UNSPECIFIED., .F., .T. ) 
 B_SPLINE_CURVE_WITH_KNOTS ( ( 3, 2, 2, 2, 3 ),
 ( 0.5277777777777777901, 0.5370370370370370905, 0.5555555555555555802, 0.5740740740740740700, 0.5833333333333333703 ),
 .UNSPECIFIED. ) 
 CURVE ( )  GEOMETRIC_REPRESENTATION_ITEM ( )  RATIONAL_B_SPLINE_CURVE ( ( 0.9330127018922194093, 0.9330127018922194093, 1.000000000000000000, 0.8660254037844387076, 1.000000000000000000, 0.8660254037844387076, 1.000000000000000000, 0.9330127018922189652, 0.9330127018922194093 ) ) 
 REPRESENTATION_ITEM ( '' )  );
#21573 = ORIENTED_EDGE ( 'NONE', *, *, #22855, .T. ) ;
#21574 = CIRCLE ( 'NONE', #29625, 0.04999999999999994033 ) ;
#21575 = DIRECTION ( 'NONE',  ( -1.000000000000000000, -3.053848253006669023E-16, 2.042510438544995415E-16 ) ) ;
#21576 = CARTESIAN_POINT ( 'NONE',  ( 58.50000000000001421, -0.8000000000000000444, 2.421260002560650104 ) ) ;
#21577 = ORIENTED_EDGE ( 'NONE', *, *, #15945, .T. ) ;
#21578 = DIRECTION ( 'NONE',  ( 0.000000000000000000, 0.000000000000000000, -1.000000000000000000 ) ) ;
#21579 = ORIENTED_EDGE ( 'NONE', *, *, #738, .T. ) ;
#21580 = SURFACE_STYLE_USAGE ( .BOTH. , #24399 ) ;
#21581 = EDGE_CURVE ( 'NONE', #15271, #29960, #18411, .T. ) ;
#21582 = VECTOR ( 'NONE', #5903, 1000.000000000000000 ) ;
#21583 = CARTESIAN_POINT ( 'NONE',  ( -60.20655989232410832, 1.962990915244748891, -3.400000000000205969 ) ) ;
#21584 = FILL_AREA_STYLE ('',( #18882 ) ) ;
#21585 = TOROIDAL_SURFACE ( 'NONE', #14971, 2.750000000000000444, 0.05000000000000000278 ) ;
#21586 = ORIENTED_EDGE ( 'NONE', *, *, #20718, .F. ) ;
#21587 = CARTESIAN_POINT ( 'NONE',  ( -60.62499999999995737, -2.944486372867076707, -1.700000000000225775 ) ) ;
#21588 = AXIS2_PLACEMENT_3D ( 'NONE', #6083, #10672, #8139 ) ;
#21589 = FACE_OUTER_BOUND ( 'NONE', #2103, .T. ) ;
#21590 = DIRECTION ( 'NONE',  ( -2.459562394685737870E-16, 0.9510565162951500895, 0.3090169943749582204 ) ) ;
#21591 = CARTESIAN_POINT ( 'NONE',  ( 68.95000000000003126, 1.401298464324817071E-42, -7.222129149397022450E-13 ) ) ;
#21592 = AXIS2_PLACEMENT_3D ( 'NONE', #6587, #3725, #18468 ) ;
#21593 = LINE ( 'NONE', #14127, #23068 ) ;
#21594 = AXIS2_PLACEMENT_3D ( 'NONE', #10847, #18306, #6262 ) ;
#21595 = CONICAL_SURFACE ( 'NONE', #16000, 2.150000000000000355, 0.03277514440407566787 ) ;
#21596 = EDGE_CURVE ( 'NONE', #67, #8224, #3524, .T. ) ;
#21597 = AXIS2_PLACEMENT_3D ( 'NONE', #11127, #8898, #8736 ) ;
#21599 = CARTESIAN_POINT ( 'NONE',  ( 51.76858160943182696, 4.130187818440810510, -1.964805969893994586 ) ) ;
#21598 = DIRECTION ( 'NONE',  ( 1.040834085586084257E-14, 0.000000000000000000, 1.000000000000000000 ) ) ;
#21600 = CARTESIAN_POINT ( 'NONE',  ( 47.09104525948219333, 9.165979422395388099, 2.049999999999835953 ) ) ;
#21601 = CYLINDRICAL_SURFACE ( 'NONE', #25579, 0.05000000000000012768 ) ;
#21602 = DIRECTION ( 'NONE',  ( 0.000000000000000000, 0.000000000000000000, -1.000000000000000000 ) ) ;
#21603 = VERTEX_POINT ( 'NONE', #28985 ) ;
#21604 = DIRECTION ( 'NONE',  ( 0.000000000000000000, -0.5333333333333335480, 0.8459051693633012903 ) ) ;
#21605 = CARTESIAN_POINT ( 'NONE',  ( 52.41144973999026746, 8.636710922408726177, 2.049999999999818190 ) ) ;
#21606 = AXIS2_PLACEMENT_3D ( 'NONE', #18143, #22570, #12734 ) ;
#21608 = CARTESIAN_POINT ( 'NONE',  ( 50.35335635708054269, -1.310522848978943555, 3.864668279552718300 ) ) ;
#21607 = CARTESIAN_POINT ( 'NONE',  ( 58.65000000000004121, -1.872332544500605378, 0.09997921184723741750 ) ) ;
#21609 = EDGE_CURVE ( 'NONE', #17628, #25335, #30425, .T. ) ;
#21610 = CARTESIAN_POINT ( 'NONE',  ( 54.21132576206891684, 6.699808777935940540, -2.050000000000189004 ) ) ;
#21611 = VECTOR ( 'NONE', #3691, 1000.000000000000000 ) ;
#21612 = CARTESIAN_POINT ( 'NONE',  ( 51.03629145313043125, -3.908336260473452839, -1.238913909466098362 ) ) ;
#21613 = AXIS2_PLACEMENT_3D ( 'NONE', #5218, #15035, #15341 ) ;
#21614 = AXIS2_PLACEMENT_3D ( 'NONE', #11239, #30884, #23615 ) ;
#21615 = ORIENTED_EDGE ( 'NONE', *, *, #1110, .T. ) ;
#21616 = CARTESIAN_POINT ( 'NONE',  ( 23.27131915274574325, 6.595123925190213399, 1.424999999999919220 ) ) ;
#21617 = CARTESIAN_POINT ( 'NONE',  ( -55.69702994616204705, 4.156921938165313080, -1.827997107644302771E-13 ) ) ;
#21618 = ORIENTED_EDGE ( 'NONE', *, *, #20650, .F. ) ;
#21619 = AXIS2_PLACEMENT_3D ( 'NONE', #2096, #16686, #31064 ) ;
#21620 = ORIENTED_EDGE ( 'NONE', *, *, #15827, .F. ) ;
#21621 = CARTESIAN_POINT ( 'NONE',  ( 15.41217651307625225, 4.863043649742707863, 1.860644097022760013 ) ) ;
#21622 = ORIENTED_EDGE ( 'NONE', *, *, #5161, .F. ) ;
#21623 = AXIS2_PLACEMENT_3D ( 'NONE', #3031, #5406, #24409 ) ;
#21624 = CARTESIAN_POINT ( 'NONE',  ( 51.89870775422352267, 4.414556427217972256, -1.294251603339130918 ) ) ;
#21625 = EDGE_CURVE ( 'NONE', #19589, #26980, #27189, .T. ) ;
#21626 = CARTESIAN_POINT ( 'NONE',  ( -55.19702994616203284, -2.078460969082631227, -3.600000000000202593 ) ) ;
#21627 = ORIENTED_EDGE ( 'NONE', *, *, #19161, .T. ) ;
#21628 = LINE ( 'NONE', #16378, #29230 ) ;
#21629 = AXIS2_PLACEMENT_3D ( 'NONE', #20914, #9030, #4267 ) ;
#21630 = AXIS2_PLACEMENT_3D ( 'NONE', #26037, #9888, #9431 ) ;
#21631 = CARTESIAN_POINT ( 'NONE',  ( -59.19495429951913223, -2.548385458854336871, -0.9469503383366065785 ) ) ;
#21632 = EDGE_CURVE ( 'NONE', #10205, #1939, #12818, .T. ) ;
#21633 = CARTESIAN_POINT ( 'NONE',  ( 28.70703846264724390, 5.747922415052714840, 2.049999999999641442 ) ) ;
#21634 = ORIENTED_EDGE ( 'NONE', *, *, #6982, .T. ) ;
#21635 = FACE_OUTER_BOUND ( 'NONE', #30604, .T. ) ;
#21636 = FACE_OUTER_BOUND ( 'NONE', #29645, .T. ) ;
#21637 = CARTESIAN_POINT ( 'NONE',  ( 58.66122797211853879, -0.9232791089885744595, -1.632010475558218099 ) ) ;
#21638 = ORIENTED_EDGE ( 'NONE', *, *, #21632, .F. ) ;
#21639 = CIRCLE ( 'NONE', #3879, 2.249352573995730520 ) ;
#21640 = DIRECTION ( 'NONE',  ( 3.384826294588897856E-15, 0.000000000000000000, 1.000000000000000000 ) ) ;
#21641 = CARTESIAN_POINT ( 'NONE',  ( 58.75000000000002132, 6.153735859711025284E-13, 3.111507638930570854E-58 ) ) ;
#21642 = CIRCLE ( 'NONE', #7959, 0.7375000000000040412 ) ;
#21643 = ADVANCED_FACE ( 'NONE', ( #5224 ), #1699, .T. ) ;
#21644 = AXIS2_PLACEMENT_3D ( 'NONE', #30367, #30688, #3765 ) ;
#21646 = CARTESIAN_POINT ( 'NONE',  ( 58.75000000000002842, -0.8948927608042580584, 1.760622601995711189 ) ) ;
#21645 =( LENGTH_UNIT ( ) NAMED_UNIT ( * ) SI_UNIT ( .MILLI., .METRE. ) );
#21647 = CARTESIAN_POINT ( 'NONE',  ( 58.71182503183446499, -0.4999999999993852695, 1.820794158166703314 ) ) ;
#21648 = FACE_OUTER_BOUND ( 'NONE', #19084, .T. ) ;
#21649 = CIRCLE ( 'NONE', #11496, 0.1000000000000000472 ) ;
#21650 = CARTESIAN_POINT ( 'NONE',  ( 52.54946733419073723, 4.465216787881786331, 2.049999999999816414 ) ) ;
#21651 = CIRCLE ( 'NONE', #15031, 0.05000000000000015543 ) ;
#21652 = AXIS2_PLACEMENT_3D ( 'NONE', #3838, #13489, #23181 ) ;
#21653 = ORIENTED_EDGE ( 'NONE', *, *, #5952, .T. ) ;
#21654 = EDGE_CURVE ( 'NONE', #21439, #833, #23466, .T. ) ;
#21655 = EDGE_LOOP ( 'NONE', ( #26988, #30976, #14144, #2072 ) ) ;
#21656 = CARTESIAN_POINT ( 'NONE',  ( 58.67990267795825332, 0.5000000000006146195, -1.808383001045529292 ) ) ;
#21657 = ORIENTED_EDGE ( 'NONE', *, *, #22376, .T. ) ;
#21658 = DIRECTION ( 'NONE',  ( -1.000000000000000000, -2.586136946169074517E-16, 0.000000000000000000 ) ) ;
#21659 = CARTESIAN_POINT ( 'NONE',  ( -56.48542740578359656, 2.936324665650207333, 2.606018187048499080 ) ) ;
#21661 = CARTESIAN_POINT ( 'NONE',  ( -36.11187263677869907, 2.734387802833793124, 4.440904455451962995 ) ) ;
#21660 = FACE_OUTER_BOUND ( 'NONE', #20794, .T. ) ;
#21662 = AXIS2_PLACEMENT_3D ( 'NONE', #7118, #18684, #25946 ) ;
#21663 = ORIENTED_EDGE ( 'NONE', *, *, #17238, .T. ) ;
#21664 = ORIENTED_EDGE ( 'NONE', *, *, #21654, .T. ) ;
#21665 = DIRECTION ( 'NONE',  ( -1.000000000000000000, -1.047444401652940007E-14, -0.000000000000000000 ) ) ;
#21666 = AXIS2_PLACEMENT_3D ( 'NONE', #30703, #25632, #15680 ) ;
#21667 = ORIENTED_EDGE ( 'NONE', *, *, #10213, .F. ) ;
#21668 = DIRECTION ( 'NONE',  ( -1.000000000000000000, -0.000000000000000000, 1.047444401652940007E-14 ) ) ;
#21669 = AXIS2_PLACEMENT_3D ( 'NONE', #10137, #19801, #29435 ) ;
#21670 = ORIENTED_EDGE ( 'NONE', *, *, #30738, .T. ) ;
#21671 = CARTESIAN_POINT ( 'NONE',  ( 59.35000000000006537, 1.401298464324817071E-42, 3.499999999999379163 ) ) ;
#21672 = EDGE_CURVE ( 'NONE', #14710, #4862, #29524, .T. ) ;
#21673 = EDGE_LOOP ( 'NONE', ( #13334, #28838, #1756, #14737, #26384 ) ) ;
#21674 = CARTESIAN_POINT ( 'NONE',  ( -59.19495429951913223, 2.548385458854359964, -0.9469503383365888149 ) ) ;
#21675 = EDGE_CURVE ( 'NONE', #2569, #16545, #12327, .T. ) ;
#21676 = DIRECTION ( 'NONE',  ( 1.000000000000000000, 3.054025858079668409E-16, -2.042474015755241579E-16 ) ) ;
#21677 = DIRECTION ( 'NONE',  ( 0.000000000000000000, -1.000000000000000000, 0.000000000000000000 ) ) ;
#21678 = CARTESIAN_POINT ( 'NONE',  ( -54.26905989232411542, 2.023778652682504003E-14, -3.400000000000192646 ) ) ;
#21679 = DIRECTION ( 'NONE',  ( 9.912705577010325352E-15, 0.000000000000000000, 1.000000000000000000 ) ) ;
#21680 = FACE_OUTER_BOUND ( 'NONE', #28077, .T. ) ;
#21681 = DIRECTION ( 'NONE',  ( 3.489354422748178582E-15, -1.218509414717996338E-16, 1.000000000000000000 ) ) ;
#21682 = AXIS2_PLACEMENT_3D ( 'NONE', #9626, #1842, #16412 ) ;
#21683 = DIRECTION ( 'NONE',  ( 0.000000000000000000, 0.000000000000000000, -1.000000000000000000 ) ) ;
#21684 = CARTESIAN_POINT ( 'NONE',  ( 58.75000000000003553, -1.499837071477731820, -1.323060376181415254 ) ) ;
#21685 = ORIENTED_EDGE ( 'NONE', *, *, #27605, .T. ) ;
#21686 = EDGE_CURVE ( 'NONE', #23034, #624, #22470, .T. ) ;
#21687 = LINE ( 'NONE', #4703, #19441 ) ;
#21688 = CARTESIAN_POINT ( 'NONE',  ( 52.06628335902944826, 0.5434431642986584654, 1.794517909405660250 ) ) ;
#21689 = CARTESIAN_POINT ( 'NONE',  ( 53.94320330750939974, 6.378592095722332544, 0.8960560279709253173 ) ) ;
#21690 = EDGE_CURVE ( 'NONE', #18734, #20962, #30031, .T. ) ;
#21691 = ORIENTED_EDGE ( 'NONE', *, *, #9122, .T. ) ;
#21692 = CARTESIAN_POINT ( 'NONE',  ( -54.44999999999997442, 1.499999999999999556, 4.029888335921975262 ) ) ;
#21693 = EDGE_LOOP ( 'NONE', ( #31116, #12540, #16285, #4659 ) ) ;
#21694 = EDGE_CURVE ( 'NONE', #10712, #8546, #16919, .T. ) ;
#21695 = CARTESIAN_POINT ( 'NONE',  ( 16.07279755198631932, 0.3252614978953071168, -5.399488438498867282 ) ) ;
#21697 = CARTESIAN_POINT ( 'NONE',  ( -61.60258317630325564, -2.642987027397695865, -0.5593832590402626481 ) ) ;
#21696 = CARTESIAN_POINT ( 'NONE',  ( 58.74999999305995857, 0.9423072185563144965, -1.683452862812838235 ) ) ;
#21698 = ORIENTED_EDGE ( 'NONE', *, *, #15859, .F. ) ;
#21699 = FACE_OUTER_BOUND ( 'NONE', #29325, .T. ) ;
#21701 = CARTESIAN_POINT ( 'NONE',  ( 58.74999981404332061, 1.050697058760077685, 1.649595783783794678 ) ) ;
#21700 = CARTESIAN_POINT ( 'NONE',  ( -35.85663232820584057, 2.199885893005988358, -4.939696249117657700 ) ) ;
#21702 = EDGE_LOOP ( 'NONE', ( #9314, #12491, #12594, #19639, #30299, #12708 ) ) ;
#21703 = CARTESIAN_POINT ( 'NONE',  ( -59.98542740578359656, -3.725040285533365303, 1.239922660687675871 ) ) ;
#21704 = DIRECTION ( 'NONE',  ( 2.581436205204234006E-16, -0.9796124928211140670, -0.2008964009354148872 ) ) ;
#21705 = CARTESIAN_POINT ( 'NONE',  ( 48.99999999999999289, 3.275930187719168862E-16, -2.675000000000511857 ) ) ;
#21706 = VECTOR ( 'NONE', #30054, 1000.000000000000000 ) ;
#21707 = DIRECTION ( 'NONE',  ( 1.000000000000000000, 0.000000000000000000, -1.047444401652940007E-14 ) ) ;
#21708 = STYLED_ITEM ( 'NONE', ( #31052 ), #15356 ) ;
#21709 = CARTESIAN_POINT ( 'NONE',  ( 15.03925126672133139, -3.817150320980655209, -2.203324261490558822 ) ) ;
#21710 = CARTESIAN_POINT ( 'NONE',  ( -62.09999999999997300, 1.168016602258162478E-15, 2.197726754101795588E-15 ) ) ;
#21711 = CARTESIAN_POINT ( 'NONE',  ( -59.59999999999998721, -2.157671697750204842, 1.538490443495526216 ) ) ;
#21712 = ORIENTED_EDGE ( 'NONE', *, *, #17352, .F. ) ;
#21713 = CARTESIAN_POINT ( 'NONE',  ( 58.64999999999999858, 1.834410884276226117, 0.3880228184671293268 ) ) ;
#21714 = CARTESIAN_POINT ( 'NONE',  ( 15.49676243306307022, -3.102491976071180879, 4.173461118157664629 ) ) ;
#21715 = DIRECTION ( 'NONE',  ( 1.000000000000000000, 0.000000000000000000, -3.491481338843133355E-15 ) ) ;
#21716 = CARTESIAN_POINT ( 'NONE',  ( 31.41368619715721877, 7.411258020427958115, -1.950000000000107869 ) ) ;
#21717 = CARTESIAN_POINT ( 'NONE',  ( -62.06277111861474793, -2.675496248757341267, 0.2149375022555932713 ) ) ;
#21719 = CARTESIAN_POINT ( 'NONE',  ( 52.35020563828505402, 8.543786098496177317, -1.945426797535727781 ) ) ;
#21718 = CARTESIAN_POINT ( 'NONE',  ( -61.57740687343568453, -2.676030259482950591, 0.3736822453871994631 ) ) ;
#21720 = EDGE_CURVE ( 'NONE', #1101, #13576, #2702, .T. ) ;
#21721 = STYLED_ITEM ( 'NONE', ( #8236 ), #13430 ) ;
#21722 = CARTESIAN_POINT ( 'NONE',  ( 61.24343480274162488, -0.9192405086477845044, 1.710822371303207579 ) ) ;
#21724 = CYLINDRICAL_SURFACE ( 'NONE', #17545, 1.000000000000000000 ) ;
#21723 = LINE ( 'NONE', #26597, #1852 ) ;
#21725 = EDGE_CURVE ( 'NONE', #2222, #2592, #22029, .T. ) ;
#21726 = ORIENTED_EDGE ( 'NONE', *, *, #22072, .F. ) ;
#21727 = CIRCLE ( 'NONE', #7535, 0.1500000000000001887 ) ;
#21728 = CARTESIAN_POINT ( 'NONE',  ( 58.65000045311414567, -1.830940512616420435, 0.4044292957153704515 ) ) ;
#21729 = DIRECTION ( 'NONE',  ( 1.000000000000000000, -1.219044193948983948E-29, 3.491481338843133355E-15 ) ) ;
#21731 = CARTESIAN_POINT ( 'NONE',  ( -36.21152527658242093, 5.035245099686857628, 1.330662535294883098 ) ) ;
#21730 = CARTESIAN_POINT ( 'NONE',  ( -59.29999999999997584, 3.111192537532289304, 2.093557019620777115 ) ) ;
#21732 = LINE ( 'NONE', #22024, #14563 ) ;
#21733 = ORIENTED_EDGE ( 'NONE', *, *, #12866, .T. ) ;
#21734 = ORIENTED_EDGE ( 'NONE', *, *, #8086, .F. ) ;
#21735 = CARTESIAN_POINT ( 'NONE',  ( -57.62486116251334778, -1.737685414808515683, 3.471684241605564658 ) ) ;
#21736 = VERTEX_POINT ( 'NONE', #4753 ) ;
#21737 = CARTESIAN_POINT ( 'NONE',  ( 54.40000000000001990, 0.000000000000000000, 0.000000000000000000 ) ) ;
#21738 = DIRECTION ( 'NONE',  ( 2.085103575917242148E-15, -0.9615843008030771077, 0.2745098039215673746 ) ) ;
#21739 = CIRCLE ( 'NONE', #30286, 2.649999999999999911 ) ;
#21740 = ORIENTED_EDGE ( 'NONE', *, *, #26567, .T. ) ;
#21741 = CARTESIAN_POINT ( 'NONE',  ( -57.72499999999997300, -0.9643027244899882167, 4.702139965541347166 ) ) ;
#21742 = EDGE_LOOP ( 'NONE', ( #20823, #11478, #10409, #20984 ) ) ;
#21743 = ADVANCED_FACE ( 'NONE', ( #26 ), #20960, .T. ) ;
#21744 = CARTESIAN_POINT ( 'NONE',  ( -60.45655989232412253, -3.925981830489445379, -2.286428396510360233E-13 ) ) ;
#21745 = ORIENTED_EDGE ( 'NONE', *, *, #25922, .F. ) ;
#21746 = AXIS2_PLACEMENT_3D ( 'NONE', #18522, #2187, #16300 ) ;
#21747 = ORIENTED_EDGE ( 'NONE', *, *, #24969, .T. ) ;
#21748 = EDGE_LOOP ( 'NONE', ( #2654, #25784, #11518, #9163 ) ) ;
#21749 =( GEOMETRIC_REPRESENTATION_CONTEXT ( 3 ) GLOBAL_UNCERTAINTY_ASSIGNED_CONTEXT ( ( #6017 ) ) GLOBAL_UNIT_ASSIGNED_CONTEXT ( ( #6831, #16496, #26153 ) ) REPRESENTATION_CONTEXT ( 'NONE', 'WORKASPACE' ) );
#21750 = AXIS2_PLACEMENT_3D ( 'NONE', #10318, #5110, #21920 ) ;
#21751 = CARTESIAN_POINT ( 'NONE',  ( -55.00952994616204705, 3.117691453623994580, -1.800000000000181899 ) ) ;
#21752 = CARTESIAN_POINT ( 'NONE',  ( 53.90311770664829538, 7.548181632372875427, -2.050000000000187228 ) ) ;
#21753 = DIRECTION ( 'NONE',  ( -1.000000000000000000, -0.000000000000000000, -0.000000000000000000 ) ) ;
#21754 = FACE_OUTER_BOUND ( 'NONE', #27437, .T. ) ;
#21755 = CARTESIAN_POINT ( 'NONE',  ( 58.65000000000001990, 6.143261415694495821E-13, 3.111507638930570854E-58 ) ) ;
#21756 = AXIS2_PLACEMENT_3D ( 'NONE', #8348, #30662, #15649 ) ;
#21758 = CARTESIAN_POINT ( 'NONE',  ( -36.77443515226921278, 0.6016956010319299830, -5.375730734456574567 ) ) ;
#21757 = DIRECTION ( 'NONE',  ( -1.000000000000000000, -0.000000000000000000, -0.000000000000000000 ) ) ;
#21759 = B_SPLINE_CURVE_WITH_KNOTS ( 'NONE', 3,
 ( #4849, #12281, #2781, #14670 ),
 .UNSPECIFIED., .F., .F.,
 ( 4, 4 ),
 ( 0.000000000000000000, 0.0002896903389214072148 ),
 .UNSPECIFIED. ) ;
#21760 = CARTESIAN_POINT ( 'NONE',  ( 47.00000000000002842, -4.144693941441892626, 1.074391609828098559 ) ) ;
#21761 = CARTESIAN_POINT ( 'NONE',  ( 58.65000000000000568, 1.394635017529600507, -1.253243060177047896 ) ) ;
#21763 = DIRECTION ( 'NONE',  ( 0.000000000000000000, -0.2008964009354147484, 0.9796124928211139560 ) ) ;
#21762 = CARTESIAN_POINT ( 'NONE',  ( 54.44364453144186911, -0.0003028757502672923879, -4.365665911209477557 ) ) ;
#21764 = EDGE_CURVE ( 'NONE', #19844, #16856, #24845, .T. ) ;
#21765 = ORIENTED_EDGE ( 'NONE', *, *, #5015, .F. ) ;
#21766 =( BOUNDED_SURFACE ( )  B_SPLINE_SURFACE ( 3, 2, ( 
 ( #18461, #20379, #20529 ),
 ( #25563, #15618, #27799 ),
 ( #10549, #11162, #893 ),
 ( #20226, #6420, #5791 ),
 ( #15446, #30162, #18302 ),
 ( #8168, #3429, #29854 ),
 ( #24936, #25414, #20836 ),
 ( #1343, #3716, #6113 ),
 ( #10696, #22750, #30001 ),
 ( #8481, #20694, #30319 ) ),
 .UNSPECIFIED., .F., .F., .F. ) 
 B_SPLINE_SURFACE_WITH_KNOTS ( ( 4, 2, 2, 2, 4 ),
 ( 3, 3 ),
 ( -1.029992063861229212E-18, 0.0003537660104434874790, 0.0007075320208869760423, 0.001061298031330464714, 0.001415064041773953169 ),
 ( 0.000000000000000000, 1.000000000000000000 ),
 .UNSPECIFIED. ) 
 GEOMETRIC_REPRESENTATION_ITEM ( )  RATIONAL_B_SPLINE_SURFACE ( (
 ( 1.000000000000000000, 0.7071067811865467956, 1.000000000000000000),
 ( 1.000000000000000000, 0.7179295922952573239, 1.000000000000000000),
 ( 1.000000000000000000, 0.7246425758715731025, 1.000000000000000000),
 ( 1.000000000000000000, 0.7309548279203579302, 1.000000000000000000),
 ( 1.000000000000000000, 0.7305336397965990214, 1.000000000000000000),
 ( 1.000000000000000000, 0.7264835597184705618, 1.000000000000000000),
 ( 1.000000000000000000, 0.7229248932001940409, 1.000000000000000000),
 ( 1.000000000000000000, 0.7174039707112246367, 1.000000000000000000),
 ( 1.000000000000000000, 0.7154085637335746428, 1.000000000000000000),
 ( 1.000000000000000000, 0.7154752000627009334, 1.000000000000000000) ) ) 
 REPRESENTATION_ITEM ( '' )  SURFACE ( )  );
#21767 = CARTESIAN_POINT ( 'NONE',  ( 51.89801475736550884, 4.350000000000017408, -1.495827530165608987 ) ) ;
#21768 = CARTESIAN_POINT ( 'NONE',  ( 47.00000000000002132, -3.995252422878563969, -2.068710474281869605 ) ) ;
#21770 = CARTESIAN_POINT ( 'NONE',  ( 48.50000000000002132, -1.391941090707485396, -3.850000000000022737 ) ) ;
#21769 = CARTESIAN_POINT ( 'NONE',  ( 48.29999997184167881, -0.7900353715960748424, 4.025797886239748991 ) ) ;
#21771 = CARTESIAN_POINT ( 'NONE',  ( -58.99999999999997158, 3.673546848079179306, 0.7533615035078117250 ) ) ;
#21772 = VERTEX_POINT ( 'NONE', #29590 ) ;
#21773 = CARTESIAN_POINT ( 'NONE',  ( 58.65000000000001279, 0.6121634413823858756, 1.877732920581527631 ) ) ;
#21774 = CARTESIAN_POINT ( 'NONE',  ( -58.40835481156723574, -0.7533615035077920741, 3.673546848079180638 ) ) ;
#21775 = CIRCLE ( 'NONE', #8092, 1.875000000000001776 ) ;
#21776 = ORIENTED_EDGE ( 'NONE', *, *, #5613, .T. ) ;
#21777 = CARTESIAN_POINT ( 'NONE',  ( -54.49999999999997868, -6.102218906431378987E-14, -2.216533082070118739E-13 ) ) ;
#21778 = CARTESIAN_POINT ( 'NONE',  ( -58.44702994616205416, -2.078460969082657872, 3.599999999999784261 ) ) ;
#21779 = ORIENTED_EDGE ( 'NONE', *, *, #9587, .F. ) ;
#21780 = VERTEX_POINT ( 'NONE', #1102 ) ;
#21781 = LINE ( 'NONE', #26665, #22514 ) ;
#21782 = EDGE_LOOP ( 'NONE', ( #12050, #23003, #7166, #18329 ) ) ;
#21783 = AXIS2_PLACEMENT_3D ( 'NONE', #18297, #10840, #1497 ) ;
#21784 = FACE_OUTER_BOUND ( 'NONE', #5534, .T. ) ;
#21785 = EDGE_CURVE ( 'NONE', #5904, #6063, #2234, .T. ) ;
#21786 = CARTESIAN_POINT ( 'NONE',  ( -55.57202994616207548, 2.078460969082646770, 3.599999999999810019 ) ) ;
#21787 = EDGE_LOOP ( 'NONE', ( #24633, #24840, #2694, #3081 ) ) ;
#21788 = DIRECTION ( 'NONE',  ( -1.000000000000000000, 0.000000000000000000, -0.000000000000000000 ) ) ;
#21789 = CARTESIAN_POINT ( 'NONE',  ( 51.87416143049283335, 8.598705507415685290, -1.950000000000180256 ) ) ;
#21790 = CARTESIAN_POINT ( 'NONE',  ( 27.84544208433369405, 5.444976785341556713, 2.050000000000031353 ) ) ;
#21791 = VERTEX_POINT ( 'NONE', #956 ) ;
#21792 = AXIS2_PLACEMENT_3D ( 'NONE', #1338, #20688, #6107 ) ;
#21793 = DIRECTION ( 'NONE',  ( -3.491481338843133355E-15, -3.491481338843133355E-15, 1.000000000000000000 ) ) ;
#21794 = CARTESIAN_POINT ( 'NONE',  ( -54.49999999999997868, -1.549598385535858380, 4.064203588144675194 ) ) ;
#21795 = CARTESIAN_POINT ( 'NONE',  ( -59.35604502977157182, -3.238409345187212907, -1.039956114811810606 ) ) ;
#21796 = CARTESIAN_POINT ( 'NONE',  ( 56.98297952491088836, 0.7550874052942159187, 1.743526814789472912 ) ) ;
#21798 = CARTESIAN_POINT ( 'NONE',  ( 58.75000000000002132, 6.153735859711025284E-13, 3.111507638930570854E-58 ) ) ;
#21797 = CARTESIAN_POINT ( 'NONE',  ( -36.68866260399460799, -3.738196885377723877, 3.908481927057712024 ) ) ;
#21799 = AXIS2_PLACEMENT_3D ( 'NONE', #9879, #12251, #17021 ) ;
#21800 = CARTESIAN_POINT ( 'NONE',  ( 58.65000000000001990, 6.143261415694495821E-13, 3.111507638930570854E-58 ) ) ;
#21801 = DIRECTION ( 'NONE',  ( 0.000000000000000000, 0.000000000000000000, -1.000000000000000000 ) ) ;
#21802 = EDGE_CURVE ( 'NONE', #18960, #10212, #22771, .T. ) ;
#21803 = CARTESIAN_POINT ( 'NONE',  ( 53.29207122288457299, 4.934008984266823994, 2.049999999999814193 ) ) ;
#21804 = ORIENTED_EDGE ( 'NONE', *, *, #27633, .F. ) ;
#21805 = EDGE_CURVE ( 'NONE', #24382, #16231, #19453, .T. ) ;
#21806 = CARTESIAN_POINT ( 'NONE',  ( -59.10128028972211212, -2.331449503985936200, 1.259712628313877980 ) ) ;
#21807 = ORIENTED_EDGE ( 'NONE', *, *, #5209, .F. ) ;
#21808 = DIRECTION ( 'NONE',  ( 0.000000000000000000, 0.000000000000000000, -1.000000000000000000 ) ) ;
#21809 = CARTESIAN_POINT ( 'NONE',  ( -60.09585481156723574, 3.673546848079181970, 0.7533615035078071731 ) ) ;
#21811 = CARTESIAN_POINT ( 'NONE',  ( 51.36702623273012591, 1.002608958138273554, -1.584424273060083044 ) ) ;
#21810 = CARTESIAN_POINT ( 'NONE',  ( 15.18459684427940104, 5.377732432866634049, 0.5657657256216265251 ) ) ;
#21812 = VERTEX_POINT ( 'NONE', #18058 ) ;
#21813 = ORIENTED_EDGE ( 'NONE', *, *, #4785, .T. ) ;
#21814 = CARTESIAN_POINT ( 'NONE',  ( -54.49999999999997868, 0.000000000000000000, 0.000000000000000000 ) ) ;
#21815 = VERTEX_POINT ( 'NONE', #3162 ) ;
#21816 = FACE_OUTER_BOUND ( 'NONE', #14621, .T. ) ;
#21817 = ADVANCED_FACE ( 'NONE', ( #17892 ), #8078, .F. ) ;
#21818 = VERTEX_POINT ( 'NONE', #3632 ) ;
#21819 = CARTESIAN_POINT ( 'NONE',  ( 58.65000000000004121, -1.656314228057949034, 0.8794134543728125974 ) ) ;
#21820 = EDGE_LOOP ( 'NONE', ( #29953, #22148, #1658, #11067 ) ) ;
#21821 = CIRCLE ( 'NONE', #30902, 1.000000000000000000 ) ;
#21822 = CARTESIAN_POINT ( 'NONE',  ( 57.01079215475500206, -0.7500001437588036390, 1.746008375800299772 ) ) ;
#21823 = DIRECTION ( 'NONE',  ( 0.000000000000000000, 0.000000000000000000, 1.000000000000000000 ) ) ;
#21824 = AXIS2_PLACEMENT_3D ( 'NONE', #19934, #17871, #27363 ) ;
#21825 = CARTESIAN_POINT ( 'NONE',  ( 61.25000000000004263, -1.666164585741877424, -1.106298139389857660 ) ) ;
#21826 = CARTESIAN_POINT ( 'NONE',  ( -56.83155989232414385, -1.962990915244731571, 3.399999999999789413 ) ) ;
#21827 = EDGE_CURVE ( 'NONE', #20276, #2603, #14856, .T. ) ;
#21828 = CARTESIAN_POINT ( 'NONE',  ( 54.23625105546377512, 6.534957249981562022, -2.050000000000189004 ) ) ;
#21829 = DIRECTION ( 'NONE',  ( 0.000000000000000000, 0.000000000000000000, 1.000000000000000000 ) ) ;
#21830 = CARTESIAN_POINT ( 'NONE',  ( 50.35335635708054980, 1.310522848978987298, -3.864668279552719632 ) ) ;
#21831 = AXIS2_PLACEMENT_3D ( 'NONE', #7537, #26525, #29062 ) ;
#21832 = CARTESIAN_POINT ( 'NONE',  ( -59.36275712389306847, -2.351251615786114524, 1.344104394424739723 ) ) ;
#21833 = B_SPLINE_CURVE_WITH_KNOTS ( 'NONE', 3,
 ( #28635, #12163, #26094, #4408, #21845, #9784, #29096, #7410, #23738, #2029, #17086, #31000, #18984, #26258, #16767, #6951 ),
 .UNSPECIFIED., .F., .F.,
 ( 4, 2, 2, 2, 2, 2, 2, 4 ),
 ( 0.000000000000000000, 0.0004351083927046443789, 0.0008702167854092887579, 0.001740433570818577516, 0.002175541963523222166, 0.002610650356227867466, 0.003045758748932512333, 0.003480867141637158067 ),
 .UNSPECIFIED. ) ;
#21834 = ADVANCED_FACE ( 'NONE', ( #27702 ), #15041, .T. ) ;
#21835 = CARTESIAN_POINT ( 'NONE',  ( -59.69999999999997442, 2.455304892039244180, -1.238538609462265905 ) ) ;
#21836 = EDGE_CURVE ( 'NONE', #7967, #3082, #24980, .T. ) ;
#21837 = B_SPLINE_CURVE_WITH_KNOTS ( 'NONE', 3,
 ( #26008, #16211, #4317, #6859 ),
 .UNSPECIFIED., .F., .F.,
 ( 4, 4 ),
 ( 0.6030138259287500802, 0.6725631453485761968 ),
 .UNSPECIFIED. ) ;
#21838 = VERTEX_POINT ( 'NONE', #17417 ) ;
#21839 = ADVANCED_FACE ( 'NONE', ( #24698, #782 ), #3012, .T. ) ;
#21840 = CARTESIAN_POINT ( 'NONE',  ( 57.00000000000000711, -0.7137254901960808917, -2.500119182088006209 ) ) ;
#21842 = CARTESIAN_POINT ( 'NONE',  ( 58.65000000000001279, 1.278599783849776461, -1.371849028670597104 ) ) ;
#21841 = CARTESIAN_POINT ( 'NONE',  ( -36.58413561666738900, -3.095036031508881180, -4.435288302043747244 ) ) ;
#21843 = FACE_OUTER_BOUND ( 'NONE', #27901, .T. ) ;
#21844 = ORIENTED_EDGE ( 'NONE', *, *, #22321, .F. ) ;
#21845 = CARTESIAN_POINT ( 'NONE',  ( -36.52679053911622731, -5.349174094756211417, 0.7986533162260726071 ) ) ;
#21846 = ORIENTED_EDGE ( 'NONE', *, *, #27126, .T. ) ;
#21847 = CARTESIAN_POINT ( 'NONE',  ( -36.76447480099743359, -4.924630501335189869, 2.234249019593649077 ) ) ;
#21849 = DIRECTION ( 'NONE',  ( -0.9993908270190956511, 0.03489949670250096919, 3.491481338843132961E-15 ) ) ;
#21848 = CARTESIAN_POINT ( 'NONE',  ( 51.25952958126881498, -4.349936135048432462, -1.496764967787034717 ) ) ;
#21850 = VERTEX_POINT ( 'NONE', #24993 ) ;
#21851 = DIRECTION ( 'NONE',  ( 1.000000000000000000, 4.678365685400771632E-16, 1.520093157366894206E-16 ) ) ;
#21852 = DIRECTION ( 'NONE',  ( -0.000000000000000000, -1.000000000000000000, 0.000000000000000000 ) ) ;
#21853 = CIRCLE ( 'NONE', #8170, 0.09999999999999850675 ) ;
#21855 = CARTESIAN_POINT ( 'NONE',  ( -59.09999999999997300, -2.649999999999991918, -1.947706029260935638E-13 ) ) ;
#21854 = DIRECTION ( 'NONE',  ( -1.000000000000000000, -2.586136946169074517E-16, 0.000000000000000000 ) ) ;
#21856 = ORIENTED_EDGE ( 'NONE', *, *, #13505, .F. ) ;
#21857 = CARTESIAN_POINT ( 'NONE',  ( -59.74999999999997158, 3.673546848079180194, 0.7533615035078065070 ) ) ;
#21858 = FACE_OUTER_BOUND ( 'NONE', #27787, .T. ) ;
#21859 = CARTESIAN_POINT ( 'NONE',  ( 58.45000000000001705, 0.000000000000000000, 0.000000000000000000 ) ) ;
#21860 = CYLINDRICAL_SURFACE ( 'NONE', #24977, 4.300000000000019362 ) ;
#21861 = CIRCLE ( 'NONE', #12709, 0.2999999999999999334 ) ;
#21862 = DIRECTION ( 'NONE',  ( 1.000000000000000000, -1.219044193948983948E-29, 3.491481338843133355E-15 ) ) ;
#21863 = CARTESIAN_POINT ( 'NONE',  ( -44.49999999999997868, 8.366749974758366115E-15, -1.867384948185803131E-13 ) ) ;
#21864 = DIRECTION ( 'NONE',  ( 0.000000000000000000, 1.000000000000000000, 0.000000000000000000 ) ) ;
#21865 = EDGE_CURVE ( 'NONE', #26557, #18525, #19141, .T. ) ;
#21866 = VERTEX_POINT ( 'NONE', #22484 ) ;
#21867 = EDGE_CURVE ( 'NONE', #12847, #4765, #10449, .T. ) ;
#21868 = CARTESIAN_POINT ( 'NONE',  ( 51.80000000000001847, 6.982261990806648555E-14, -1.796574372350448449E-13 ) ) ;
#21869 = DIRECTION ( 'NONE',  ( 0.000000000000000000, 0.000000000000000000, 1.000000000000000000 ) ) ;
#21870 = FACE_OUTER_BOUND ( 'NONE', #28848, .T. ) ;
#21872 = CARTESIAN_POINT ( 'NONE',  ( 53.41816162339292617, 7.853362761740803499, -1.880937203427523574 ) ) ;
#21871 = CARTESIAN_POINT ( 'NONE',  ( -59.31908585006429036, 2.449738638601857588, -1.018617722459514763 ) ) ;
#21873 = AXIS2_PLACEMENT_3D ( 'NONE', #29239, #17351, #7551 ) ;
#21874 = CARTESIAN_POINT ( 'NONE',  ( 50.31971926781693583, 8.252744006147214151, -2.050000000000174794 ) ) ;
#21876 = CARTESIAN_POINT ( 'NONE',  ( -35.85663232820583346, -3.817150320980672529, -2.203324261490544611 ) ) ;
#21875 = CARTESIAN_POINT ( 'NONE',  ( 58.75000000000001421, 0.5811678240972331100, 1.782657835995121509 ) ) ;
#21877 = ORIENTED_EDGE ( 'NONE', *, *, #12678, .T. ) ;
#21878 = CARTESIAN_POINT ( 'NONE',  ( 58.65263613458537151, -1.792763816754253892, 0.5494533739914930770 ) ) ;
#21879 = CARTESIAN_POINT ( 'NONE',  ( 60.75000000000001421, 0.6500000000006362910, 1.489337100860648189 ) ) ;
#21881 = PLANE ( 'NONE',  #28804 ) ;
#21880 = CARTESIAN_POINT ( 'NONE',  ( -59.19184846062112371, 0.2309624077929078034, 3.875409454552792621 ) ) ;
#21882 = DIRECTION ( 'NONE',  ( 1.000000000000000000, -0.000000000000000000, -0.000000000000000000 ) ) ;
#21883 = ORIENTED_EDGE ( 'NONE', *, *, #29823, .T. ) ;
#21884 = ORIENTED_EDGE ( 'NONE', *, *, #7036, .T. ) ;
#21885 = CARTESIAN_POINT ( 'NONE',  ( 58.75000000000000711, 1.800471618824440734, 1.039502773797588597 ) ) ;
#21886 = ORIENTED_EDGE ( 'NONE', *, *, #5340, .F. ) ;
#21887 = CARTESIAN_POINT ( 'NONE',  ( 51.71308018800799289, -4.178911716362186723, 1.000646358242007983 ) ) ;
#21888 = CARTESIAN_POINT ( 'NONE',  ( 64.25000000000001421, 1.163569835200988601E-28, -1.375000000000225819 ) ) ;
#21889 = AXIS2_PLACEMENT_3D ( 'NONE', #14175, #4196, #9281 ) ;
#21890 = VERTEX_POINT ( 'NONE', #27385 ) ;
#21891 = CARTESIAN_POINT ( 'NONE',  ( -35.85663232820581214, -5.086913985776156721, -1.171642053949115914 ) ) ;
#21892 = EDGE_LOOP ( 'NONE', ( #12355, #11939 ) ) ;
#21893 = FILL_AREA_STYLE ('',( #31049 ) ) ;
#21894 = DIRECTION ( 'NONE',  ( 1.000000000000000000, 1.047444401652940007E-14, 0.000000000000000000 ) ) ;
#21895 = ORIENTED_EDGE ( 'NONE', *, *, #21434, .F. ) ;
#21896 = PRESENTATION_STYLE_ASSIGNMENT (( #14422 ) ) ;
#21897 = B_SPLINE_CURVE_WITH_KNOTS ( 'NONE', 3,
 ( #28514, #6515, #25821, #13615 ),
 .UNSPECIFIED., .F., .F.,
 ( 4, 4 ),
 ( 0.0001521069361438105792, 0.0002184312136277813138 ),
 .UNSPECIFIED. ) ;
#21898 = ADVANCED_FACE ( 'NONE', ( #3319 ), #6752, .T. ) ;
#21899 = ORIENTED_EDGE ( 'NONE', *, *, #14716, .T. ) ;
#21900 = EDGE_CURVE ( 'NONE', #11230, #23664, #28161, .T. ) ;
#21901 = CARTESIAN_POINT ( 'NONE',  ( -58.19702994616203284, -2.078460969082631227, -3.600000000000212363 ) ) ;
#21902 = EDGE_CURVE ( 'NONE', #8529, #6314, #19941, .T. ) ;
#21903 = CARTESIAN_POINT ( 'NONE',  ( 53.88135321025246327, 4.969568719840013138, -2.050000000000188560 ) ) ;
#21904 = CARTESIAN_POINT ( 'NONE',  ( -54.39999999999997726, 8.366749974758487600E-15, -2.213041600731273397E-13 ) ) ;
#21905 = DIRECTION ( 'NONE',  ( 0.9993908270190956511, -0.03489949670250096919, -3.491481338843132961E-15 ) ) ;
#21906 = DIRECTION ( 'NONE',  ( -1.047444401652940007E-14, 1.000000000000000000, 0.000000000000000000 ) ) ;
#21908 = CARTESIAN_POINT ( 'NONE',  ( -61.39959552429773026, -2.565909676969820641, -0.8403020935398156643 ) ) ;
#21907 = FACE_OUTER_BOUND ( 'NONE', #18985, .T. ) ;
#21909 =( BOUNDED_SURFACE ( )  B_SPLINE_SURFACE ( 3, 2, ( 
 ( #9353, #14399, #16651 ),
 ( #4120, #9034, #26292 ),
 ( #23443, #18708, #2213 ),
 ( #4594, #28352, #9528 ) ),
 .UNSPECIFIED., .F., .F., .T. ) 
 B_SPLINE_SURFACE_WITH_KNOTS ( ( 4, 4 ),
 ( 3, 3 ),
 ( 3.756617526051016459E-05, 0.0002104436212403357762 ),
 ( 0.000000000000000000, 1.000000000000000000 ),
 .UNSPECIFIED. ) 
 GEOMETRIC_REPRESENTATION_ITEM ( )  RATIONAL_B_SPLINE_SURFACE ( (
 ( 1.000000000000000000, 0.7071067811865965336, 1.000000000000000000),
 ( 1.000000000000000000, 0.7737094907949337852, 1.000000000000000000),
 ( 1.000000000000000000, 0.8271097373158977639, 1.000000000000000000),
 ( 1.000000000000000000, 0.8191520442890480869, 1.000000000000000000) ) ) 
 REPRESENTATION_ITEM ( '' )  SURFACE ( )  );
#21910 = CIRCLE ( 'NONE', #29458, 2.050000000000000266 ) ;
#21911 = CARTESIAN_POINT ( 'NONE',  ( 51.78416995154973534, 0.8999235898787814047, 1.360374659026170496 ) ) ;
#21912 = CARTESIAN_POINT ( 'NONE',  ( 48.46953526341861362, 1.366509374015061784, -3.854674997130605352 ) ) ;
#21914 = CARTESIAN_POINT ( 'NONE',  ( 57.03820272507597622, -0.7500000014582769436, 2.490438835250821992 ) ) ;
#21913 = CARTESIAN_POINT ( 'NONE',  ( 15.22842924604222503, 4.861582136949903266, -2.394243986685391512 ) ) ;
#21915 = EDGE_CURVE ( 'NONE', #6782, #8007, #29266, .T. ) ;
#21916 = ORIENTED_EDGE ( 'NONE', *, *, #20855, .T. ) ;
#21917 = CARTESIAN_POINT ( 'NONE',  ( 36.55000000000001847, 0.000000000000000000, 0.000000000000000000 ) ) ;
#21918 = CARTESIAN_POINT ( 'NONE',  ( -36.00201293083839005, -5.377732432866788592, -0.5657657256210414376 ) ) ;
#21920 = DIRECTION ( 'NONE',  ( -0.9993908270190956511, 0.03489949670250096919, 3.491481338843132961E-15 ) ) ;
#21919 = CARTESIAN_POINT ( 'NONE',  ( 48.45103168306561514, -1.383117500626934282, 3.859810431918025309 ) ) ;
#21921 = CARTESIAN_POINT ( 'NONE',  ( 22.06071280439821081, 8.185410187602871090, 1.949999999999922906 ) ) ;
#21922 = ORIENTED_EDGE ( 'NONE', *, *, #25669, .F. ) ;
#21923 = DIRECTION ( 'NONE',  ( -1.000000000000000000, 1.219044193948983948E-29, -3.491481338843133355E-15 ) ) ;
#21924 = ORIENTED_EDGE ( 'NONE', *, *, #28945, .T. ) ;
#21925 = CARTESIAN_POINT ( 'NONE',  ( 68.05000000000002558, 1.401298464324817071E-42, -7.127859153248258291E-13 ) ) ;
#21926 = EDGE_LOOP ( 'NONE', ( #5268, #28886, #17599, #29030, #14884 ) ) ;
#21927 = ORIENTED_EDGE ( 'NONE', *, *, #12856, .T. ) ;
#21928 = CARTESIAN_POINT ( 'NONE',  ( 15.87128154250932610, 5.321612844166258682, 0.9647713018063041046 ) ) ;
#21929 = ORIENTED_EDGE ( 'NONE', *, *, #1489, .F. ) ;
#21930 = CARTESIAN_POINT ( 'NONE',  ( 47.10000000000002274, -3.726179070414207928, -1.000000000000000000 ) ) ;
#21931 = CARTESIAN_POINT ( 'NONE',  ( -57.19702994616204705, 4.156921938165313080, -1.880369327726949834E-13 ) ) ;
#21932 = ORIENTED_EDGE ( 'NONE', *, *, #17336, .F. ) ;
#21933 = CARTESIAN_POINT ( 'NONE',  ( 69.20000000000001705, -0.7500000000000000000, -1.988246715074081017 ) ) ;
#21934 = AXIS2_PLACEMENT_3D ( 'NONE', #24690, #12795, #8217 ) ;
#21935 = CARTESIAN_POINT ( 'NONE',  ( 51.80000000000001847, 1.734723475976807094E-15, -4.275000000000000355 ) ) ;
#21936 = CARTESIAN_POINT ( 'NONE',  ( 32.54904120526451550, 8.004085848662246150, 2.049999999999885691 ) ) ;
#21937 = ORIENTED_EDGE ( 'NONE', *, *, #4031, .T. ) ;
#21938 = EDGE_CURVE ( 'NONE', #5594, #21736, #11340, .T. ) ;
#21939 = CARTESIAN_POINT ( 'NONE',  ( -54.93749999999998579, 1.962990915244722689, 3.399999999999812506 ) ) ;
#21940 = CARTESIAN_POINT ( 'NONE',  ( 53.05468381831882851, 8.377149132718326285, -2.050000000000184563 ) ) ;
#21941 = CARTESIAN_POINT ( 'NONE',  ( 58.73379417893105625, -1.006340787081331456, -1.582215608938851270 ) ) ;
#21942 = DIRECTION ( 'NONE',  ( 1.000000000000000000, 1.047444401652940007E-14, 0.000000000000000000 ) ) ;
#21943 = CARTESIAN_POINT ( 'NONE',  ( 57.03405126743467690, -0.7473881623357462312, 2.422979693216943176 ) ) ;
#21944 =( BOUNDED_SURFACE ( )  B_SPLINE_SURFACE ( 3, 2, ( 
 ( #14852, #19788, #7732 ),
 ( #23910, #26436, #29121 ),
 ( #28965, #7593, #21549 ),
 ( #17394, #5058, #4729 ),
 ( #14239, #27041, #14390 ),
 ( #2684, #16942, #9970 ),
 ( #12040, #19328, #2538 ),
 ( #19642, #24513, #2827 ),
 ( #9521, #24062, #21714 ),
 ( #19180, #3, #7273 ),
 ( #26587, #12185, #5834 ),
 ( #29898, #17726, #22322 ),
 ( #2994, #12637, #22797 ),
 ( #10589, #17565, #27214 ),
 ( #15494, #22938, #8521 ),
 ( #30040, #8059, #3301 ) ),
 .UNSPECIFIED., .F., .F., .F. ) 
 B_SPLINE_SURFACE_WITH_KNOTS ( ( 4, 2, 2, 2, 2, 2, 2, 4 ),
 ( 3, 3 ),
 ( 0.001780502285214207499, 0.002558945925323793252, 0.002753556835351190016, 0.002948167745378586346, 0.003337389565433379439, 0.003726611385488172532, 0.004115833205542965625, 0.004894276845652550945 ),
 ( 0.000000000000000000, 1.000000000000000000 ),
 .UNSPECIFIED. ) 
 GEOMETRIC_REPRESENTATION_ITEM ( )  RATIONAL_B_SPLINE_SURFACE ( (
 ( 1.000000000000000000, 0.9418517008537220514, 1.000000000000000000),
 ( 1.000000000000000000, 0.9417987965885382673, 1.000000000000000000),
 ( 1.000000000000000000, 0.9418198861733636518, 1.000000000000000000),
 ( 1.000000000000000000, 0.9434060303845666073, 1.000000000000000000),
 ( 1.000000000000000000, 0.9437939819948258924, 1.000000000000000000),
 ( 1.000000000000000000, 0.9445989566712681418, 1.000000000000000000),
 ( 1.000000000000000000, 0.9450169930049783229, 1.000000000000000000),
 ( 1.000000000000000000, 0.9461610507673675619, 1.000000000000000000),
 ( 1.000000000000000000, 0.9467217966427196041, 1.000000000000000000),
 ( 1.000000000000000000, 0.9467345476124345849, 1.000000000000000000),
 ( 1.000000000000000000, 0.9461964028052562981, 1.000000000000000000),
 ( 1.000000000000000000, 0.9446801822474193422, 1.000000000000000000),
 ( 1.000000000000000000, 0.9437582546536890105, 1.000000000000000000),
 ( 1.000000000000000000, 0.9418129560294938862, 1.000000000000000000),
 ( 1.000000000000000000, 0.9418016889778016987, 1.000000000000000000),
 ( 1.000000000000000000, 0.9418517008537222734, 1.000000000000000000) ) ) 
 REPRESENTATION_ITEM ( '' )  SURFACE ( )  );
#21946 = FACE_OUTER_BOUND ( 'NONE', #1841, .T. ) ;
#21945 = CARTESIAN_POINT ( 'NONE',  ( -36.43290890416756156, -3.561547362098786973, 4.076645242318810425 ) ) ;
#21947 = DIRECTION ( 'NONE',  ( 1.000000000000000000, 3.054025858079668409E-16, -2.042474015755241579E-16 ) ) ;
#21948 = DIRECTION ( 'NONE',  ( 1.000000000000000000, 3.053848253006669023E-16, -2.042510438544995415E-16 ) ) ;
#21949 = EDGE_CURVE ( 'NONE', #29844, #29879, #29050, .T. ) ;
#21950 = CARTESIAN_POINT ( 'NONE',  ( 61.24959995150304337, -0.9774770340128312585, -1.663387054287091882 ) ) ;
#21951 = ORIENTED_EDGE ( 'NONE', *, *, #7870, .F. ) ;
#21952 = ORIENTED_EDGE ( 'NONE', *, *, #14724, .F. ) ;
#21953 = CARTESIAN_POINT ( 'NONE',  ( 58.45000000000001705, 0.000000000000000000, 0.000000000000000000 ) ) ;
#21954 = CARTESIAN_POINT ( 'NONE',  ( -54.29792740578361077, 3.330682475591790315, 0.6830477631804100502 ) ) ;
#21956 = CARTESIAN_POINT ( 'NONE',  ( 51.80000000000001847, 2.428612866367529932E-14, 0.000000000000000000 ) ) ;
#21955 = CARTESIAN_POINT ( 'NONE',  ( -74.39999999999997726, -2.588216748940040213E-15, 4.710014593512140639E-15 ) ) ;
#21957 = EDGE_LOOP ( 'NONE', ( #1867, #19090 ) ) ;
#21958 = ORIENTED_EDGE ( 'NONE', *, *, #7486, .F. ) ;
#21959 = LINE ( 'NONE', #246, #27540 ) ;
#21960 = VERTEX_POINT ( 'NONE', #28329 ) ;
#21961 = CARTESIAN_POINT ( 'NONE',  ( 51.25000000000001421, 0.7500000000005367928, -1.718465885608440269 ) ) ;
#21962 = ORIENTED_EDGE ( 'NONE', *, *, #5984, .T. ) ;
#21963 = CARTESIAN_POINT ( 'NONE',  ( 33.39233489564305302, 8.222108905995247241, -2.050000000000115730 ) ) ;
#21964 = VERTEX_POINT ( 'NONE', #30859 ) ;
#21965 = CARTESIAN_POINT ( 'NONE',  ( -54.49999999999997868, 0.000000000000000000, -0.7500000000000001110 ) ) ;
#21966 = LINE ( 'NONE', #14810, #29932 ) ;
#21967 = EDGE_CURVE ( 'NONE', #5072, #22540, #6786, .T. ) ;
#21968 = LINE ( 'NONE', #9152, #6661 ) ;
#21970 = CARTESIAN_POINT ( 'NONE',  ( -55.70655989232410832, 1.962990915244748891, -3.400000000000189093 ) ) ;
#21969 = AXIS2_PLACEMENT_3D ( 'NONE', #12171, #7114, #17093 ) ;
#21971 = CARTESIAN_POINT ( 'NONE',  ( 53.94440344817342492, 6.524635634306411802, -1.761196874214848052 ) ) ;
#21972 = DIRECTION ( 'NONE',  ( 1.037591611799212092E-14, 0.000000000000000000, 1.000000000000000000 ) ) ;
#21973 = CARTESIAN_POINT ( 'NONE',  ( -36.11122220296834939, -3.378548217643453366, -3.972894518062632052 ) ) ;
#21974 = CIRCLE ( 'NONE', #16349, 4.375000000000000000 ) ;
#21975 = CARTESIAN_POINT ( 'NONE',  ( -54.49999999999997868, 0.000000000000000000, 4.349999999999997868 ) ) ;
#21976 = VERTEX_POINT ( 'NONE', #30378 ) ;
#21977 = CARTESIAN_POINT ( 'NONE',  ( 57.02185466405004632, -0.7499999999999981126, -2.421260014775926006 ) ) ;
#21978 = DIRECTION ( 'NONE',  ( 1.000000000000000000, 0.000000000000000000, -3.491481338843133355E-15 ) ) ;
#21979 = CARTESIAN_POINT ( 'NONE',  ( 47.10000000000002274, 2.428612866367529932E-14, -1.100000000000000089 ) ) ;
#21980 = AXIS2_PLACEMENT_3D ( 'NONE', #5051, #21707, #8091 ) ;
#21981 = EDGE_LOOP ( 'NONE', ( #13760, #5933, #30088, #18374 ) ) ;
#21982 = CARTESIAN_POINT ( 'NONE',  ( -59.67455719258389735, -3.195666608421381838, -1.223849197751685436 ) ) ;
#21983 = VERTEX_POINT ( 'NONE', #16139 ) ;
#21984 = CARTESIAN_POINT ( 'NONE',  ( 15.48609859788818355, 0.1138661108243574638, -5.199999999057642874 ) ) ;
#21985 = CIRCLE ( 'NONE', #16416, 2.750000000000000000 ) ;
#21986 = CARTESIAN_POINT ( 'NONE',  ( -36.58413561666647951, -5.174628573245042773, 1.572974725650844174 ) ) ;
#21988 = CARTESIAN_POINT ( 'NONE',  ( -59.19999999999997442, 3.400000000000007905, -1.910919895035100347E-13 ) ) ;
#21987 = CARTESIAN_POINT ( 'NONE',  ( 48.46289871413547701, -1.426739617975173013, -3.843750000000023981 ) ) ;
#21989 = ADVANCED_FACE ( 'NONE', ( #18679, #30229, #23744, #8830, #23273, #20597 ), #3943, .T. ) ;
#21990 = EDGE_LOOP ( 'NONE', ( #15152, #17491, #9127, #9829 ) ) ;
#21991 = CYLINDRICAL_SURFACE ( 'NONE', #12842, 0.05000000000000012768 ) ;
#21992 = CARTESIAN_POINT ( 'NONE',  ( -45.15971931043468146, 0.000000000000000000, 0.000000000000000000 ) ) ;
#21994 = CARTESIAN_POINT ( 'NONE',  ( -59.69999999999997442, 2.455304892039244180, -1.238538609462265905 ) ) ;
#21993 = CARTESIAN_POINT ( 'NONE',  ( 34.56269065792915995, 8.313757757582562746, -1.950000000000119860 ) ) ;
#21995 = ORIENTED_EDGE ( 'NONE', *, *, #23186, .F. ) ;
#21996 = CARTESIAN_POINT ( 'NONE',  ( -60.93749999999995737, -4.108500314926507357, 1.367561758111407455 ) ) ;
#21997 = CARTESIAN_POINT ( 'NONE',  ( 61.24794577449333133, 0.9523642485468641894, 1.677218681935483069 ) ) ;
#21998 = DIRECTION ( 'NONE',  ( 1.000000000000000000, 3.054025858079668409E-16, -2.042474015755241579E-16 ) ) ;
#21999 = CARTESIAN_POINT ( 'NONE',  ( -55.43749999999997868, -3.399999999999991473, -2.094585006122325661E-13 ) ) ;
#22000 = ADVANCED_FACE ( 'NONE', ( #11218 ), #5789, .T. ) ;
#22001 = CARTESIAN_POINT ( 'NONE',  ( -55.02900635094608361, -1.737685414808514794, 3.471684241605561994 ) ) ;
#22002 = LINE ( 'NONE', #14382, #2058 ) ;
#22003 = CARTESIAN_POINT ( 'NONE',  ( -35.85663232820584057, -1.793057972834811054, 4.026191436120395650 ) ) ;
#22004 = ADVANCED_FACE ( 'NONE', ( #15964 ), #6635, .F. ) ;
#22005 = AXIS2_PLACEMENT_3D ( 'NONE', #26013, #18604, #27778 ) ;
#22006 = ORIENTED_EDGE ( 'NONE', *, *, #19754, .T. ) ;
#22007 = DIRECTION ( 'NONE',  ( 3.016910393003118404E-15, 0.000000000000000000, 1.000000000000000000 ) ) ;
#22008 = AXIS2_PLACEMENT_3D ( 'NONE', #10500, #8119, #17787 ) ;
#22009 = CARTESIAN_POINT ( 'NONE',  ( 22.08866779209807873, 7.467293579578107909, -1.950000000000077005 ) ) ;
#22010 = CARTESIAN_POINT ( 'NONE',  ( -59.09999999999997300, 8.366749974758448157E-15, -2.099585467500611340E-13 ) ) ;
#22011 = B_SPLINE_CURVE_WITH_KNOTS ( 'NONE', 3,
 ( #30169, #3721, #13537, #8487 ),
 .UNSPECIFIED., .F., .F.,
 ( 4, 4 ),
 ( 8.741117365843378158E-19, 2.862003379457917908E-05 ),
 .UNSPECIFIED. ) ;
#22012 = ADVANCED_FACE ( 'NONE', ( #25790 ), #13890, .F. ) ;
#22013 = TOROIDAL_SURFACE ( 'NONE', #18969, 2.750000000000000000, 0.05000000000000000278 ) ;
#22014 = DIRECTION ( 'NONE',  ( 1.000000000000000000, 3.054025858079668409E-16, -2.042474015755241579E-16 ) ) ;
#22015 = LINE ( 'NONE', #10275, #20047 ) ;
#22017 = CARTESIAN_POINT ( 'NONE',  ( 23.49584529083620765, 5.910990189302488318, 1.424999999999918554 ) ) ;
#22016 = CARTESIAN_POINT ( 'NONE',  ( 51.12687253673779253, 0.9194130538826106314, 1.491219977510798156 ) ) ;
#22018 = ORIENTED_EDGE ( 'NONE', *, *, #26519, .T. ) ;
#22019 = CARTESIAN_POINT ( 'NONE',  ( 51.80000000000001847, 2.428612866367529932E-14, -1.808587333520743709E-13 ) ) ;
#22020 = ORIENTED_EDGE ( 'NONE', *, *, #11056, .T. ) ;
#22021 = CARTESIAN_POINT ( 'NONE',  ( 51.80000000000001137, 4.287867059355201071, -1.832567882403405068 ) ) ;
#22023 = CARTESIAN_POINT ( 'NONE',  ( 58.66054497608038076, -0.4999999999994944599, -1.807104036850091688 ) ) ;
#22022 = CARTESIAN_POINT ( 'NONE',  ( 57.02405634237670284, 0.7430569499193692140, -2.425812863566016997 ) ) ;
#22024 = CARTESIAN_POINT ( 'NONE',  ( -54.49999999999999289, 1.433333333333330906, 4.054078878802625852 ) ) ;
#22025 = ADVANCED_FACE ( 'NONE', ( #18520 ), #29265, .T. ) ;
#22026 = ORIENTED_EDGE ( 'NONE', *, *, #5182, .F. ) ;
#22027 = AXIS2_PLACEMENT_3D ( 'NONE', #6045, #27551, #5570 ) ;
#22028 = EDGE_LOOP ( 'NONE', ( #4919, #22453, #27191, #9627 ) ) ;
#22029 = LINE ( 'NONE', #16815, #14366 ) ;
#22030 = FACE_OUTER_BOUND ( 'NONE', #13086, .T. ) ;
#22031 = EDGE_LOOP ( 'NONE', ( #38, #14149, #10871, #15200 ) ) ;
#22032 = EDGE_CURVE ( 'NONE', #23034, #20928, #6287, .T. ) ;
#22033 = CARTESIAN_POINT ( 'NONE',  ( 50.30000000000001847, -1.426739617975173013, 3.843750000000023093 ) ) ;
#22034 = CARTESIAN_POINT ( 'NONE',  ( -55.04792740578361077, 3.330682475591790315, 0.6830477631804101613 ) ) ;
#22035 = CARTESIAN_POINT ( 'NONE',  ( -36.92362342067168868, -5.192953935288583622, -1.516181439821844279 ) ) ;
#22036 = ORIENTED_EDGE ( 'NONE', *, *, #12527, .T. ) ;
#22037 = AXIS2_PLACEMENT_3D ( 'NONE', #11646, #9272, #30798 ) ;
#22038 = CARTESIAN_POINT ( 'NONE',  ( -61.34999999999997300, -2.609922480197373940, 0.4591346723570145505 ) ) ;
#22039 = ADVANCED_FACE ( 'NONE', ( #6959 ), #9840, .T. ) ;
#22040 = EDGE_CURVE ( 'NONE', #22071, #17711, #7576, .T. ) ;
#22041 = ORIENTED_EDGE ( 'NONE', *, *, #23398, .T. ) ;
#22042 = CARTESIAN_POINT ( 'NONE',  ( -57.25952994616203995, 3.117691453623994580, -1.800000000000189671 ) ) ;
#22043 = CARTESIAN_POINT ( 'NONE',  ( 50.31874172786520916, 1.426739617975217866, 3.843750000000022649 ) ) ;
#22044 = FACE_BOUND ( 'NONE', #18172, .T. ) ;
#22045 = DIRECTION ( 'NONE',  ( 1.000000000000000000, 0.000000000000000000, 0.000000000000000000 ) ) ;
#22046 = AXIS2_PLACEMENT_3D ( 'NONE', #15479, #10258, #14840 ) ;
#22047 = VECTOR ( 'NONE', #1544, 1000.000000000000114 ) ;
#22048 = CARTESIAN_POINT ( 'NONE',  ( 51.70000000000000995, -4.179189514726507682, -1.000000000000000000 ) ) ;
#22049 = AXIS2_PLACEMENT_3D ( 'NONE', #15060, #16983, #19217 ) ;
#22050 = DIRECTION ( 'NONE',  ( 0.000000000000000000, 0.000000000000000000, 1.000000000000000000 ) ) ;
#22052 = CARTESIAN_POINT ( 'NONE',  ( -36.30424252565905618, 0.1108756495952690768, -5.200000001675009642 ) ) ;
#22051 = FACE_OUTER_BOUND ( 'NONE', #23354, .T. ) ;
#22053 = AXIS2_PLACEMENT_3D ( 'NONE', #22599, #5971, #15626 ) ;
#22054 = CARTESIAN_POINT ( 'NONE',  ( 51.14630318392394770, 0.9364487020639118420, -1.503522130792751987 ) ) ;
#22055 = LINE ( 'NONE', #809, #8406 ) ;
#22056 = TOROIDAL_SURFACE ( 'NONE', #28623, 0.2000000000000000111, 0.1000000000000000056 ) ;
#22058 = CARTESIAN_POINT ( 'NONE',  ( 57.02184386277451722, -0.7500000000000000000, 2.421260326253384942 ) ) ;
#22057 = CARTESIAN_POINT ( 'NONE',  ( 15.76623786017541562, 5.175840503946205651, -1.569056257078622618 ) ) ;
#22059 = EDGE_LOOP ( 'NONE', ( #3539, #22743 ) ) ;
#22060 = DIRECTION ( 'NONE',  ( -1.000000000000000000, 0.000000000000000000, 1.047444401652940007E-14 ) ) ;
#22061 = CIRCLE ( 'NONE', #30120, 0.1000000000000001305 ) ;
#22062 = CARTESIAN_POINT ( 'NONE',  ( -36.92405921417685022, -5.187083072802368022, -1.534568794951191251 ) ) ;
#22064 = DIRECTION ( 'NONE',  ( -3.489354422748178188E-15, 1.218509414717996091E-16, -1.000000000000000000 ) ) ;
#22063 = DIRECTION ( 'NONE',  ( 1.000000000000000000, 1.047444401652940007E-14, 0.000000000000000000 ) ) ;
#22065 = FACE_OUTER_BOUND ( 'NONE', #23150, .T. ) ;
#22066 = EDGE_CURVE ( 'NONE', #19552, #28113, #21528, .T. ) ;
#22067 = ORIENTED_EDGE ( 'NONE', *, *, #26088, .T. ) ;
#22068 = DIRECTION ( 'NONE',  ( 2.581436205204234499E-16, -0.9796124928211140670, -0.2008964009354146651 ) ) ;
#22069 = EDGE_CURVE ( 'NONE', #12204, #8913, #26513, .T. ) ;
#22070 = AXIS2_PLACEMENT_3D ( 'NONE', #25512, #17788, #29959 ) ;
#22071 = VERTEX_POINT ( 'NONE', #16774 ) ;
#22072 = EDGE_CURVE ( 'NONE', #22168, #31257, #5259, .T. ) ;
#22073 = CARTESIAN_POINT ( 'NONE',  ( 51.14630318392394770, 0.9364487020639118420, -1.503522130792751987 ) ) ;
#22074 = ORIENTED_EDGE ( 'NONE', *, *, #5579, .F. ) ;
#22075 = ORIENTED_EDGE ( 'NONE', *, *, #10025, .F. ) ;
#22076 = VECTOR ( 'NONE', #27092, 1000.000000000000000 ) ;
#22077 = CARTESIAN_POINT ( 'NONE',  ( 15.03925126672132784, 5.377732432866644707, -0.5657657256215208319 ) ) ;
#22078 = ORIENTED_EDGE ( 'NONE', *, *, #5718, .T. ) ;
#22079 = CARTESIAN_POINT ( 'NONE',  ( 51.87915152462694124, 4.432914534380794080, 1.230195908850218123 ) ) ;
#22080 = CARTESIAN_POINT ( 'NONE',  ( -56.57202994616203995, 2.078460969082674747, -3.600000000000191935 ) ) ;
#22081 = ORIENTED_EDGE ( 'NONE', *, *, #24035, .F. ) ;
#22082 = AXIS2_PLACEMENT_3D ( 'NONE', #18749, #16688, #26175 ) ;
#22083 = DIRECTION ( 'NONE',  ( -1.000000000000000000, -3.053848253006669023E-16, 2.042510438544995415E-16 ) ) ;
#22084 = CARTESIAN_POINT ( 'NONE',  ( -44.59999999999998010, -2.749999999999991562, -1.689336410186543392E-13 ) ) ;
#22085 = AXIS2_PLACEMENT_3D ( 'NONE', #23519, #16395, #14006 ) ;
#22086 = CARTESIAN_POINT ( 'NONE',  ( 33.40812713681398805, 8.122903765862725223, 2.049999999999884803 ) ) ;
#22087 = ORIENTED_EDGE ( 'NONE', *, *, #11830, .T. ) ;
#22088 = VECTOR ( 'NONE', #17840, 1000.000000000000000 ) ;
#22089 = FACE_BOUND ( 'NONE', #22652, .T. ) ;
#22090 = AXIS2_PLACEMENT_3D ( 'NONE', #11168, #1191, #13364 ) ;
#22091 =( BOUNDED_CURVE ( )  B_SPLINE_CURVE ( 2, ( #17246, #10112, #12778, #7723, #12312, #10415, #22459, #17717, #29733 ),
 .UNSPECIFIED., .F., .T. ) 
 B_SPLINE_CURVE_WITH_KNOTS ( ( 3, 2, 2, 2, 3 ),
 ( 0.1944444444444444475, 0.2037037037037036924, 0.2222222222222222099, 0.2407407407407407274, 0.2500000000000000000 ),
 .UNSPECIFIED. ) 
 CURVE ( )  GEOMETRIC_REPRESENTATION_ITEM ( )  RATIONAL_B_SPLINE_CURVE ( ( 0.9330127018922192983, 0.9330127018922194093, 1.000000000000000000, 0.8660254037844387076, 1.000000000000000000, 0.8660254037844387076, 1.000000000000000000, 0.9330127018922191873, 0.9330127018922192983 ) ) 
 REPRESENTATION_ITEM ( '' )  );
#22092 = DIRECTION ( 'NONE',  ( 0.5633368246415009217, 0.8262273428075537218, 0.000000000000000000 ) ) ;
#22093 = DIRECTION ( 'NONE',  ( 0.000000000000000000, 0.000000000000000000, 1.000000000000000000 ) ) ;
#22094 = DIRECTION ( 'NONE',  ( 1.000000000000000000, 2.586136946169074517E-16, -0.000000000000000000 ) ) ;
#22095 = CARTESIAN_POINT ( 'NONE',  ( 57.00000000000001421, 0.7058179832143345322, 2.448718171069995009 ) ) ;
#22096 = AXIS2_PLACEMENT_3D ( 'NONE', #18888, #30912, #21125 ) ;
#22098 = CARTESIAN_POINT ( 'NONE',  ( 51.80000000000001847, -3.726179070414207928, 1.000000000000002220 ) ) ;
#22097 = DIRECTION ( 'NONE',  ( 0.000000000000000000, -0.3529411764705897014, -0.9356455129756974243 ) ) ;
#22099 = VECTOR ( 'NONE', #25659, 1000.000000000000000 ) ;
#22100 = VECTOR ( 'NONE', #360, 1000.000000000000000 ) ;
#22101 = CARTESIAN_POINT ( 'NONE',  ( 51.08379317338046377, 0.8723108729837811826, 1.374656996893403260 ) ) ;
#22102 = CARTESIAN_POINT ( 'NONE',  ( 60.75000000000002842, -0.4999999999993638977, -1.863080903343643069 ) ) ;
#22104 = CARTESIAN_POINT ( 'NONE',  ( 61.25000000000003553, -0.9999999999993586242, -1.655766640118113031 ) ) ;
#22103 = CONICAL_SURFACE ( 'NONE', #20589, 2.250000000000000444, 0.7853981633974536081 ) ;
#22105 = EDGE_LOOP ( 'NONE', ( #21017, #15828 ) ) ;
#22106 = CIRCLE ( 'NONE', #12470, 4.375000000000000000 ) ;
#22107 = TOROIDAL_SURFACE ( 'NONE', #20100, 4.500000000000037303, 0.1000000000000000056 ) ;
#22108 = ADVANCED_FACE ( 'NONE', ( #4879 ), #21991, .T. ) ;
#22109 = ORIENTED_EDGE ( 'NONE', *, *, #28141, .F. ) ;
#22110 = ORIENTED_EDGE ( 'NONE', *, *, #25338, .T. ) ;
#22111 = CIRCLE ( 'NONE', #7916, 1.975000000000001865 ) ;
#22112 = AXIS2_PLACEMENT_3D ( 'NONE', #11018, #6421, #16083 ) ;
#22113 = DIRECTION ( 'NONE',  ( 1.000000000000000000, 3.054025858079668409E-16, -2.042474015755241579E-16 ) ) ;
#22114 = CARTESIAN_POINT ( 'NONE',  ( -57.61042740578359656, -2.936324665650201116, -2.606018187048497747 ) ) ;
#22115 = CARTESIAN_POINT ( 'NONE',  ( 69.20000000000005969, -0.8382352941176473005, 2.222158093316557004 ) ) ;
#22116 = ORIENTED_EDGE ( 'NONE', *, *, #20469, .T. ) ;
#22117 = ORIENTED_EDGE ( 'NONE', *, *, #2364, .F. ) ;
#22118 = DIRECTION ( 'NONE',  ( 1.000000000000000000, 3.053848253006669023E-16, -2.042510438544995415E-16 ) ) ;
#22119 = ORIENTED_EDGE ( 'NONE', *, *, #29522, .F. ) ;
#22120 = CARTESIAN_POINT ( 'NONE',  ( 51.80000000000001847, 2.428612866367529932E-14, -1.808587333520743709E-13 ) ) ;
#22121 = ORIENTED_EDGE ( 'NONE', *, *, #4707, .T. ) ;
#22122 = CARTESIAN_POINT ( 'NONE',  ( 34.56702326949724835, 8.213851659285211326, -1.950000000000119860 ) ) ;
#22123 = EDGE_LOOP ( 'NONE', ( #7458, #6975 ) ) ;
#22124 = CIRCLE ( 'NONE', #16557, 0.4600000000000000755 ) ;
#22125 = DIRECTION ( 'NONE',  ( 0.000000000000000000, -1.000000000000000000, 0.000000000000000000 ) ) ;
#22126 = AXIS2_PLACEMENT_3D ( 'NONE', #10403, #20245, #29262 ) ;
#22127 = EDGE_CURVE ( 'NONE', #20935, #11715, #2737, .T. ) ;
#22128 = CIRCLE ( 'NONE', #20612, 0.05000000000000012768 ) ;
#22129 = CARTESIAN_POINT ( 'NONE',  ( -54.58155989232414385, -1.962990915244731571, 3.399999999999797851 ) ) ;
#22130 = CARTESIAN_POINT ( 'NONE',  ( 54.17887612135720588, 6.867997567695679706, -2.050000000000189004 ) ) ;
#22131 = CIRCLE ( 'NONE', #23642, 0.4500000000000001221 ) ;
#22132 = AXIS2_PLACEMENT_3D ( 'NONE', #14602, #24267, #25015 ) ;
#22134 = AXIS2_PLACEMENT_3D ( 'NONE', #12469, #17553, #12936 ) ;
#22133 = DIRECTION ( 'NONE',  ( 0.03489949670250097613, 0.9993908270190957621, 0.000000000000000000 ) ) ;
#22135 = CARTESIAN_POINT ( 'NONE',  ( 15.59140265158956140, -4.755985070912263524, -2.573747172434730945 ) ) ;
#22136 = B_SPLINE_CURVE_WITH_KNOTS ( 'NONE', 3,
 ( #24574, #12843, #20169, #3365, #5735, #26809, #22525, #29800, #27107, #17783, #12382, #29335, #27424, #5428, #2897, #3052 ),
 .UNSPECIFIED., .F., .F.,
 ( 4, 2, 2, 2, 2, 2, 2, 4 ),
 ( 1.734723475976807094E-18, 0.0004351083927046432947, 0.0008702167854092848548, 0.001740433570818574914, 0.002175541963523219997, 0.002610650356227864864, 0.003045758748932510165, 0.003480867141637155032 ),
 .UNSPECIFIED. ) ;
#22137 = CARTESIAN_POINT ( 'NONE',  ( 64.25000000000001421, 1.163569835200988601E-28, 1.624999999999777067 ) ) ;
#22138 = ORIENTED_EDGE ( 'NONE', *, *, #25086, .F. ) ;
#22139 = AXIS2_PLACEMENT_3D ( 'NONE', #446, #7582, #10109 ) ;
#22140 = DIRECTION ( 'NONE',  ( 0.000000000000000000, 0.000000000000000000, 1.000000000000000000 ) ) ;
#22141 = AXIS2_PLACEMENT_3D ( 'NONE', #18996, #18841, #14066 ) ;
#22142 = DIRECTION ( 'NONE',  ( -3.491481338843133355E-15, 0.000000000000000000, -1.000000000000000000 ) ) ;
#22143 = DIRECTION ( 'NONE',  ( 0.9957419851084058360, 0.09218405009746234724, -4.336808689941986970E-15 ) ) ;
#22144 = ORIENTED_EDGE ( 'NONE', *, *, #20656, .F. ) ;
#22145 = EDGE_CURVE ( 'NONE', #24125, #13972, #26566, .T. ) ;
#22146 = CARTESIAN_POINT ( 'NONE',  ( 50.50000000000002132, 0.6462379109121000331, -4.048750000000023164 ) ) ;
#22147 = VECTOR ( 'NONE', #7395, 1000.000000000000000 ) ;
#22148 = ORIENTED_EDGE ( 'NONE', *, *, #24908, .F. ) ;
#22149 = CARTESIAN_POINT ( 'NONE',  ( -59.69999999999997442, 8.366749974758454467E-15, -2.120534355533670266E-13 ) ) ;
#22150 = CARTESIAN_POINT ( 'NONE',  ( -35.85663232820581214, -4.804073783693462829, 2.042134687550346772 ) ) ;
#22152 = DIRECTION ( 'NONE',  ( 1.000000000000000000, 0.000000000000000000, 0.000000000000000000 ) ) ;
#22151 = CARTESIAN_POINT ( 'NONE',  ( 50.92088486138060688, -4.387164041431067751, 1.383037119376580470 ) ) ;
#22153 = VERTEX_POINT ( 'NONE', #19458 ) ;
#22154 = CARTESIAN_POINT ( 'NONE',  ( 60.97799375661013244, -0.7610968749141068246, -1.436497712332848398 ) ) ;
#22155 = CIRCLE ( 'NONE', #14034, 2.874999999999999112 ) ;
#22156 = DIRECTION ( 'NONE',  ( 1.000000000000000000, 2.586136946169074517E-16, -0.000000000000000000 ) ) ;
#22158 = DIRECTION ( 'NONE',  ( -3.491481338843133355E-15, -3.491481338843133355E-15, 1.000000000000000000 ) ) ;
#22157 = CARTESIAN_POINT ( 'NONE',  ( 52.44060252733988392, 4.003370659767288231, 2.045783712298512746 ) ) ;
#22159 = DIRECTION ( 'NONE',  ( 0.000000000000000000, 0.000000000000000000, 1.000000000000000000 ) ) ;
#22160 = CARTESIAN_POINT ( 'NONE',  ( -60.56249999999997158, 4.108500314926511798, -1.367561758111406345 ) ) ;
#22161 = CARTESIAN_POINT ( 'NONE',  ( 58.65000000000001990, 6.143261415694495821E-13, 3.111507638930570854E-58 ) ) ;
#22162 = CARTESIAN_POINT ( 'NONE',  ( -55.18749999999997158, 3.238593381231846369, 2.874284765127020691 ) ) ;
#22163 = ADVANCED_FACE ( 'NONE', ( #24497 ), #9326, .T. ) ;
#22164 = CARTESIAN_POINT ( 'NONE',  ( 58.75000000000000711, 1.800471618824440734, 1.039502773797588597 ) ) ;
#22165 = DIRECTION ( 'NONE',  ( 0.000000000000000000, 0.000000000000000000, -1.000000000000000000 ) ) ;
#22166 = DIRECTION ( 'NONE',  ( -0.9993908270190956511, 0.03489949670250089980, 3.491481338843132961E-15 ) ) ;
#22167 = CARTESIAN_POINT ( 'NONE',  ( 51.98914612709255323, -0.7788013043298537275, -1.433123603079401231 ) ) ;
#22168 = VERTEX_POINT ( 'NONE', #26265 ) ;
#22169 = AXIS2_PLACEMENT_3D ( 'NONE', #11982, #28606, #17061 ) ;
#22170 = VECTOR ( 'NONE', #28359, 1000.000000000000114 ) ;
#22171 = DIRECTION ( 'NONE',  ( -1.000000000000000000, -0.000000000000000000, 3.491481338843133355E-15 ) ) ;
#22172 = DIRECTION ( 'NONE',  ( 0.000000000000000000, 0.000000000000000000, -1.000000000000000000 ) ) ;
#22173 = CARTESIAN_POINT ( 'NONE',  ( 15.03925126672132961, 1.123735532908280765, -5.289358697221546279 ) ) ;
#22174 = CARTESIAN_POINT ( 'NONE',  ( 51.14630318392396902, -0.9364487020628400327, 1.503522130792752209 ) ) ;
#22175 = CARTESIAN_POINT ( 'NONE',  ( -56.59599364905386665, 0.2309624077929022246, 3.875409454552789956 ) ) ;
#22177 = CARTESIAN_POINT ( 'NONE',  ( 27.10659297677966961, 5.279073180725294634, 1.424999999999906564 ) ) ;
#22176 = DIRECTION ( 'NONE',  ( 0.000000000000000000, 0.000000000000000000, 1.000000000000000000 ) ) ;
#22178 = VERTEX_POINT ( 'NONE', #31167 ) ;
#22179 = EDGE_CURVE ( 'NONE', #26840, #31166, #30411, .T. ) ;
#22180 = CARTESIAN_POINT ( 'NONE',  ( 61.25000000000004263, -1.499837071477534867, 1.323060376180833275 ) ) ;
#22181 = VERTEX_POINT ( 'NONE', #14836 ) ;
#22182 = UNCERTAINTY_MEASURE_WITH_UNIT (LENGTH_MEASURE( 1.000000000000000082E-05 ), #19816, 'distance_accuracy_value', 'NONE');
#22183 = DIRECTION ( 'NONE',  ( 1.000000000000000000, 0.000000000000000000, 0.000000000000000000 ) ) ;
#22185 = DIRECTION ( 'NONE',  ( 0.000000000000000000, 0.3333333333333307058, 0.9428090415820643555 ) ) ;
#22184 = CARTESIAN_POINT ( 'NONE',  ( 15.17256654081423051, -3.426725948577732606, -3.937891352654259602 ) ) ;
#22187 = EDGE_CURVE ( 'NONE', #4123, #23938, #26999, .T. ) ;
#22186 = DIRECTION ( 'NONE',  ( 0.000000000000000000, 0.000000000000000000, 1.000000000000000000 ) ) ;
#22188 = ORIENTED_EDGE ( 'NONE', *, *, #6628, .T. ) ;
#22189 = AXIS2_PLACEMENT_3D ( 'NONE', #22332, #27054, #7145 ) ;
#22190 = ORIENTED_EDGE ( 'NONE', *, *, #19685, .T. ) ;
#22191 = DIRECTION ( 'NONE',  ( 1.000000000000000000, 1.047444401652940007E-14, 0.000000000000000000 ) ) ;
#22192 = STYLED_ITEM ( 'NONE', ( #4464 ), #27821 ) ;
#22193 = CARTESIAN_POINT ( 'NONE',  ( 47.12400663174540938, -3.859587729118648447, 1.644141655454772977 ) ) ;
#22194 = ORIENTED_EDGE ( 'NONE', *, *, #1099, .F. ) ;
#22195 = CARTESIAN_POINT ( 'NONE',  ( 56.95000000000001705, -0.6820512820512817376, -1.773360101234997988 ) ) ;
#22196 = CARTESIAN_POINT ( 'NONE',  ( 50.34665981758797670, 1.329038565861465848, 3.861394075523872260 ) ) ;
#22197 = CARTESIAN_POINT ( 'NONE',  ( -36.89017861347080185, -5.235729994560249345, -1.359191621353769142 ) ) ;
#22198 = ORIENTED_EDGE ( 'NONE', *, *, #7021, .T. ) ;
#22199 = DIRECTION ( 'NONE',  ( 0.000000000000000000, 0.000000000000000000, 1.000000000000000000 ) ) ;
#22200 = ADVANCED_FACE ( 'NONE', ( #9791 ), #21380, .T. ) ;
#22201 = CARTESIAN_POINT ( 'NONE',  ( 58.74154451056421067, -1.258335925859845439, -1.390058629628315057 ) ) ;
#22202 = ORIENTED_EDGE ( 'NONE', *, *, #7933, .T. ) ;
#22203 = CARTESIAN_POINT ( 'NONE',  ( -57.63452994616205416, -3.117691453623976816, 1.799999999999783329 ) ) ;
#22204 = CARTESIAN_POINT ( 'NONE',  ( 50.46999119548826940, 1.140870969100562293, 3.938727831757874664 ) ) ;
#22205 = CARTESIAN_POINT ( 'NONE',  ( 48.39328721529930277, -1.343285922954026379, -3.873819829599202791 ) ) ;
#22206 = CARTESIAN_POINT ( 'NONE',  ( -54.46462222424374033, -1.502185874895794138, 3.301501926143236343 ) ) ;
#22207 = EDGE_CURVE ( 'NONE', #28800, #21494, #28017, .T. ) ;
#22208 = COLOUR_RGB ( '', 0.08235294, 0.09019608, 0.10196078) ;
#22209 = DIRECTION ( 'NONE',  ( 0.000000000000000000, 0.000000000000000000, 1.000000000000000000 ) ) ;
#22210 = CIRCLE ( 'NONE', #452, 0.04999999999999969746 ) ;
#22212 = CARTESIAN_POINT ( 'NONE',  ( -61.39266396720692143, -2.567250461644490223, -0.8356799977092136400 ) ) ;
#22211 = DIRECTION ( 'NONE',  ( 1.000000000000000000, 0.000000000000000000, -3.491481338843133355E-15 ) ) ;
#22213 = PRODUCT ( 'Eraser Holder', 'Eraser Holder', '', ( #23281 ) ) ;
#22214 = DIRECTION ( 'NONE',  ( 0.000000000000000000, -0.2573099415204678775, 0.9663289263986324373 ) ) ;
#22215 = DIRECTION ( 'NONE',  ( 0.000000000000000000, -1.000000000000000000, -3.491481338843129805E-15 ) ) ;
#22217 = CARTESIAN_POINT ( 'NONE',  ( 58.75000000000002132, 6.153735859711025284E-13, 3.111507638930570854E-58 ) ) ;
#22216 = CARTESIAN_POINT ( 'NONE',  ( 15.74652664997094575, 5.076023720898220404, -1.868859051106881664 ) ) ;
#22218 = ORIENTED_EDGE ( 'NONE', *, *, #30793, .T. ) ;
#22219 = CARTESIAN_POINT ( 'NONE',  ( -73.89999999999997726, 0.2499224661714811724, 0.006225825468457807203 ) ) ;
#22220 = ADVANCED_FACE ( 'NONE', ( #21699 ), #10006, .T. ) ;
#22221 = CARTESIAN_POINT ( 'NONE',  ( 51.71305322616575495, 3.851407826495535591, 1.405937361346973224 ) ) ;
#22222 = AXIS2_PLACEMENT_3D ( 'NONE', #27475, #1189, #721 ) ;
#22224 = FACE_OUTER_BOUND ( 'NONE', #12103, .T. ) ;
#22223 = CARTESIAN_POINT ( 'NONE',  ( 15.41170998834797246, 2.595074437874858031, -4.757608386865152639 ) ) ;
#22226 = EDGE_CURVE ( 'NONE', #3125, #17229, #14997, .T. ) ;
#22225 = CARTESIAN_POINT ( 'NONE',  ( -58.37499999999996447, -2.944486372867072710, -1.700000000000224443 ) ) ;
#22227 = ORIENTED_EDGE ( 'NONE', *, *, #1253, .T. ) ;
#22228 = DIRECTION ( 'NONE',  ( 0.000000000000000000, 0.000000000000000000, 1.000000000000000000 ) ) ;
#22229 = ORIENTED_EDGE ( 'NONE', *, *, #14630, .F. ) ;
#22230 = CARTESIAN_POINT ( 'NONE',  ( -61.39999999999998437, -2.604492677689918878, 0.7117709546332967596 ) ) ;
#22231 = EDGE_LOOP ( 'NONE', ( #12136, #10755, #27429, #7342 ) ) ;
#22232 = ORIENTED_EDGE ( 'NONE', *, *, #30713, .T. ) ;
#22233 = CARTESIAN_POINT ( 'NONE',  ( 58.65000000000002700, -0.5811678240976775323, -1.782657835994575724 ) ) ;
#22234 = AXIS2_PLACEMENT_3D ( 'NONE', #17278, #16671, #14273 ) ;
#22235 = ORIENTED_EDGE ( 'NONE', *, *, #6312, .T. ) ;
#22236 = SURFACE_SIDE_STYLE ('',( #20330 ) ) ;
#22237 = CARTESIAN_POINT ( 'NONE',  ( 33.82794497195008887, 8.157778427462202941, 1.949999999999882050 ) ) ;
#22238 = AXIS2_PLACEMENT_3D ( 'NONE', #26772, #14727, #24388 ) ;
#22239 = CARTESIAN_POINT ( 'NONE',  ( -55.58155989232412963, 3.925981830489463142, -1.832452953121496317E-13 ) ) ;
#22240 = VERTEX_POINT ( 'NONE', #15159 ) ;
#22241 = CARTESIAN_POINT ( 'NONE',  ( -56.56249999999997158, 3.400000000000008349, -1.863919195461974867E-13 ) ) ;
#22242 = ORIENTED_EDGE ( 'NONE', *, *, #12895, .T. ) ;
#22243 = DIRECTION ( 'NONE',  ( -1.000000000000000000, -0.000000000000000000, 3.491481338843133355E-15 ) ) ;
#22244 = FACE_OUTER_BOUND ( 'NONE', #27165, .T. ) ;
#22245 = VERTEX_POINT ( 'NONE', #13091 ) ;
#22246 = CARTESIAN_POINT ( 'NONE',  ( 51.69060524973921389, 0.7995873297242470645, -1.427997211818276435 ) ) ;
#22247 = DIRECTION ( 'NONE',  ( -0.8262273428075537218, 0.5633368246415009217, 0.000000000000000000 ) ) ;
#22248 = CARTESIAN_POINT ( 'NONE',  ( 60.81601545282717325, 0.5000000000006243894, -1.863080903339688899 ) ) ;
#22249 = CYLINDRICAL_SURFACE ( 'NONE', #11439, 0.1000000000000000472 ) ;
#22250 = EDGE_CURVE ( 'NONE', #17127, #10254, #15258, .T. ) ;
#22251 = DIRECTION ( 'NONE',  ( 1.000000000000000000, 3.053848253006669023E-16, -2.042510438544995415E-16 ) ) ;
#22252 = AXIS2_PLACEMENT_3D ( 'NONE', #12972, #15517, #29916 ) ;
#22253 = EDGE_CURVE ( 'NONE', #6234, #4064, #3761, .T. ) ;
#22254 = CARTESIAN_POINT ( 'NONE',  ( 58.75000000000002842, -1.065927491743560163, 1.652350234724849765 ) ) ;
#22255 = CARTESIAN_POINT ( 'NONE',  ( 50.25000000000000711, 1.039502773797110979, -1.650471618823823539 ) ) ;
#22256 = LINE ( 'NONE', #9747, #26601 ) ;
#22257 = AXIS2_PLACEMENT_3D ( 'NONE', #2349, #18515, #28158 ) ;
#22258 = CARTESIAN_POINT ( 'NONE',  ( -54.49998431799114940, 1.548747819918198987, -3.331336553795240185 ) ) ;
#22259 = TOROIDAL_SURFACE ( 'NONE', #13119, 4.800000000000000711, 0.05000000000000000278 ) ;
#22260 = CARTESIAN_POINT ( 'NONE',  ( -63.86464466094066239, 6.291209007590390943E-16, 2.558157268131197822E-15 ) ) ;
#22261 = VERTEX_POINT ( 'NONE', #15471 ) ;
#22262 = AXIS2_PLACEMENT_3D ( 'NONE', #10180, #1001, #27431 ) ;
#22263 = EDGE_LOOP ( 'NONE', ( #17393, #18299, #26679 ) ) ;
#22264 = VERTEX_POINT ( 'NONE', #10574 ) ;
#22265 = CARTESIAN_POINT ( 'NONE',  ( 51.80000000000001137, 6.475000000000062705, -2.050000000000180123 ) ) ;
#22266 = CARTESIAN_POINT ( 'NONE',  ( -58.04792740578360366, 3.330682475591789427, 0.6830477631804109384 ) ) ;
#22268 = CARTESIAN_POINT ( 'NONE',  ( -54.39999999999997726, -1.399999999999992806, -1.984366583318788002E-13 ) ) ;
#22267 = CARTESIAN_POINT ( 'NONE',  ( -59.29999999999997584, 2.330309927981285032E-15, 4.253626757584724400E-16 ) ) ;
#22269 = ORIENTED_EDGE ( 'NONE', *, *, #23524, .F. ) ;
#22270 = VERTEX_POINT ( 'NONE', #17705 ) ;
#22271 = CARTESIAN_POINT ( 'NONE',  ( 51.25562636158013419, -4.350642226022881864, -1.494686490729537409 ) ) ;
#22272 = ORIENTED_EDGE ( 'NONE', *, *, #25005, .F. ) ;
#22273 = DIRECTION ( 'NONE',  ( 0.000000000000000000, 0.7438053426821253922, -0.6683962987610911899 ) ) ;
#22274 = CIRCLE ( 'NONE', #20760, 2.525000000000001243 ) ;
#22275 = ORIENTED_EDGE ( 'NONE', *, *, #23659, .T. ) ;
#22276 = CARTESIAN_POINT ( 'NONE',  ( 27.52339381994850953, 5.460762561607475085, -2.050000000000095746 ) ) ;
#22277 = ORIENTED_EDGE ( 'NONE', *, *, #4819, .F. ) ;
#22278 = CARTESIAN_POINT ( 'NONE',  ( -59.19999999999997442, 2.750000000000007994, -2.007061212021268338E-13 ) ) ;
#22279 = FACE_BOUND ( 'NONE', #20323, .T. ) ;
#22280 = DIRECTION ( 'NONE',  ( -1.000000000000000000, 0.000000000000000000, 1.047444401652940007E-14 ) ) ;
#22281 = CARTESIAN_POINT ( 'NONE',  ( -60.50952994616203284, -3.117691453623963938, -1.800000000000225864 ) ) ;
#22282 = CARTESIAN_POINT ( 'NONE',  ( 54.17703590114059153, 6.867671797591380134, -2.050000000000188560 ) ) ;
#22283 = EDGE_CURVE ( 'NONE', #25749, #27693, #591, .T. ) ;
#22284 = CARTESIAN_POINT ( 'NONE',  ( 47.02542275843954656, -3.759243154119187302, -1.865745259404487655 ) ) ;
#22285 = CIRCLE ( 'NONE', #18737, 1.824999999999998623 ) ;
#22286 = EDGE_CURVE ( 'NONE', #20389, #18736, #28036, .T. ) ;
#22287 = DIRECTION ( 'NONE',  ( 1.000000000000000000, 0.000000000000000000, -1.047444401652940007E-14 ) ) ;
#22288 = EDGE_CURVE ( 'NONE', #25335, #8224, #19966, .T. ) ;
#22289 = CARTESIAN_POINT ( 'NONE',  ( 48.30000000000001847, 0.6304760106459513791, -3.950000000000021938 ) ) ;
#22290 = DIRECTION ( 'NONE',  ( 0.000000000000000000, 0.000000000000000000, -1.000000000000000000 ) ) ;
#22291 = CARTESIAN_POINT ( 'NONE',  ( 58.75000000000002132, 6.153735859711025284E-13, 3.111507638930570854E-58 ) ) ;
#22292 = CARTESIAN_POINT ( 'NONE',  ( 51.22715433738867574, -0.9941391646896066137, 1.410349289489640556 ) ) ;
#22293 = ORIENTED_EDGE ( 'NONE', *, *, #208, .F. ) ;
#22294 = CARTESIAN_POINT ( 'NONE',  ( -67.32861504302871936, -4.287230892216076523E-16, 3.265676834553754426E-15 ) ) ;
#22295 = FACE_OUTER_BOUND ( 'NONE', #11109, .T. ) ;
#22296 = CARTESIAN_POINT ( 'NONE',  ( 54.41366571437522026, 6.718673005292168376, 0.9749999999998122391 ) ) ;
#22297 = ORIENTED_EDGE ( 'NONE', *, *, #19474, .F. ) ;
#22298 = EDGE_CURVE ( 'NONE', #20361, #23664, #18459, .T. ) ;
#22299 = CARTESIAN_POINT ( 'NONE',  ( 50.46977479615469520, 1.142230555601122965, -3.938343097974785767 ) ) ;
#22300 = EDGE_LOOP ( 'NONE', ( #7180, #10750, #17267, #30521 ) ) ;
#22301 = DIRECTION ( 'NONE',  ( 1.000000000000000000, 1.047444401652940007E-14, 0.000000000000000000 ) ) ;
#22303 = CARTESIAN_POINT ( 'NONE',  ( 48.50000000000002132, -1.426739617975173013, -3.843750000000023093 ) ) ;
#22302 = CARTESIAN_POINT ( 'NONE',  ( -44.59999999999998721, -1.500000000000004663, 3.363870538531272381 ) ) ;
#22304 = EDGE_LOOP ( 'NONE', ( #16011, #12016, #29094, #14011 ) ) ;
#22305 = CARTESIAN_POINT ( 'NONE',  ( -57.49005354137802470, -3.399999999999994138, 0.9110272542655952766 ) ) ;
#22306 = CIRCLE ( 'NONE', #2572, 1.949999999999999956 ) ;
#22307 = DIRECTION ( 'NONE',  ( -3.491481338843133355E-15, -3.491481338843133355E-15, 1.000000000000000000 ) ) ;
#22308 = ORIENTED_EDGE ( 'NONE', *, *, #9624, .T. ) ;
#22310 = PLANE ( 'NONE',  #1394 ) ;
#22309 = DIRECTION ( 'NONE',  ( -0.000000000000000000, -0.000000000000000000, -1.000000000000000000 ) ) ;
#22311 = DIRECTION ( 'NONE',  ( 0.000000000000000000, -1.000000000000000000, 0.000000000000000000 ) ) ;
#22312 = CARTESIAN_POINT ( 'NONE',  ( -60.37499999999996447, 1.184343223768589803, 3.558065644182725862 ) ) ;
#22313 = CARTESIAN_POINT ( 'NONE',  ( 50.35762544161296006, 8.151359338959888845, 1.949999999999825206 ) ) ;
#22314 = CARTESIAN_POINT ( 'NONE',  ( 50.25000000000002842, -1.106298139389803925, -1.666164585742599513 ) ) ;
#22315 = LINE ( 'NONE', #17720, #27097 ) ;
#22316 = CARTESIAN_POINT ( 'NONE',  ( -59.69999999999996732, -1.873569517744609447, -3.074042495181142698 ) ) ;
#22317 = FACE_OUTER_BOUND ( 'NONE', #30481, .T. ) ;
#22318 = CARTESIAN_POINT ( 'NONE',  ( 15.18463186935387554, -1.123735532908824997, 5.289358697221508976 ) ) ;
#22319 = EDGE_LOOP ( 'NONE', ( #4877, #12740, #8432, #1203, #21374, #10950, #12699, #6566, #8223, #29635, #25718, #16664, #29637, #12448, #8921, #18992, #4053 ) ) ;
#22320 = EDGE_CURVE ( 'NONE', #28519, #24531, #26537, .T. ) ;
#22321 = EDGE_CURVE ( 'NONE', #28152, #1827, #22496, .T. ) ;
#22322 = CARTESIAN_POINT ( 'NONE',  ( 15.44631504820161005, -2.881190829692224398, 4.334245811858097319 ) ) ;
#22323 = DIRECTION ( 'NONE',  ( 3.051840300662039536E-15, 0.4857787595540328796, 0.8740818021021518058 ) ) ;
#22324 = DIRECTION ( 'NONE',  ( -1.000000000000000000, -3.053848253006669023E-16, 2.042510438544995415E-16 ) ) ;
#22325 = CARTESIAN_POINT ( 'NONE',  ( -36.11692583559843683, 4.683225668088560667, -2.703237747137714919 ) ) ;
#22326 = CARTESIAN_POINT ( 'NONE',  ( 61.25000000000003553, -0.9999999999993586242, 1.655766640118854438 ) ) ;
#22327 = DIRECTION ( 'NONE',  ( 1.000000000000000000, -1.219044193948983948E-29, 3.491481338843133355E-15 ) ) ;
#22328 = VERTEX_POINT ( 'NONE', #27664 ) ;
#22329 = ADVANCED_FACE ( 'NONE', ( #5990 ), #26005, .T. ) ;
#22330 = DIRECTION ( 'NONE',  ( 1.000000000000000000, 2.586136946169074517E-16, -0.000000000000000000 ) ) ;
#22331 = EDGE_LOOP ( 'NONE', ( #15197, #10369, #22087, #20689 ) ) ;
#22332 = CARTESIAN_POINT ( 'NONE',  ( -54.49999999999996447, 1.500000000000023981, -4.029888335922182208 ) ) ;
#22334 = CARTESIAN_POINT ( 'NONE',  ( 58.67159525762716754, -0.4999999999994943489, -1.807104036850090134 ) ) ;
#22333 = CARTESIAN_POINT ( 'NONE',  ( -54.47257281981953270, -2.332729758745841764, -2.735898203255155980 ) ) ;
#22335 = ORIENTED_EDGE ( 'NONE', *, *, #4072, .T. ) ;
#22336 = ORIENTED_EDGE ( 'NONE', *, *, #30508, .T. ) ;
#22337 = CARTESIAN_POINT ( 'NONE',  ( -59.01905989232412253, -2.944486372867095358, 1.699999999999768363 ) ) ;
#22338 = VECTOR ( 'NONE', #3576, 1000.000000000000000 ) ;
#22339 = CARTESIAN_POINT ( 'NONE',  ( 51.45655683570191741, -0.9591657938390838467, -1.611094652690527873 ) ) ;
#22340 = ORIENTED_EDGE ( 'NONE', *, *, #26819, .T. ) ;
#22342 = DIRECTION ( 'NONE',  ( 0.000000000000000000, 0.000000000000000000, -1.000000000000000000 ) ) ;
#22341 = CARTESIAN_POINT ( 'NONE',  ( -59.19702994616205416, -2.078460969082657872, 3.599999999999782041 ) ) ;
#22343 = CARTESIAN_POINT ( 'NONE',  ( 68.00000000000000000, -0.5000000000000000000, -1.988246715074070137 ) ) ;
#22344 = CARTESIAN_POINT ( 'NONE',  ( 58.75000000000004263, -1.253243060177393176, -1.394635017528124132 ) ) ;
#22345 =( LENGTH_UNIT ( ) NAMED_UNIT ( * ) SI_UNIT ( .MILLI., .METRE. ) );
#22346 = ORIENTED_EDGE ( 'NONE', *, *, #13708, .T. ) ;
#22347 = EDGE_CURVE ( 'NONE', #28844, #28012, #29547, .T. ) ;
#22348 = CIRCLE ( 'NONE', #30932, 4.275000000000000355 ) ;
#22349 = CARTESIAN_POINT ( 'NONE',  ( -58.94702994616203284, -2.078460969082631227, -3.600000000000215472 ) ) ;
#22350 = CARTESIAN_POINT ( 'NONE',  ( 51.38825337055898501, 3.875334094704443899, -2.050000000000178790 ) ) ;
#22351 = CARTESIAN_POINT ( 'NONE',  ( -60.64999999999998437, 1.610824598944129570E-15, 1.901562740512771401E-15 ) ) ;
#22352 = CARTESIAN_POINT ( 'NONE',  ( 15.41080140630216988, -0.6967302926296836674, 5.374298406429148578 ) ) ;
#22353 = DIRECTION ( 'NONE',  ( -1.047444401652940007E-14, 0.000000000000000000, -1.000000000000000000 ) ) ;
#22354 = VECTOR ( 'NONE', #13424, 1000.000000000000000 ) ;
#22355 = CARTESIAN_POINT ( 'NONE',  ( 69.25000000000001421, 3.252606517456513302E-16, -7.253552481446610839E-13 ) ) ;
#22356 = AXIS2_PLACEMENT_3D ( 'NONE', #19254, #4660, #7203 ) ;
#22358 = CARTESIAN_POINT ( 'NONE',  ( -61.38069258722538279, -2.566273914340431173, -0.8266263692889775916 ) ) ;
#22357 = FACE_OUTER_BOUND ( 'NONE', #12094, .T. ) ;
#22359 = CARTESIAN_POINT ( 'NONE',  ( 58.50000000000001421, 0.8000000000000000444, -2.489477856900920383 ) ) ;
#22360 = CARTESIAN_POINT ( 'NONE',  ( 51.45655683570189609, 0.9591657938401613182, -1.611094652690528317 ) ) ;
#22362 = CARTESIAN_POINT ( 'NONE',  ( 57.00000000000001421, -0.7137254901960804476, 2.500119182088006209 ) ) ;
#22361 = CARTESIAN_POINT ( 'NONE',  ( 54.45370770736469268, -0.0004837498569171640238, -4.360091688067994298 ) ) ;
#22363 = ORIENTED_EDGE ( 'NONE', *, *, #26168, .F. ) ;
#22364 = EDGE_CURVE ( 'NONE', #1635, #20831, #7328, .T. ) ;
#22365 = CARTESIAN_POINT ( 'NONE',  ( 50.32838854698020725, -1.409900272549264644, -3.850000494969507248 ) ) ;
#22366 = CARTESIAN_POINT ( 'NONE',  ( 47.00000000000001421, -3.933368109459638884, -2.186004417993339111 ) ) ;
#22368 = CARTESIAN_POINT ( 'NONE',  ( 52.36968054666201056, 3.911638213474379011, -1.229829597898885130 ) ) ;
#22367 = DIRECTION ( 'NONE',  ( 1.000000000000000000, 0.000000000000000000, -3.491481338843133355E-15 ) ) ;
#22369 = DIRECTION ( 'NONE',  ( 0.000000000000000000, 0.000000000000000000, -1.000000000000000000 ) ) ;
#22370 = VERTEX_POINT ( 'NONE', #28446 ) ;
#22371 = CARTESIAN_POINT ( 'NONE',  ( 51.31572262954152563, 1.002608958138273554, 1.584424273060082378 ) ) ;
#22372 = CARTESIAN_POINT ( 'NONE',  ( -60.63660384741033482, -2.460988642455861797, -1.107171701358785620 ) ) ;
#22373 = EDGE_LOOP ( 'NONE', ( #2647, #7567, #21379, #24752 ) ) ;
#22374 = LINE ( 'NONE', #13016, #8345 ) ;
#22375 = EDGE_LOOP ( 'NONE', ( #9969, #6451, #30689, #9540 ) ) ;
#22376 = EDGE_CURVE ( 'NONE', #6162, #25369, #8312, .T. ) ;
#22377 = ORIENTED_EDGE ( 'NONE', *, *, #13610, .F. ) ;
#22378 = CARTESIAN_POINT ( 'NONE',  ( 15.97944027357901042, 5.289443499204828925, -1.131445731060737980 ) ) ;
#22379 = ORIENTED_EDGE ( 'NONE', *, *, #14883, .T. ) ;
#22380 = CARTESIAN_POINT ( 'NONE',  ( 29.90503599876537777, 6.470972976943354382, 1.949999999999894040 ) ) ;
#22381 = CARTESIAN_POINT ( 'NONE',  ( -55.08155989232411542, -1.962990915244706924, -3.400000000000202416 ) ) ;
#22382 = ORIENTED_EDGE ( 'NONE', *, *, #22855, .F. ) ;
#22383 = CARTESIAN_POINT ( 'NONE',  ( 51.25000000000002842, -1.099999999999459410, 1.001327244211406953 ) ) ;
#22384 = VERTEX_POINT ( 'NONE', #13706 ) ;
#22385 = DIRECTION ( 'NONE',  ( 1.000000000000000000, 1.047444401652940007E-14, 0.000000000000000000 ) ) ;
#22386 = ORIENTED_EDGE ( 'NONE', *, *, #30454, .T. ) ;
#22387 = EDGE_CURVE ( 'NONE', #11253, #14068, #6301, .T. ) ;
#22388 =( BOUNDED_SURFACE ( )  B_SPLINE_SURFACE ( 1, 2, ( 
 ( #1970, #11634, #21313, #17716, #14775, #2120, #2273, #24292, #24433, #24138, #2744, #19551, #12248, #21626, #29196, #214, #5122, #12105, #7048, #21786, #71, #29035, #12390, #16861, #4971, #17017, #23829, #2446, #9876, #9732, #26671, #19393, #16709, #26498, #26351, #22080, #7197, #4501, #7344, #14463, #31261, #4803, #14625, #18921, #2602, #21931, #7510, #26196, #17173, #26817, #9259, #28563, #6875, #16544, #9414, #19083, #28885, #14155, #11782, #21457, #31088, #28736, #4654, #14307, #23978, #11938, #9588, #19247, #1002, #24749, #20178, #27116, #10181, #525, #22532, #25215, #8123, #19850, #836, #15393, #17937, #20333, #15568, #15245, #5743, #671, #25044, #3535, #12550, #17793, #10331, #17464, #7971, #26957, #19709, #5909, #29343, #10505, #3207, #3059, #29811, #13171, #29479, #5437, #20003, #12701, #7795, #2904, #3374 ),
 ( #29644, #375, #10040, #13025, #15090, #7653, #10655, #22707, #29962, #27432, #8269, #27578, #17314, #22381, #5267, #17634, #27280, #14918, #24583, #5598, #12850, #22239, #24891, #20940, #30420, #15861, #11424, #6211, #3987, #18731, #22858, #1146, #6070, #20793, #20482, #1600, #16341, #23171, #28373, #15721, #25516, #6527, #6676, #6361, #25985, #1755, #25835, #3827, #21114, #13779, #4293, #25684, #20646, #13631, #23317, #11261, #10798, #8723, #18571, #30570, #25368, #16023, #23463, #8881, #28221, #16187, #30273, #18407, #8580, #30105, #28046, #18112, #4143, #30752, #13474, #9058, #8428, #27749, #3674, #13310, #23002, #1292, #10957, #18262, #27900, #1454, #11114, #19360, #14115, #23793, #2233, #16974, #14420, #7162, #1934, #21583, #13941, #2083, #11594, #21744, #26784, #28847, #18881, #16824, #28525, #11897, #7470, #34, #11747 ) ),
 .UNSPECIFIED., .F., .F., .F. ) 
 B_SPLINE_SURFACE_WITH_KNOTS ( ( 2, 2 ),
 ( 3, 2, 2, 2, 2, 2, 2, 2, 2, 2, 2, 2, 2, 2, 2, 2, 2, 2, 2, 2, 2, 2, 2, 2, 2, 2, 2, 2, 2, 2, 2, 2, 2, 2, 2, 2, 2, 2, 2, 2, 2, 2, 2, 2, 2, 2, 2, 2, 2, 2, 2, 2, 2, 2, 3 ),
 ( 0.000000000000000000, 1.000000000000000000 ),
 ( 0.000000000000000000, 0.01851851851851851749, 0.03703703703703703498, 0.05555555555555555247, 0.07407407407407406996, 0.09259259259259258745, 0.1111111111111111049, 0.1296296296296296224, 0.1481481481481481399, 0.1666666666666666574, 0.1851851851851851749, 0.2037037037037036924, 0.2222222222222222099, 0.2407407407407407274, 0.2592592592592592449, 0.2777777777777777901, 0.2962962962962962798, 0.3148148148148148251, 0.3333333333333333148, 0.3518518518518518601, 0.3703703703703703498, 0.3888888888888888951, 0.4074074074074073848, 0.4259259259259259300, 0.4444444444444444198, 0.4629629629629629650, 0.4814814814814814548, 0.5000000000000000000, 0.5185185185185184897, 0.5370370370370370905, 0.5555555555555555802, 0.5740740740740740700, 0.5925925925925925597, 0.6111111111111111605, 0.6296296296296296502, 0.6481481481481481399, 0.6666666666666666297, 0.6851851851851852304, 0.7037037037037037202, 0.7222222222222222099, 0.7407407407407406996, 0.7592592592592593004, 0.7777777777777777901, 0.7962962962962962798, 0.8148148148148147696, 0.8333333333333333703, 0.8518518518518518601, 0.8703703703703703498, 0.8888888888888888395, 0.9074074074074074403, 0.9259259259259259300, 0.9444444444444444198, 0.9629629629629629095, 0.9814814814814815103, 1.000000000000000000 ),
 .UNSPECIFIED. ) 
 GEOMETRIC_REPRESENTATION_ITEM ( )  RATIONAL_B_SPLINE_SURFACE ( (
 ( 1.000000000000000000, 0.8660254037844387076, 1.000000000000000000, 0.8660254037844387076, 1.000000000000000000, 0.8660254037844387076, 1.000000000000000000, 0.8660254037844387076, 1.000000000000000000, 0.8660254037844387076, 1.000000000000000000, 0.8660254037844387076, 1.000000000000000000, 0.8660254037844387076, 1.000000000000000000, 0.8660254037844387076, 1.000000000000000000, 0.8660254037844387076, 1.000000000000000000, 0.8660254037844387076, 1.000000000000000000, 0.8660254037844387076, 1.000000000000000000, 0.8660254037844387076, 1.000000000000000000, 0.8660254037844387076, 1.000000000000000000, 0.8660254037844387076, 1.000000000000000000, 0.8660254037844387076, 1.000000000000000000, 0.8660254037844387076, 1.000000000000000000, 0.8660254037844387076, 1.000000000000000000, 0.8660254037844387076, 1.000000000000000000, 0.8660254037844387076, 1.000000000000000000, 0.8660254037844387076, 1.000000000000000000, 0.8660254037844387076, 1.000000000000000000, 0.8660254037844387076, 1.000000000000000000, 0.8660254037844387076, 1.000000000000000000, 0.8660254037844387076, 1.000000000000000000, 0.8660254037844387076, 1.000000000000000000, 0.8660254037844387076, 1.000000000000000000, 0.8660254037844387076, 1.000000000000000000, 0.8660254037844387076, 1.000000000000000000, 0.8660254037844387076, 1.000000000000000000, 0.8660254037844387076, 1.000000000000000000, 0.8660254037844387076, 1.000000000000000000, 0.8660254037844387076, 1.000000000000000000, 0.8660254037844387076, 1.000000000000000000, 0.8660254037844387076, 1.000000000000000000, 0.8660254037844387076, 1.000000000000000000, 0.8660254037844387076, 1.000000000000000000, 0.8660254037844387076, 1.000000000000000000, 0.8660254037844387076, 1.000000000000000000, 0.8660254037844387076, 1.000000000000000000, 0.8660254037844387076, 1.000000000000000000, 0.8660254037844387076, 1.000000000000000000, 0.8660254037844387076, 1.000000000000000000, 0.8660254037844387076, 1.000000000000000000, 0.8660254037844387076, 1.000000000000000000, 0.8660254037844387076, 1.000000000000000000, 0.8660254037844387076, 1.000000000000000000, 0.8660254037844387076, 1.000000000000000000, 0.8660254037844387076, 1.000000000000000000, 0.8660254037844387076, 1.000000000000000000, 0.8660254037844387076, 1.000000000000000000, 0.8660254037844387076, 1.000000000000000000, 0.8660254037844387076, 1.000000000000000000, 0.8660254037844387076, 1.000000000000000000, 0.8660254037844387076, 1.000000000000000000),
 ( 1.000000000000000000, 0.8660254037844387076, 1.000000000000000000, 0.8660254037844387076, 1.000000000000000000, 0.8660254037844387076, 1.000000000000000000, 0.8660254037844387076, 1.000000000000000000, 0.8660254037844387076, 1.000000000000000000, 0.8660254037844387076, 1.000000000000000000, 0.8660254037844387076, 1.000000000000000000, 0.8660254037844387076, 1.000000000000000000, 0.8660254037844387076, 1.000000000000000000, 0.8660254037844387076, 1.000000000000000000, 0.8660254037844387076, 1.000000000000000000, 0.8660254037844387076, 1.000000000000000000, 0.8660254037844387076, 1.000000000000000000, 0.8660254037844387076, 1.000000000000000000, 0.8660254037844387076, 1.000000000000000000, 0.8660254037844387076, 1.000000000000000000, 0.8660254037844387076, 1.000000000000000000, 0.8660254037844387076, 1.000000000000000000, 0.8660254037844387076, 1.000000000000000000, 0.8660254037844387076, 1.000000000000000000, 0.8660254037844387076, 1.000000000000000000, 0.8660254037844387076, 1.000000000000000000, 0.8660254037844387076, 1.000000000000000000, 0.8660254037844387076, 1.000000000000000000, 0.8660254037844387076, 1.000000000000000000, 0.8660254037844387076, 1.000000000000000000, 0.8660254037844387076, 1.000000000000000000, 0.8660254037844387076, 1.000000000000000000, 0.8660254037844387076, 1.000000000000000000, 0.8660254037844387076, 1.000000000000000000, 0.8660254037844387076, 1.000000000000000000, 0.8660254037844387076, 1.000000000000000000, 0.8660254037844387076, 1.000000000000000000, 0.8660254037844387076, 1.000000000000000000, 0.8660254037844387076, 1.000000000000000000, 0.8660254037844387076, 1.000000000000000000, 0.8660254037844387076, 1.000000000000000000, 0.8660254037844387076, 1.000000000000000000, 0.8660254037844387076, 1.000000000000000000, 0.8660254037844387076, 1.000000000000000000, 0.8660254037844387076, 1.000000000000000000, 0.8660254037844387076, 1.000000000000000000, 0.8660254037844387076, 1.000000000000000000, 0.8660254037844387076, 1.000000000000000000, 0.8660254037844387076, 1.000000000000000000, 0.8660254037844387076, 1.000000000000000000, 0.8660254037844387076, 1.000000000000000000, 0.8660254037844387076, 1.000000000000000000, 0.8660254037844387076, 1.000000000000000000, 0.8660254037844387076, 1.000000000000000000, 0.8660254037844387076, 1.000000000000000000, 0.8660254037844387076, 1.000000000000000000, 0.8660254037844387076, 1.000000000000000000, 0.8660254037844387076, 1.000000000000000000) ) ) 
 REPRESENTATION_ITEM ( '' )  SURFACE ( )  );
#22389 = CARTESIAN_POINT ( 'NONE',  ( 51.79694101351947211, -4.143816080048276618, -1.075455348895917984 ) ) ;
#22390 = ADVANCED_FACE ( 'NONE', ( #4211 ), #1672, .T. ) ;
#22391 = CARTESIAN_POINT ( 'NONE',  ( -54.46439202372638277, -1.502116081466616793, 4.031358338852112588 ) ) ;
#22392 = LINE ( 'NONE', #29490, #5139 ) ;
#22393 = CIRCLE ( 'NONE', #29444, 4.600000000000036948 ) ;
#22395 = EDGE_CURVE ( 'NONE', #22708, #14986, #1838, .T. ) ;
#22394 = CARTESIAN_POINT ( 'NONE',  ( 51.80000000000001137, -4.291790910095606648, -1.352971095042662553 ) ) ;
#22396 = CARTESIAN_POINT ( 'NONE',  ( 57.00174889577907322, -0.7131084301676396953, 2.444403622924161912 ) ) ;
#22398 = CARTESIAN_POINT ( 'NONE',  ( 50.25000000000000000, 2.008165151418772609, -0.5380862305899540843 ) ) ;
#22397 = CARTESIAN_POINT ( 'NONE',  ( -36.92443669619772351, -3.305069970238164956, 4.282766538619550367 ) ) ;
#22399 = CARTESIAN_POINT ( 'NONE',  ( 50.50000000000002132, -0.7900853852131047850, -4.025789903357282817 ) ) ;
#22400 = CARTESIAN_POINT ( 'NONE',  ( 58.64999999999999858, 1.872332544501833507, -0.09997921184724666011 ) ) ;
#22401 = B_SPLINE_CURVE_WITH_KNOTS ( 'NONE', 3,
 ( #1851, #9151, #18812, #23871, #25238, #3557, #6090, #15741, #27922, #16055, #28071, #13194, #13506, #20964, #11137, #6390 ),
 .UNSPECIFIED., .F., .F.,
 ( 4, 2, 2, 2, 2, 2, 2, 4 ),
 ( 0.000000000000000000, 0.0004351083927046427526, 0.0008702167854092855053, 0.001740433570818570794, 0.002175541963523213926, 0.002610650356227856624, 0.003045758748932499323, 0.003480867141637142021 ),
 .UNSPECIFIED. ) ;
#22402 = EDGE_CURVE ( 'NONE', #24313, #9750, #30564, .T. ) ;
#22403 = EDGE_LOOP ( 'NONE', ( #30755, #19983, #15887, #28560 ) ) ;
#22404 = CARTESIAN_POINT ( 'NONE',  ( -54.46462222424374033, 1.502185874895793694, 3.301501926143237675 ) ) ;
#22405 = ORIENTED_EDGE ( 'NONE', *, *, #14110, .F. ) ;
#22406 = ORIENTED_EDGE ( 'NONE', *, *, #2137, .F. ) ;
#22407 = FACE_OUTER_BOUND ( 'NONE', #12518, .T. ) ;
#22408 = CIRCLE ( 'NONE', #20899, 0.1500000000000003830 ) ;
#22409 = CARTESIAN_POINT ( 'NONE',  ( -60.29792740578359656, 3.330682475591789427, 0.6830477631804114935 ) ) ;
#22410 = DIRECTION ( 'NONE',  ( 0.000000000000000000, 0.000000000000000000, 1.000000000000000000 ) ) ;
#22411 = ORIENTED_EDGE ( 'NONE', *, *, #9236, .F. ) ;
#22412 = ADVANCED_FACE ( 'NONE', ( #30653 ), #22921, .T. ) ;
#22413 = VERTEX_POINT ( 'NONE', #16260 ) ;
#22414 = CARTESIAN_POINT ( 'NONE',  ( -67.97846802697301882, -3.201166483080443511E-16, 2.197917219923980763E-15 ) ) ;
#22415 = ORIENTED_EDGE ( 'NONE', *, *, #28566, .F. ) ;
#22416 = CARTESIAN_POINT ( 'NONE',  ( -59.69999999999997442, 8.366749974758454467E-15, -2.120534355533670266E-13 ) ) ;
#22417 = ORIENTED_EDGE ( 'NONE', *, *, #5241, .F. ) ;
#22418 = CARTESIAN_POINT ( 'NONE',  ( 25.99900894223008763, 5.212247165294384921, -1.950000000000091438 ) ) ;
#22419 = EDGE_CURVE ( 'NONE', #9403, #28571, #10868, .T. ) ;
#22420 = CARTESIAN_POINT ( 'NONE',  ( -57.33155989232411542, -1.962990915244702039, -3.400000000000212630 ) ) ;
#22421 = CARTESIAN_POINT ( 'NONE',  ( -58.93749999999996447, 1.962990915244761991, -3.400000000000193534 ) ) ;
#22422 = ORIENTED_EDGE ( 'NONE', *, *, #24476, .T. ) ;
#22423 = CARTESIAN_POINT ( 'NONE',  ( 15.03925126672126034, -4.861582140531611529, -2.394243978978356502 ) ) ;
#22424 = EDGE_CURVE ( 'NONE', #7997, #66, #22995, .T. ) ;
#22425 = CARTESIAN_POINT ( 'NONE',  ( -59.33155989232412253, 3.925981830489463142, -1.963383503328113345E-13 ) ) ;
#22427 = EDGE_CURVE ( 'NONE', #26529, #4543, #28124, .T. ) ;
#22426 = CARTESIAN_POINT ( 'NONE',  ( 51.65313719492860400, 3.829415913202794286, -2.050000000000180123 ) ) ;
#22428 = CARTESIAN_POINT ( 'NONE',  ( 47.76297833550881222, -3.901511898670463108, -1.261029562208496824 ) ) ;
#22429 = CARTESIAN_POINT ( 'NONE',  ( 50.59602332238209499, 0.1408342061609078322, 1.212874140286674063 ) ) ;
#22430 = DIRECTION ( 'NONE',  ( 0.000000000000000000, -1.000000000000000000, 0.000000000000000000 ) ) ;
#22431 = CARTESIAN_POINT ( 'NONE',  ( 50.30000000000001847, 1.426739617975228525, -3.843750000000022649 ) ) ;
#22432 = AXIS2_PLACEMENT_3D ( 'NONE', #17735, #22330, #15337 ) ;
#22433 = CIRCLE ( 'NONE', #14818, 1.613789466889706814 ) ;
#22434 = CARTESIAN_POINT ( 'NONE',  ( 51.80000000000001847, 2.428612866367529932E-14, -1.808587333520743709E-13 ) ) ;
#22435 = CARTESIAN_POINT ( 'NONE',  ( 58.65000000000003411, -1.571497941946114363, -1.022750809560766694 ) ) ;
#22436 = VERTEX_POINT ( 'NONE', #3599 ) ;
#22437 = CARTESIAN_POINT ( 'NONE',  ( -59.29999999999997584, 0.05651759653475140616, 3.560132860530125232 ) ) ;
#22438 = CARTESIAN_POINT ( 'NONE',  ( -36.89017861347172555, -3.436881753486550561, -4.177093996075186055 ) ) ;
#22439 = CARTESIAN_POINT ( 'NONE',  ( 54.28770169842803028, 6.706929334265034903, 2.049999999999810196 ) ) ;
#22440 = ORIENTED_EDGE ( 'NONE', *, *, #9944, .F. ) ;
#22441 = CYLINDRICAL_SURFACE ( 'NONE', #26978, 0.1499999999999998557 ) ;
#22442 = ORIENTED_EDGE ( 'NONE', *, *, #9417, .F. ) ;
#22443 =( BOUNDED_CURVE ( )  B_SPLINE_CURVE ( 3, ( #25930, #30685, #3933, #18667 ),
 .UNSPECIFIED., .F., .T. ) 
 B_SPLINE_CURVE_WITH_KNOTS ( ( 4, 4 ),
 ( 0.8272220676012492779, 0.8437250283369831516 ),
 .UNSPECIFIED. ) 
 CURVE ( )  GEOMETRIC_REPRESENTATION_ITEM ( )  RATIONAL_B_SPLINE_CURVE ( ( 1.000000000000000000, 0.9999773044860189586, 0.9999773044860189586, 1.000000000000000000 ) ) 
 REPRESENTATION_ITEM ( '' )  );
#22444 = DIRECTION ( 'NONE',  ( 0.000000000000000000, 0.9996898646859344595, 0.02490330187381124827 ) ) ;
#22445 = CARTESIAN_POINT ( 'NONE',  ( -54.09585481156724285, 3.673546848079182858, 0.7533615035078057298 ) ) ;
#22447 = FACE_OUTER_BOUND ( 'NONE', #21673, .T. ) ;
#22446 = CARTESIAN_POINT ( 'NONE',  ( 58.75000000000002132, 6.153735859711025284E-13, 3.111507638930570854E-58 ) ) ;
#22448 = EDGE_LOOP ( 'NONE', ( #15749, #20203, #23241, #30973 ) ) ;
#22449 = EDGE_CURVE ( 'NONE', #5154, #21603, #27747, .T. ) ;
#22450 = CARTESIAN_POINT ( 'NONE',  ( 61.20598745287938414, -0.7563774268552496682, -1.657497327210055493 ) ) ;
#22451 = ADVANCED_FACE ( 'NONE', ( #14021 ), #7377, .T. ) ;
#22452 = CARTESIAN_POINT ( 'NONE',  ( 57.00074754615238248, -0.7099475343046129927, -1.812279303590036639 ) ) ;
#22453 = ORIENTED_EDGE ( 'NONE', *, *, #27708, .T. ) ;
#22455 = CARTESIAN_POINT ( 'NONE',  ( -54.47710365256552478, -1.507983431629474014, -4.035431478432994545 ) ) ;
#22454 = CARTESIAN_POINT ( 'NONE',  ( 64.94999999999997442, 1.401298464324817071E-42, -3.950000000000680522 ) ) ;
#22456 = ORIENTED_EDGE ( 'NONE', *, *, #27340, .F. ) ;
#22457 = EDGE_LOOP ( 'NONE', ( #4316, #21491, #15121, #14332, #23313, #11280 ) ) ;
#22458 = CARTESIAN_POINT ( 'NONE',  ( -57.87499999999997158, -3.673546848079173976, -0.7533615035078061739 ) ) ;
#22459 = CARTESIAN_POINT ( 'NONE',  ( -56.12499999999996447, -2.944486372867074042, -1.700000000000214673 ) ) ;
#22460 = CARTESIAN_POINT ( 'NONE',  ( -54.83155989232413674, 3.400000000000008349, -1.845326485282803322E-13 ) ) ;
#22461 = DIRECTION ( 'NONE',  ( 1.000000000000000000, 1.047444401652940007E-14, 0.000000000000000000 ) ) ;
#22462 = CARTESIAN_POINT ( 'NONE',  ( -55.13452994616203995, 2.093608279459367933E-14, -3.600000000000195932 ) ) ;
#22463 = CARTESIAN_POINT ( 'NONE',  ( 51.80000000000001137, 6.475000000000062705, -1.950000000000180256 ) ) ;
#22465 = ORIENTED_EDGE ( 'NONE', *, *, #16997, .T. ) ;
#22464 = AXIS2_PLACEMENT_3D ( 'NONE', #29539, #10391, #27919 ) ;
#22466 = CARTESIAN_POINT ( 'NONE',  ( 15.03925126672127810, 2.686240680702102868, 4.475885388010754085 ) ) ;
#22467 = CIRCLE ( 'NONE', #20955, 0.05000000000000012074 ) ;
#22468 = CARTESIAN_POINT ( 'NONE',  ( -60.60214168571716442, -2.489792084731451194, 0.9488797246527581608 ) ) ;
#22469 = CARTESIAN_POINT ( 'NONE',  ( 51.90000000000001990, -4.241638912518127746, 1.073342218585537466 ) ) ;
#22470 = CIRCLE ( 'NONE', #204, 0.1499999999999999667 ) ;
#22471 = CARTESIAN_POINT ( 'NONE',  ( -57.75952994616205416, -2.096020771799606953E-14, 3.599999999999794031 ) ) ;
#22472 = CARTESIAN_POINT ( 'NONE',  ( -35.85663232820581214, 0.7747498368337695229, 5.363501452440937456 ) ) ;
#22473 = CARTESIAN_POINT ( 'NONE',  ( 22.11595495846478343, 7.781273941107792247, 2.049999999999922107 ) ) ;
#22474 = EDGE_LOOP ( 'NONE', ( #24325, #548, #30791, #28839, #24253, #9985, #8154, #1630, #23624, #19126 ) ) ;
#22475 = CARTESIAN_POINT ( 'NONE',  ( -54.49999999999996447, 2.023778652682504319E-14, -3.400000000000193978 ) ) ;
#22476 = EDGE_LOOP ( 'NONE', ( #18538, #19697, #17137, #18796 ) ) ;
#22477 = UNCERTAINTY_MEASURE_WITH_UNIT (LENGTH_MEASURE( 1.000000000000000082E-05 ), #9070, 'distance_accuracy_value', 'NONE');
#22478 = DIRECTION ( 'NONE',  ( 0.000000000000000000, 0.3333333333333358683, -0.9428090415820624681 ) ) ;
#22479 = VECTOR ( 'NONE', #9805, 1000.000000000000000 ) ;
#22481 = CARTESIAN_POINT ( 'NONE',  ( -54.44999999999997442, 0.000000000000000000, 0.000000000000000000 ) ) ;
#22480 = CARTESIAN_POINT ( 'NONE',  ( 57.02888566337306031, 0.7456496514153734267, -2.424120212325347357 ) ) ;
#22482 = ORIENTED_EDGE ( 'NONE', *, *, #13405, .T. ) ;
#22483 = ORIENTED_EDGE ( 'NONE', *, *, #19889, .T. ) ;
#22484 = CARTESIAN_POINT ( 'NONE',  ( -59.68658240507107138, -2.223882124562203799, 1.531065007683262591 ) ) ;
#22485 = EDGE_CURVE ( 'NONE', #9864, #18872, #2153, .T. ) ;
#22486 = DIRECTION ( 'NONE',  ( 0.000000000000000000, 0.000000000000000000, 1.000000000000000000 ) ) ;
#22487 = ORIENTED_EDGE ( 'NONE', *, *, #30491, .F. ) ;
#22489 = CARTESIAN_POINT ( 'NONE',  ( 50.59602332238209499, 0.1408342061609073048, 0.8215393206232031176 ) ) ;
#22488 = CARTESIAN_POINT ( 'NONE',  ( -59.13452994616204705, -3.117691453623976816, 1.799999999999778000 ) ) ;
#22490 = CARTESIAN_POINT ( 'NONE',  ( -54.42292740578361077, 2.256877952708269852, -2.542931754211926076 ) ) ;
#22491 = CIRCLE ( 'NONE', #20980, 1.975000000000001865 ) ;
#22492 = CIRCLE ( 'NONE', #13370, 0.4576450603546982632 ) ;
#22493 = DIRECTION ( 'NONE',  ( 1.168655815394902336E-14, 0.000000000000000000, 1.000000000000000000 ) ) ;
#22494 = DIRECTION ( 'NONE',  ( 0.000000000000000000, 0.000000000000000000, 1.000000000000000000 ) ) ;
#22495 = CARTESIAN_POINT ( 'NONE',  ( 58.66118217212504504, -1.337770226785847338, -1.313877211063244621 ) ) ;
#22496 = CIRCLE ( 'NONE', #11870, 2.263970382088065225 ) ;
#22497 = EDGE_LOOP ( 'NONE', ( #8103, #5559, #20218, #16251, #17132 ) ) ;
#22498 = EDGE_CURVE ( 'NONE', #3131, #29448, #254, .T. ) ;
#22499 = CARTESIAN_POINT ( 'NONE',  ( -58.57202994616204705, 2.078460969082646770, 3.599999999999799805 ) ) ;
#22500 = CIRCLE ( 'NONE', #25010, 1.000000000000000000 ) ;
#22501 = CARTESIAN_POINT ( 'NONE',  ( -59.09999999999997300, 2.650000000000008349, -1.759412204284508433E-13 ) ) ;
#22502 = CARTESIAN_POINT ( 'NONE',  ( -56.70655989232412253, -3.399999999999991029, -2.112596694108398482E-13 ) ) ;
#22503 = CYLINDRICAL_SURFACE ( 'NONE', #7392, 0.1000000000000000472 ) ;
#22504 = CARTESIAN_POINT ( 'NONE',  ( -54.81249999999998579, -1.962990915244732015, 3.399999999999796962 ) ) ;
#22506 = DIRECTION ( 'NONE',  ( 0.000000000000000000, 0.000000000000000000, -1.000000000000000000 ) ) ;
#22505 = CARTESIAN_POINT ( 'NONE',  ( -56.56249999999997158, 3.400000000000008349, -1.863919195461974867E-13 ) ) ;
#22507 = TOROIDAL_SURFACE ( 'NONE', #20008, 3.524999999999996358, 0.1000000000000000056 ) ;
#22508 = CARTESIAN_POINT ( 'NONE',  ( -62.07735545010103806, -2.517494014746469499, 0.1945804328892600521 ) ) ;
#22509 = DIRECTION ( 'NONE',  ( -1.000000000000000000, 0.000000000000000000, 1.047444401652940007E-14 ) ) ;
#22511 = FACE_OUTER_BOUND ( 'NONE', #12428, .T. ) ;
#22510 = CARTESIAN_POINT ( 'NONE',  ( -59.43749999999997868, 1.962990915244716028, 3.399999999999800071 ) ) ;
#22512 = VERTEX_POINT ( 'NONE', #26229 ) ;
#22513 = FACE_OUTER_BOUND ( 'NONE', #14495, .T. ) ;
#22514 = VECTOR ( 'NONE', #7191, 1000.000000000000000 ) ;
#22515 = DIRECTION ( 'NONE',  ( 0.000000000000000000, 0.2008964009354147484, -0.9796124928211139560 ) ) ;
#22517 = CARTESIAN_POINT ( 'NONE',  ( -59.41132486539680713, 3.361433066165957051, 1.250136525132557574 ) ) ;
#22516 = CARTESIAN_POINT ( 'NONE',  ( 15.41217651307625580, 3.272340825137240117, -4.050058705652119784 ) ) ;
#22518 = CARTESIAN_POINT ( 'NONE',  ( 15.56274145962647104, -5.369990034204302098, 0.6654225812208781621 ) ) ;
#22519 = ORIENTED_EDGE ( 'NONE', *, *, #10477, .F. ) ;
#22520 = CARTESIAN_POINT ( 'NONE',  ( -61.35192115139415137, -2.623188642970683215, 0.4629488832698942513 ) ) ;
#22521 = CARTESIAN_POINT ( 'NONE',  ( 47.00101556927586444, -4.139722501993201575, 1.083525984490929961 ) ) ;
#22522 = ADVANCED_FACE ( 'NONE', ( #7226 ), #23508, .T. ) ;
#22523 = ORIENTED_EDGE ( 'NONE', *, *, #17070, .T. ) ;
#22524 = TOROIDAL_SURFACE ( 'NONE', #23023, 0.2000000000000000111, 0.1000000000000000056 ) ;
#22525 = CARTESIAN_POINT ( 'NONE',  ( 16.10660252424456829, -5.053896291911978977, 1.944420249220634833 ) ) ;
#22526 = ORIENTED_EDGE ( 'NONE', *, *, #23161, .T. ) ;
#22527 = ORIENTED_EDGE ( 'NONE', *, *, #15742, .F. ) ;
#22528 = DIRECTION ( 'NONE',  ( 0.000000000000000000, 0.2008964009354143876, -0.9796124928211140670 ) ) ;
#22529 = CARTESIAN_POINT ( 'NONE',  ( 47.10000000000000853, -4.020776289669854009, -2.234582293948742748 ) ) ;
#22530 = ORIENTED_EDGE ( 'NONE', *, *, #5323, .T. ) ;
#22531 = CARTESIAN_POINT ( 'NONE',  ( 26.83497762440962120, 5.238776824946374866, 1.949999999999906031 ) ) ;
#22532 = CARTESIAN_POINT ( 'NONE',  ( -59.00952994616203284, -3.117691453623963938, -1.800000000000220757 ) ) ;
#22533 = ORIENTED_EDGE ( 'NONE', *, *, #24833, .T. ) ;
#22534 = CARTESIAN_POINT ( 'NONE',  ( 61.09423418604053069, -0.6373668173463740150, -1.895722432252557432 ) ) ;
#22535 = VERTEX_POINT ( 'NONE', #26708 ) ;
#22536 = DIRECTION ( 'NONE',  ( -0.000000000000000000, 0.000000000000000000, 1.000000000000000000 ) ) ;
#22537 = CIRCLE ( 'NONE', #21031, 0.1000000000000000472 ) ;
#22538 = VECTOR ( 'NONE', #7701, 1000.000000000000000 ) ;
#22539 = CARTESIAN_POINT ( 'NONE',  ( 24.76493886329451399, 5.404133871416378021, 1.949999999999914468 ) ) ;
#22540 = VERTEX_POINT ( 'NONE', #18957 ) ;
#22541 = AXIS2_PLACEMENT_3D ( 'NONE', #31245, #28870, #7181 ) ;
#22542 = EDGE_CURVE ( 'NONE', #30886, #15970, #21959, .T. ) ;
#22543 = CARTESIAN_POINT ( 'NONE',  ( 51.77770663993858591, -4.163003037071927537, -1.036150823695777934 ) ) ;
#22544 = CARTESIAN_POINT ( 'NONE',  ( 60.97799375661035981, 0.7610968749155430091, 1.436497712332769794 ) ) ;
#22545 = LINE ( 'NONE', #27440, #7671 ) ;
#22546 = CARTESIAN_POINT ( 'NONE',  ( 57.00914817631336717, -0.7715555436188452632, -1.736293111776144205 ) ) ;
#22547 = TOROIDAL_SURFACE ( 'NONE', #4336, 0.2000000000000000111, 0.1000000000000000056 ) ;
#22548 = CARTESIAN_POINT ( 'NONE',  ( -59.29999999999997584, 0.7533615035078071731, -3.673546848079177529 ) ) ;
#22549 = VECTOR ( 'NONE', #23051, 1000.000000000000000 ) ;
#22550 = PRESENTATION_LAYER_ASSIGNMENT (  '', '', ( #4846 ) ) ;
#22552 = CARTESIAN_POINT ( 'NONE',  ( 50.50000000000001421, 0.7375000000005331735, 3.111507638930570854E-58 ) ) ;
#22551 = DIRECTION ( 'NONE',  ( -3.352440544655105674E-15, 0.2793919678926571892, -0.9601771338024399638 ) ) ;
#22553 = EDGE_CURVE ( 'NONE', #12097, #29156, #2758, .T. ) ;
#22554 = CARTESIAN_POINT ( 'NONE',  ( 58.66324791596930055, -0.4999999999993858246, 1.807104036850105899 ) ) ;
#22555 = CARTESIAN_POINT ( 'NONE',  ( -59.69999999999998153, 2.120235050790597153, 1.750136525132547360 ) ) ;
#22556 = CARTESIAN_POINT ( 'NONE',  ( 58.75000018595668649, 1.333791840693631103, -1.404395290252168360 ) ) ;
#22557 = CARTESIAN_POINT ( 'NONE',  ( 48.30000000000001847, -0.7900853852131047850, 4.025789903357282817 ) ) ;
#22558 = ORIENTED_EDGE ( 'NONE', *, *, #18817, .T. ) ;
#22559 = CARTESIAN_POINT ( 'NONE',  ( 58.65000000000000568, 1.022750809560621921, 1.571497941947222587 ) ) ;
#22560 = AXIS2_PLACEMENT_3D ( 'NONE', #12326, #12193, #26441 ) ;
#22561 = CIRCLE ( 'NONE', #14461, 4.100000000000000533 ) ;
#22562 = EDGE_LOOP ( 'NONE', ( #19817, #1971, #18637, #20862 ) ) ;
#22563 = EDGE_CURVE ( 'NONE', #3627, #2662, #13872, .T. ) ;
#22564 = AXIS2_PLACEMENT_3D ( 'NONE', #10056, #2925, #2617 ) ;
#22565 = ORIENTED_EDGE ( 'NONE', *, *, #10739, .T. ) ;
#22566 = EDGE_CURVE ( 'NONE', #6992, #20708, #21985, .T. ) ;
#22567 = CARTESIAN_POINT ( 'NONE',  ( -73.85208152723558328, 1.351577301140750587, 0.03366917953767410016 ) ) ;
#22568 = CARTESIAN_POINT ( 'NONE',  ( -57.86042740578360366, -0.7887156198831604126, 3.845940847736174284 ) ) ;
#22570 = DIRECTION ( 'NONE',  ( 1.000000000000000000, 0.000000000000000000, 0.000000000000000000 ) ) ;
#22569 = CARTESIAN_POINT ( 'NONE',  ( -56.87499999999996447, -2.944486372867076707, -1.700000000000212674 ) ) ;
#22571 = EDGE_CURVE ( 'NONE', #8746, #9260, #30044, .T. ) ;
#22572 = ORIENTED_EDGE ( 'NONE', *, *, #14704, .T. ) ;
#22573 = VECTOR ( 'NONE', #6542, 1000.000000000000114 ) ;
#22574 = ORIENTED_EDGE ( 'NONE', *, *, #27628, .T. ) ;
#22575 = CARTESIAN_POINT ( 'NONE',  ( 50.91833842830035906, -4.387164033828486076, -1.383037143493254240 ) ) ;
#22576 = ORIENTED_EDGE ( 'NONE', *, *, #27010, .F. ) ;
#22577 = CIRCLE ( 'NONE', #24084, 0.1000000000000000472 ) ;
#22578 = CIRCLE ( 'NONE', #2852, 4.100000000000022737 ) ;
#22579 =( BOUNDED_SURFACE ( )  B_SPLINE_SURFACE ( 3, 2, ( 
 ( #8414, #13457, #6200 ),
 ( #25499, #18395, #28030 ),
 ( #22518, #9210, #13926 ),
 ( #21566, #4129, #11249 ),
 ( #4450, #11736, #28684 ),
 ( #18871, #1739, #8866 ),
 ( #16173, #6998, #20927 ),
 ( #14259, #1588, #7148 ),
 ( #9044, #13766, #21263 ),
 ( #31210, #23779, #11409 ),
 ( #2221, #11582, #6817 ),
 ( #28205, #30894, #30558 ),
 ( #16811, #23623, #19198 ),
 ( #6666, #16660, #28837 ),
 ( #26452, #23929, #26301 ),
 ( #11885, #4602, #9538 ) ),
 .UNSPECIFIED., .F., .F., .F. ) 
 B_SPLINE_SURFACE_WITH_KNOTS ( ( 4, 2, 2, 2, 2, 2, 2, 4 ),
 ( 3, 3 ),
 ( 0.001780502285214212487, 0.002558945925323800191, 0.002753556835351196955, 0.002948167745378593718, 0.003337389565433387679, 0.003726611385488181639, 0.004115833205542975166, 0.004894276845652563088 ),
 ( 0.000000000000000000, 1.000000000000000000 ),
 .UNSPECIFIED. ) 
 GEOMETRIC_REPRESENTATION_ITEM ( )  RATIONAL_B_SPLINE_SURFACE ( (
 ( 1.000000000000000000, 0.9418517008537223845, 1.000000000000000000),
 ( 1.000000000000000000, 0.9417987965885161739, 1.000000000000000000),
 ( 1.000000000000000000, 0.9418198861733920735, 1.000000000000000000),
 ( 1.000000000000000000, 0.9434060303845589468, 1.000000000000000000),
 ( 1.000000000000000000, 0.9437939819948110154, 1.000000000000000000),
 ( 1.000000000000000000, 0.9445989566712821306, 1.000000000000000000),
 ( 1.000000000000000000, 0.9450169930049815425, 1.000000000000000000),
 ( 1.000000000000000000, 0.9461610507673599013, 1.000000000000000000),
 ( 1.000000000000000000, 0.9467217966427268205, 1.000000000000000000),
 ( 1.000000000000000000, 0.9467345476124273684, 1.000000000000000000),
 ( 1.000000000000000000, 0.9461964028052485265, 1.000000000000000000),
 ( 1.000000000000000000, 0.9446801822474260035, 1.000000000000000000),
 ( 1.000000000000000000, 0.9437582546536592565, 1.000000000000000000),
 ( 1.000000000000000000, 0.9418129560295517289, 1.000000000000000000),
 ( 1.000000000000000000, 0.9418016889777567346, 1.000000000000000000),
 ( 1.000000000000000000, 0.9418517008537217183, 1.000000000000000000) ) ) 
 REPRESENTATION_ITEM ( '' )  SURFACE ( )  );
#22580 = VERTEX_POINT ( 'NONE', #23861 ) ;
#22581 = CARTESIAN_POINT ( 'NONE',  ( 30.98482657477733682, 7.184130536712149073, -2.050000000000107292 ) ) ;
#22582 = CIRCLE ( 'NONE', #8897, 2.000000000000000000 ) ;
#22583 = CARTESIAN_POINT ( 'NONE',  ( -57.42306624327022746, -3.399999999999988365, -0.9110272542660364792 ) ) ;
#22584 = DIRECTION ( 'NONE',  ( 1.000000000000000000, 0.000000000000000000, 0.000000000000000000 ) ) ;
#22585 = ADVANCED_FACE ( 'NONE', ( #9457 ), #19124, .F. ) ;
#22586 = DIRECTION ( 'NONE',  ( -0.7071067811865413555, 0.000000000000000000, 0.7071067811865536790 ) ) ;
#22587 = AXIS2_PLACEMENT_3D ( 'NONE', #6220, #20342, #18268 ) ;
#22588 = CARTESIAN_POINT ( 'NONE',  ( -57.83155989232412253, 3.925981830489463142, -1.911011283245466534E-13 ) ) ;
#22589 = FACE_OUTER_BOUND ( 'NONE', #24214, .T. ) ;
#22590 = AXIS2_PLACEMENT_3D ( 'NONE', #18171, #27812, #3727 ) ;
#22591 = CARTESIAN_POINT ( 'NONE',  ( 58.65000000000001990, 6.143261415694495821E-13, 3.111507638930570854E-58 ) ) ;
#22592 = DIRECTION ( 'NONE',  ( 0.000000000000000000, -0.9996898646859346815, -0.02490330187379791865 ) ) ;
#22593 = CIRCLE ( 'NONE', #8912, 2.000000000000000000 ) ;
#22594 = LINE ( 'NONE', #573, #31180 ) ;
#22595 = CARTESIAN_POINT ( 'NONE',  ( -60.58528264635175731, -2.531045389859400974, 0.9426176302699454945 ) ) ;
#22597 = ADVANCED_FACE ( 'NONE', ( #24324 ), #28545, .T. ) ;
#22596 = AXIS2_PLACEMENT_3D ( 'NONE', #17292, #26936, #5246 ) ;
#22598 = VECTOR ( 'NONE', #10701, 1000.000000000000000 ) ;
#22599 = CARTESIAN_POINT ( 'NONE',  ( -57.72499999999997300, 2.811319000628834039E-15, 1.036730182770210180E-16 ) ) ;
#22600 = DIRECTION ( 'NONE',  ( -1.000000000000000000, -0.000000000000000000, 3.491481338843133355E-15 ) ) ;
#22601 = CIRCLE ( 'NONE', #8927, 2.525000000001609290 ) ;
#22602 = DIRECTION ( 'NONE',  ( 0.000000000000000000, 1.000000000000000000, 0.000000000000000000 ) ) ;
#22603 = VECTOR ( 'NONE', #28343, 1000.000000000000000 ) ;
#22604 = EDGE_LOOP ( 'NONE', ( #21424, #19912, #12383, #24913 ) ) ;
#22605 = CARTESIAN_POINT ( 'NONE',  ( 51.22715433738867574, -0.9941391646896066137, -1.410349289489640556 ) ) ;
#22606 = CARTESIAN_POINT ( 'NONE',  ( 54.40859248998804532, 6.718200026737121355, 1.988253682540942258 ) ) ;
#22607 = ORIENTED_EDGE ( 'NONE', *, *, #1113, .F. ) ;
#22608 = EDGE_CURVE ( 'NONE', #19129, #19672, #11178, .T. ) ;
#22609 = CARTESIAN_POINT ( 'NONE',  ( 69.20000000000001705, 0.7500000000000000000, -1.988246715074081017 ) ) ;
#22610 = ORIENTED_EDGE ( 'NONE', *, *, #5588, .T. ) ;
#22611 = ADVANCED_FACE ( 'NONE', ( #29229 ), #27019, .T. ) ;
#22612 = B_SPLINE_CURVE_WITH_KNOTS ( 'NONE', 3,
 ( #2547, #29287, #29128, #24235, #29427, #4908, #307, #31201, #9529, #19190 ),
 .UNSPECIFIED., .F., .F.,
 ( 4, 2, 2, 2, 4 ),
 ( 0.000000000000000000, 0.0003520942986628438666, 0.0007041885973256877332, 0.001056282895988531600, 0.001408377194651375466 ),
 .UNSPECIFIED. ) ;
#22613 = DIRECTION ( 'NONE',  ( -1.000000000000000000, 0.000000000000000000, 0.000000000000000000 ) ) ;
#22614 = CARTESIAN_POINT ( 'NONE',  ( -59.19999999999997442, -3.382957286162487698, 0.3399999999999019362 ) ) ;
#22616 = CARTESIAN_POINT ( 'NONE',  ( 51.31572262954152563, 1.002608958138273554, -1.996089927833914146 ) ) ;
#22615 = CARTESIAN_POINT ( 'NONE',  ( 58.65000000000001279, 0.8495817349399592544, 1.671477153794648673 ) ) ;
#22617 = VECTOR ( 'NONE', #28989, 1000.000000000000000 ) ;
#22618 = ADVANCED_FACE ( 'NONE', ( #25082 ), #9345, .T. ) ;
#22619 = ORIENTED_EDGE ( 'NONE', *, *, #30372, .T. ) ;
#22620 = CARTESIAN_POINT ( 'NONE',  ( 61.25000000000003553, -0.8825412585404734944, -1.623100356595552407 ) ) ;
#22621 = CIRCLE ( 'NONE', #30190, 3.500000000000000444 ) ;
#22622 = CARTESIAN_POINT ( 'NONE',  ( 58.65000000000001990, 6.143261415694495821E-13, 3.111507638930570854E-58 ) ) ;
#22623 = AXIS2_PLACEMENT_3D ( 'NONE', #16166, #25814, #14092 ) ;
#22624 = ORIENTED_EDGE ( 'NONE', *, *, #4116, .F. ) ;
#22626 = CARTESIAN_POINT ( 'NONE',  ( -59.29999999999997584, 0.7533615035078071731, -3.673546848079177529 ) ) ;
#22625 = CARTESIAN_POINT ( 'NONE',  ( 52.20711756518983293, 0.5000000000005468959, -1.996089927833914146 ) ) ;
#22627 = LINE ( 'NONE', #12626, #11493 ) ;
#22628 = EDGE_LOOP ( 'NONE', ( #9464, #11515, #27221, #13050, #24237, #13942, #1441, #20810, #29151, #14780, #13595, #20360, #10438, #4430, #13780, #29677, #28091, #10279 ) ) ;
#22629 = CARTESIAN_POINT ( 'NONE',  ( 51.12687253673781385, -0.9194130538815391551, 1.491219977510798600 ) ) ;
#22630 = CARTESIAN_POINT ( 'NONE',  ( -59.29999999999997584, 2.330309927981285032E-15, 4.253626757584724400E-16 ) ) ;
#22631 = DIRECTION ( 'NONE',  ( -3.491481338843133355E-15, -3.491481338843133355E-15, 1.000000000000000000 ) ) ;
#22632 = CLOSED_SHELL ( 'NONE', ( #12426, #6787, #28011, #14434, #23758, #4547, #29954, #20763, #28779, #5357 ) ) ;
#22633 = AXIS2_PLACEMENT_3D ( 'NONE', #6653, #6334, #4438 ) ;
#22634 = CARTESIAN_POINT ( 'NONE',  ( 61.25000000000003553, -0.9999999999993586242, 1.863080903344643380 ) ) ;
#22635 = CYLINDRICAL_SURFACE ( 'NONE', #26834, 0.2500000000000000000 ) ;
#22636 = AXIS2_PLACEMENT_3D ( 'NONE', #3437, #30329, #13075 ) ;
#22637 = CIRCLE ( 'NONE', #1861, 3.625000000000000444 ) ;
#22638 = CARTESIAN_POINT ( 'NONE',  ( 51.59739104186229497, -1.010292945602099701, 1.272765950230261733 ) ) ;
#22639 = ORIENTED_EDGE ( 'NONE', *, *, #3944, .F. ) ;
#22640 = CARTESIAN_POINT ( 'NONE',  ( 15.98305126557428224, 2.728070298465770982, 4.669343935538297963 ) ) ;
#22641 = AXIS2_PLACEMENT_3D ( 'NONE', #13095, #23084, #3460 ) ;
#22642 = EDGE_CURVE ( 'NONE', #5992, #9864, #2314, .T. ) ;
#22643 = CIRCLE ( 'NONE', #8967, 1.000000000000000000 ) ;
#22644 = ADVANCED_FACE ( 'NONE', ( #10366 ), #14172, .T. ) ;
#22645 = CARTESIAN_POINT ( 'NONE',  ( -54.52560264074444518, -0.4085193297958337744, -3.447427373925056493 ) ) ;
#22646 = AXIS2_PLACEMENT_3D ( 'NONE', #27989, #28151, #6774 ) ;
#22648 = ADVANCED_FACE ( 'NONE', ( #24924 ), #6194, .T. ) ;
#22647 = CARTESIAN_POINT ( 'NONE',  ( -58.45655989232413674, 1.962990915244716694, 3.399999999999802736 ) ) ;
#22649 = CARTESIAN_POINT ( 'NONE',  ( -58.63452994616204705, 3.117691453623969711, 1.799999999999821299 ) ) ;
#22650 = CARTESIAN_POINT ( 'NONE',  ( 65.04999999999996874, 4.959819536545755081E-16, -4.050000000000682832 ) ) ;
#22651 = CARTESIAN_POINT ( 'NONE',  ( 48.43920370478603843, 1.278211010209494347, -3.870212229389975889 ) ) ;
#22652 = EDGE_LOOP ( 'NONE', ( #20724, #28 ) ) ;
#22653 = CIRCLE ( 'NONE', #30201, 1.000000000000000000 ) ;
#22654 = DIRECTION ( 'NONE',  ( 3.002035892788117459E-16, -0.9996898646859343485, -0.02490330187381124133 ) ) ;
#22655 = VECTOR ( 'NONE', #26517, 1000.000000000000000 ) ;
#22656 = EDGE_LOOP ( 'NONE', ( #16485, #11864, #12794, #11674, #14313, #5523, #250 ) ) ;
#22657 = DIRECTION ( 'NONE',  ( 1.000000000000000000, 1.047444401652940007E-14, 0.000000000000000000 ) ) ;
#22659 = CARTESIAN_POINT ( 'NONE',  ( 58.65000038048067665, -1.265626441015677450, 1.383507098106847799 ) ) ;
#22658 = CARTESIAN_POINT ( 'NONE',  ( -54.49999999999996447, -1.993349740317589935, -2.907263629733159327 ) ) ;
#22660 = ORIENTED_EDGE ( 'NONE', *, *, #12285, .T. ) ;
#22661 = ORIENTED_EDGE ( 'NONE', *, *, #9899, .T. ) ;
#22662 = CARTESIAN_POINT ( 'NONE',  ( -59.15835481156722864, -0.7533615035078041755, 3.673546848079178861 ) ) ;
#22663 = EDGE_LOOP ( 'NONE', ( #17140, #16015, #17502, #23408 ) ) ;
#22665 = DIRECTION ( 'NONE',  ( 1.000000000000000000, -1.219044193948983948E-29, 3.491481338843133355E-15 ) ) ;
#22664 = CARTESIAN_POINT ( 'NONE',  ( -58.19702994616203284, -2.078460969082631227, -3.600000000000212363 ) ) ;
#22666 = CARTESIAN_POINT ( 'NONE',  ( -58.36042740578360366, -2.936324665650201116, -2.606018187048497747 ) ) ;
#22667 = AXIS2_PLACEMENT_3D ( 'NONE', #20499, #15735, #28063 ) ;
#22668 = CARTESIAN_POINT ( 'NONE',  ( 51.90000000000001279, 1.029992063861229212E-15, -4.375000000000002665 ) ) ;
#22669 = PRODUCT_CONTEXT ( 'NONE', #12352, 'mechanical' ) ;
#22670 = CIRCLE ( 'NONE', #7487, 2.874999999999999112 ) ;
#22671 = CARTESIAN_POINT ( 'NONE',  ( 58.66122797211845352, -1.314214529126519704, -1.337438849764270632 ) ) ;
#22672 = CIRCLE ( 'NONE', #27688, 1.000000000000000000 ) ;
#22673 = ORIENTED_EDGE ( 'NONE', *, *, #13771, .F. ) ;
#22674 = DIRECTION ( 'NONE',  ( 7.637891338979824674E-45, -1.000000000000000000, -3.491481338843135327E-15 ) ) ;
#22675 = CARTESIAN_POINT ( 'NONE',  ( 52.91918222397608673, 8.304852724747799897, -1.919164453910518375 ) ) ;
#22676 = CARTESIAN_POINT ( 'NONE',  ( 48.46709009337374141, -1.365599538210734876, -3.854893000251051749 ) ) ;
#22677 = CARTESIAN_POINT ( 'NONE',  ( 15.03925126672132961, 1.123735532908287427, 5.289358697221544503 ) ) ;
#22678 = EDGE_CURVE ( 'NONE', #10038, #12845, #17426, .T. ) ;
#22679 = EDGE_CURVE ( 'NONE', #2190, #25428, #10863, .T. ) ;
#22680 = DIRECTION ( 'NONE',  ( 1.000000000000000000, -0.000000000000000000, -1.047444401652940007E-14 ) ) ;
#22683 = ADVANCED_FACE ( 'NONE', ( #18609 ), #13203, .F. ) ;
#22682 = CARTESIAN_POINT ( 'NONE',  ( 58.75000000694010538, -1.856761646087839113, -0.5233439189817360448 ) ) ;
#22681 = DIRECTION ( 'NONE',  ( 1.000000000000000000, 1.047444401652940007E-14, 0.000000000000000000 ) ) ;
#22684 = AXIS2_PLACEMENT_3D ( 'NONE', #20335, #30107, #13477 ) ;
#22685 = CARTESIAN_POINT ( 'NONE',  ( 51.70000000000003837, 2.428612866367529932E-14, 4.099999999999812239 ) ) ;
#22686 = CARTESIAN_POINT ( 'NONE',  ( -62.06710100716625789, -2.694091267595633887, 0.1949429447076614641 ) ) ;
#22688 = CARTESIAN_POINT ( 'NONE',  ( -62.09999999999997300, -2.712886303669590049, -0.3394508044491614807 ) ) ;
#22687 = CARTESIAN_POINT ( 'NONE',  ( 58.64999999999999858, 1.834410884276644227, -0.3880228184651523526 ) ) ;
#22689 = EDGE_LOOP ( 'NONE', ( #30965, #15512, #13463, #26048 ) ) ;
#22690 = DIRECTION ( 'NONE',  ( 0.000000000000000000, 0.9996898646859344595, 0.02490330187381124133 ) ) ;
#22691 = DIRECTION ( 'NONE',  ( 0.000000000000000000, -0.8914544820234928668, -0.4531102586349443628 ) ) ;
#22693 = CARTESIAN_POINT ( 'NONE',  ( -59.59999999999997300, -2.337126060168364994, -1.249136413240117038 ) ) ;
#22692 = CARTESIAN_POINT ( 'NONE',  ( 15.41586008885047576, 2.840672495176553625, -4.363684107482565189 ) ) ;
#22694 = CARTESIAN_POINT ( 'NONE',  ( 51.25000000000000711, 1.487500000000536504, 3.111507638930570854E-58 ) ) ;
#22695 = ORIENTED_EDGE ( 'NONE', *, *, #3100, .F. ) ;
#22696 = CARTESIAN_POINT ( 'NONE',  ( 54.21471704787897750, 5.862036637490150248, 2.049999999999810640 ) ) ;
#22697 = CARTESIAN_POINT ( 'NONE',  ( -60.59999999999997300, -2.426837276046140079, -1.064406330116907329 ) ) ;
#22698 = EDGE_CURVE ( 'NONE', #12308, #12582, #6247, .T. ) ;
#22699 = ORIENTED_EDGE ( 'NONE', *, *, #26897, .F. ) ;
#22700 = APPLICATION_CONTEXT ( 'automotive_design' ) ;
#22701 = DIRECTION ( 'NONE',  ( 0.000000000000000000, 1.000000000000000000, 3.491481338843131383E-15 ) ) ;
#22702 = EDGE_LOOP ( 'NONE', ( #26064, #774, #25618, #18113 ) ) ;
#22703 = CARTESIAN_POINT ( 'NONE',  ( -73.89999999999997726, -0.4498604391086729049, -0.01120648584321003519 ) ) ;
#22704 = CARTESIAN_POINT ( 'NONE',  ( -59.69999999999997442, 8.366749974758454467E-15, -2.120534355533670266E-13 ) ) ;
#22705 = ORIENTED_EDGE ( 'NONE', *, *, #7003, .F. ) ;
#22706 = DIRECTION ( 'NONE',  ( 1.000000000000000000, 0.000000000000000000, 0.000000000000000000 ) ) ;
#22707 = CARTESIAN_POINT ( 'NONE',  ( -54.70655989232413674, 1.962990915244722245, 3.399999999999812950 ) ) ;
#22708 = VERTEX_POINT ( 'NONE', #16222 ) ;
#22709 = CARTESIAN_POINT ( 'NONE',  ( 56.97512559646294505, 0.7466375667864569854, -1.747149777169433094 ) ) ;
#22710 = CYLINDRICAL_SURFACE ( 'NONE', #27351, 0.1000000000000000472 ) ;
#22711 = CARTESIAN_POINT ( 'NONE',  ( 21.97322666366011035, 8.076925076899389211, 1.949999999999923128 ) ) ;
#22712 = ORIENTED_EDGE ( 'NONE', *, *, #23414, .F. ) ;
#22713 =( GEOMETRIC_REPRESENTATION_CONTEXT ( 3 ) GLOBAL_UNCERTAINTY_ASSIGNED_CONTEXT ( ( #16807 ) ) GLOBAL_UNIT_ASSIGNED_CONTEXT ( ( #12517, #12351, #7308 ) ) REPRESENTATION_CONTEXT ( 'NONE', 'WORKASPACE' ) );
#22714 = CIRCLE ( 'NONE', #1459, 3.598079936076698182 ) ;
#22715 = CARTESIAN_POINT ( 'NONE',  ( -58.74999999999997158, 2.944486372867092250, 1.699999999999803002 ) ) ;
#22716 = CARTESIAN_POINT ( 'NONE',  ( 48.40000000000001990, -4.899999999999999467, -4.100000000000022737 ) ) ;
#22717 = CARTESIAN_POINT ( 'NONE',  ( 46.90000000000001279, 1.734723475976807094E-15, -4.375000000000000000 ) ) ;
#22718 = DIRECTION ( 'NONE',  ( 0.000000000000000000, -0.9996898646859344595, -0.02490330187381124133 ) ) ;
#22719 = CARTESIAN_POINT ( 'NONE',  ( 61.25000000000004263, -2.008165151418606520, 0.5380862305909606125 ) ) ;
#22720 = EDGE_CURVE ( 'NONE', #15281, #826, #24029, .T. ) ;
#22722 = DIRECTION ( 'NONE',  ( 1.000000000000000000, 0.000000000000000000, -3.491481338843133355E-15 ) ) ;
#22721 = DIRECTION ( 'NONE',  ( 1.000000000000000000, -1.165806029810671835E-15, -1.108125256279701864E-14 ) ) ;
#22723 = DIRECTION ( 'NONE',  ( 0.000000000000000000, 0.000000000000000000, 1.000000000000000000 ) ) ;
#22724 = CARTESIAN_POINT ( 'NONE',  ( -59.69142724121850563, 2.412383461849218591, -1.233589124872089826 ) ) ;
#22725 = DIRECTION ( 'NONE',  ( -9.329605248950888974E-15, 1.000000000000000000, 0.000000000000000000 ) ) ;
#22726 = CARTESIAN_POINT ( 'NONE',  ( -54.45495050826418293, 1.499999999999999556, -3.300094695611021312 ) ) ;
#22727 = CARTESIAN_POINT ( 'NONE',  ( 53.25930982050607554, 8.220062413181228322, -2.050000000000184563 ) ) ;
#22728 = ORIENTED_EDGE ( 'NONE', *, *, #9373, .T. ) ;
#22729 = DIRECTION ( 'NONE',  ( 1.000000000000000000, 3.053848253006669023E-16, -2.042510438544995415E-16 ) ) ;
#22730 = AXIS2_PLACEMENT_3D ( 'NONE', #3518, #5892, #8865 ) ;
#22731 = EDGE_CURVE ( 'NONE', #11180, #5002, #2285, .T. ) ;
#22732 = ORIENTED_EDGE ( 'NONE', *, *, #23940, .T. ) ;
#22733 = CYLINDRICAL_SURFACE ( 'NONE', #17948, 2.625000000001612044 ) ;
#22734 = PRODUCT_DEFINITION_SHAPE ( 'NONE', 'NONE',  #31333 ) ;
#22735 = CARTESIAN_POINT ( 'NONE',  ( -58.48542740578359656, -3.725040285533365303, 1.239922660687675648 ) ) ;
#22737 = CARTESIAN_POINT ( 'NONE',  ( 47.73715617352264218, -4.312058781922654127, 1.282041952413738306 ) ) ;
#22736 = CARTESIAN_POINT ( 'NONE',  ( -56.12499999999996447, -2.944486372867076707, -1.700000000000210010 ) ) ;
#22738 = VERTEX_POINT ( 'NONE', #29992 ) ;
#22739 = VERTEX_POINT ( 'NONE', #13345 ) ;
#22740 = CARTESIAN_POINT ( 'NONE',  ( 53.82818350034567345, 5.794550817852396563, -1.819853284099130608 ) ) ;
#22741 = ORIENTED_EDGE ( 'NONE', *, *, #21553, .F. ) ;
#22742 = DIRECTION ( 'NONE',  ( 1.000000000000000000, -0.000000000000000000, -0.000000000000000000 ) ) ;
#22743 = ORIENTED_EDGE ( 'NONE', *, *, #6112, .F. ) ;
#22744 = CARTESIAN_POINT ( 'NONE',  ( 22.09542497196754951, 7.445411295443247646, -1.950000000000144285 ) ) ;
#22745 = CARTESIAN_POINT ( 'NONE',  ( 50.80000000000001847, -4.003661535119149129, -1.169131321892095565 ) ) ;
#22746 = CARTESIAN_POINT ( 'NONE',  ( -59.15400635094606940, -3.399999999999988365, -0.9110272542660506900 ) ) ;
#22747 = AXIS2_PLACEMENT_3D ( 'NONE', #19663, #17272, #2110 ) ;
#22748 = CARTESIAN_POINT ( 'NONE',  ( 33.47623932017462778, -4.018128179617539431, 3.618665901676652918 ) ) ;
#22749 = CARTESIAN_POINT ( 'NONE',  ( -58.70655989232410832, 1.962990915244748891, -3.400000000000199751 ) ) ;
#22750 = CARTESIAN_POINT ( 'NONE',  ( 47.86807216729960146, -3.937842570012147103, 1.145831914963004960 ) ) ;
#22751 = PRODUCT_DEFINITION_FORMATION_WITH_SPECIFIED_SOURCE ( 'ANY', '', #7773, .NOT_KNOWN. ) ;
#22752 = CARTESIAN_POINT ( 'NONE',  ( -54.54999999999998295, 0.9743475445367651977, -4.751120590182403625 ) ) ;
#22753 = VECTOR ( 'NONE', #10572, 1000.000000000000000 ) ;
#22754 = EDGE_CURVE ( 'NONE', #2983, #333, #10371, .T. ) ;
#22755 = DIRECTION ( 'NONE',  ( 1.000000000000000000, 3.054025858079668409E-16, -2.042474015755241579E-16 ) ) ;
#22756 = CIRCLE ( 'NONE', #30834, 0.2500000000000000000 ) ;
#22757 = DIRECTION ( 'NONE',  ( 0.000000000000000000, 1.224646799147358384E-16, 1.000000000000000000 ) ) ;
#22759 = CARTESIAN_POINT ( 'NONE',  ( 51.06473033323084820, -4.311876499822710151, 1.282612398563742095 ) ) ;
#22758 = CARTESIAN_POINT ( 'NONE',  ( -61.40479058095097287, -2.604980992110456306, 0.7099817115554608593 ) ) ;
#22760 = VECTOR ( 'NONE', #11148, 1000.000000000000000 ) ;
#22761 = CARTESIAN_POINT ( 'NONE',  ( 63.50000000000000000, -0.8382352941176473005, -2.222158093317947003 ) ) ;
#22762 = CARTESIAN_POINT ( 'NONE',  ( 50.59602332238209499, -0.1408342061598474859, 0.8215393206232036727 ) ) ;
#22763 = CARTESIAN_POINT ( 'NONE',  ( -36.00201293083839005, 1.123735532908824331, 5.289358697221505423 ) ) ;
#22764 = ORIENTED_EDGE ( 'NONE', *, *, #17320, .F. ) ;
#22765 = B_SPLINE_CURVE_WITH_KNOTS ( 'NONE', 3,
 ( #1302, #30115, #22867, #24902, #5921, #7984, #17804, #3222, #6078, #11124, #13181, #22546, #1155, #850, #17947, #1464 ),
 .UNSPECIFIED., .F., .F.,
 ( 4, 3, 3, 3, 3, 4 ),
 ( 0.000000000000000000, 3.111139534546023401E-05, 6.583698738123831937E-05, 9.811465807641186142E-05, 0.0001294159172546408877, 0.0001609582457662007114 ),
 .UNSPECIFIED. ) ;
#22766 = CARTESIAN_POINT ( 'NONE',  ( 50.55260020142763722, 0.05166409867394209515, 0.7900938592415983619 ) ) ;
#22767 = CARTESIAN_POINT ( 'NONE',  ( 54.27127970009382096, 6.003218211144689676, 2.049999999999811084 ) ) ;
#22768 = ORIENTED_EDGE ( 'NONE', *, *, #25943, .T. ) ;
#22769 = ADVANCED_FACE ( 'NONE', ( #4171 ), #13376, .F. ) ;
#22770 = DIRECTION ( 'NONE',  ( 0.000000000000000000, 0.000000000000000000, 1.000000000000000000 ) ) ;
#22771 =( BOUNDED_CURVE ( )  B_SPLINE_CURVE ( 2, ( #20435, #6024, #22337, #10752, #8374, #27061, #15198, #5379, #29913 ),
 .UNSPECIFIED., .F., .T. ) 
 B_SPLINE_CURVE_WITH_KNOTS ( ( 3, 2, 2, 2, 3 ),
 ( 0.6944444444444445308, 0.7037037037037037202, 0.7222222222222222099, 0.7407407407407406996, 0.7434165071384308821 ),
 .UNSPECIFIED. ) 
 CURVE ( )  GEOMETRIC_REPRESENTATION_ITEM ( )  RATIONAL_B_SPLINE_CURVE ( ( 0.9330127018922194093, 0.9330127018922197424, 1.000000000000000000, 0.8660254037844387076, 1.000000000000000000, 0.8660254037844387076, 1.000000000000000000, 0.9806418249743238391, 0.9668778290081130322 ) ) 
 REPRESENTATION_ITEM ( '' )  );
#22772 = ORIENTED_EDGE ( 'NONE', *, *, #11720, .F. ) ;
#22773 = DIRECTION ( 'NONE',  ( 0.000000000000000000, 0.000000000000000000, 1.000000000000000000 ) ) ;
#22774 = CARTESIAN_POINT ( 'NONE',  ( -54.40835481156724285, -3.238593381231841928, -2.874284765127022911 ) ) ;
#22776 = LINE ( 'NONE', #23075, #15668 ) ;
#22775 = PLANE ( 'NONE',  #13999 ) ;
#22777 = VERTEX_POINT ( 'NONE', #18444 ) ;
#22778 = CARTESIAN_POINT ( 'NONE',  ( 61.25000000000003553, -0.9999999999993586242, -1.586072192556190030 ) ) ;
#22779 = CIRCLE ( 'NONE', #28321, 0.04999999999999988481 ) ;
#22780 = CARTESIAN_POINT ( 'NONE',  ( 59.00000000000004974, 3.520859547548639454E-16, 2.874999999999380940 ) ) ;
#22781 = VERTEX_POINT ( 'NONE', #16065 ) ;
#22783 = CARTESIAN_POINT ( 'NONE',  ( 58.45000000000001705, 0.8000000000000000444, -1.778341924377873751 ) ) ;
#22782 = CARTESIAN_POINT ( 'NONE',  ( 51.80000000000002558, 6.475000000000061817, 2.049999999999819522 ) ) ;
#22784 = CARTESIAN_POINT ( 'NONE',  ( 47.10000000000002274, 2.260045634542508431E-14, 1.100000000000006084 ) ) ;
#22785 = ORIENTED_EDGE ( 'NONE', *, *, #15081, .F. ) ;
#22786 = DIRECTION ( 'NONE',  ( -1.000000000000000000, -0.000000000000000000, 3.491481338843133355E-15 ) ) ;
#22787 = CIRCLE ( 'NONE', #13143, 0.09999999999999982514 ) ;
#22788 = CARTESIAN_POINT ( 'NONE',  ( -36.92443669619682112, 5.191204783933211608, -1.522159526382838246 ) ) ;
#22789 = ADVANCED_FACE ( 'NONE', ( #8615 ), #23494, .F. ) ;
#22790 = CARTESIAN_POINT ( 'NONE',  ( -61.34999999999997300, 1.397055221233662433E-15, 2.044538471210920981E-15 ) ) ;
#22791 = AXIS2_PLACEMENT_3D ( 'NONE', #26717, #255, #2947 ) ;
#22792 = CARTESIAN_POINT ( 'NONE',  ( -54.49999999999997868, -1.549999999999999600, -3.332135201338624952 ) ) ;
#22793 = DIRECTION ( 'NONE',  ( 1.857384214413941805E-31, -5.942513678379226626E-16, -1.000000000000000000 ) ) ;
#22794 = DIRECTION ( 'NONE',  ( -0.000000000000000000, 0.000000000000000000, 1.000000000000000000 ) ) ;
#22795 = ORIENTED_EDGE ( 'NONE', *, *, #7255, .F. ) ;
#22796 = EDGE_CURVE ( 'NONE', #30383, #10286, #4023, .T. ) ;
#22797 = CARTESIAN_POINT ( 'NONE',  ( 15.41586008885047221, -2.840672495176578938, 4.363684107482475483 ) ) ;
#22798 = EDGE_CURVE ( 'NONE', #20928, #2824, #18479, .T. ) ;
#22799 = EDGE_CURVE ( 'NONE', #20905, #27818, #8841, .T. ) ;
#22800 = DIRECTION ( 'NONE',  ( 0.000000000000000000, -1.000000000000000000, 5.942513678379226626E-16 ) ) ;
#22801 = CARTESIAN_POINT ( 'NONE',  ( 51.25000000000002842, -0.9938153758920951208, -1.589954715908409977 ) ) ;
#22802 = DIRECTION ( 'NONE',  ( 1.000000000000000000, 0.000000000000000000, 0.000000000000000000 ) ) ;
#22803 = CARTESIAN_POINT ( 'NONE',  ( -58.69702994616204705, 4.156921938165313968, -1.807992169193672380E-13 ) ) ;
#22805 = AXIS2_PLACEMENT_3D ( 'NONE', #12316, #31183, #17249 ) ;
#22804 = CARTESIAN_POINT ( 'NONE',  ( 58.65266784251146959, -1.873893454697892036, -0.06654060276246864802 ) ) ;
#22806 = CARTESIAN_POINT ( 'NONE',  ( 29.92080114924054968, 6.605317672619497316, 2.049999999999895461 ) ) ;
#22807 = VERTEX_POINT ( 'NONE', #1331 ) ;
#22808 = DIRECTION ( 'NONE',  ( 0.000000000000000000, 0.9996898646859344595, 0.02490330187381119623 ) ) ;
#22809 = ORIENTED_EDGE ( 'NONE', *, *, #19499, .T. ) ;
#22810 = CARTESIAN_POINT ( 'NONE',  ( 50.25000000000000000, 1.895722432252826328, 0.6373668173479852816 ) ) ;
#22812 = CARTESIAN_POINT ( 'NONE',  ( -54.39999999999999147, 1.557046979865768677, 3.273565289174698911 ) ) ;
#22811 = CARTESIAN_POINT ( 'NONE',  ( 48.30261087823118515, 0.9335627837658418970, 3.994936164801341061 ) ) ;
#22813 = ORIENTED_EDGE ( 'NONE', *, *, #6582, .F. ) ;
#22814 = EDGE_LOOP ( 'NONE', ( #22886, #20510, #24176, #101 ) ) ;
#22815 = DIRECTION ( 'NONE',  ( 0.000000000000000000, 0.000000000000000000, -1.000000000000000000 ) ) ;
#22816 = DIRECTION ( 'NONE',  ( 0.000000000000000000, 0.000000000000000000, -1.000000000000000000 ) ) ;
#22817 = ORIENTED_EDGE ( 'NONE', *, *, #22145, .F. ) ;
#22819 = CARTESIAN_POINT ( 'NONE',  ( 58.65000038048047060, 1.008797009996078353, 1.580579251836430332 ) ) ;
#22818 = CARTESIAN_POINT ( 'NONE',  ( -59.88452994616203995, -3.117691453623976816, 1.799999999999775335 ) ) ;
#22820 = CARTESIAN_POINT ( 'NONE',  ( -58.42292740578360366, -3.330682475591783653, -0.6830477631804107164 ) ) ;
#22821 = ADVANCED_FACE ( 'NONE', ( #11000 ), #20680, .T. ) ;
#22822 = DIRECTION ( 'NONE',  ( 2.117927888850091331E-16, -0.02490330187381135929, 0.9996898646859343485 ) ) ;
#22823 =( LENGTH_UNIT ( ) NAMED_UNIT ( * ) SI_UNIT ( .MILLI., .METRE. ) );
#22824 = CARTESIAN_POINT ( 'NONE',  ( -59.37030229529103309, 2.324290318287153490, 1.279035047872993269 ) ) ;
#22825 = EDGE_CURVE ( 'NONE', #28370, #12339, #30782, .T. ) ;
#22826 = AXIS2_PLACEMENT_3D ( 'NONE', #3639, #27392, #29922 ) ;
#22827 = ORIENTED_EDGE ( 'NONE', *, *, #18373, .T. ) ;
#22828 = DIRECTION ( 'NONE',  ( -1.000000000000000000, -3.053848253006669023E-16, 2.042510438544995415E-16 ) ) ;
#22829 = CARTESIAN_POINT ( 'NONE',  ( 54.16188382698977222, 6.950389949135505674, -2.050000000000188560 ) ) ;
#22830 = CARTESIAN_POINT ( 'NONE',  ( 48.40000000000002700, -0.6462379109120522935, -4.048750000000028493 ) ) ;
#22831 = CARTESIAN_POINT ( 'NONE',  ( 15.17256654081409373, 0.4576450652446744649, 5.200000002521306008 ) ) ;
#22832 = EDGE_CURVE ( 'NONE', #17785, #11045, #13462, .T. ) ;
#22833 = CARTESIAN_POINT ( 'NONE',  ( 51.80000000000001137, 4.350000000000017408, -2.050000000000180123 ) ) ;
#22834 = CARTESIAN_POINT ( 'NONE',  ( -35.85663232820601820, 1.123735532908269441, -5.289358697221545391 ) ) ;
#22835 = LINE ( 'NONE', #18666, #1855 ) ;
#22836 = DIRECTION ( 'NONE',  ( 3.491481338843133355E-15, -0.000000000000000000, 1.000000000000000000 ) ) ;
#22838 = DIRECTION ( 'NONE',  ( -1.000000000000000000, 1.219044193948983948E-29, -3.491481338843133355E-15 ) ) ;
#22837 = DIRECTION ( 'NONE',  ( -1.000000000000000000, -2.586136946169074517E-16, 0.000000000000000000 ) ) ;
#22839 = ORIENTED_EDGE ( 'NONE', *, *, #11479, .T. ) ;
#22840 = FACE_OUTER_BOUND ( 'NONE', #465, .T. ) ;
#22841 = DIRECTION ( 'NONE',  ( 0.000000000000000000, -1.000000000000000000, 8.673617379884030739E-15 ) ) ;
#22843 = DIRECTION ( 'NONE',  ( 1.000000000000000000, 1.047444401652940007E-14, 0.000000000000000000 ) ) ;
#22842 = CARTESIAN_POINT ( 'NONE',  ( 15.86395258069111769, 3.736273719777285507, -3.909490113446701720 ) ) ;
#22844 = CARTESIAN_POINT ( 'NONE',  ( 57.05000000000001137, 0.8156862745098039102, 2.468735688885371982 ) ) ;
#22845 = VERTEX_POINT ( 'NONE', #16858 ) ;
#22846 = CARTESIAN_POINT ( 'NONE',  ( 53.93792434297150606, 7.473468098462469733, 2.049999999999811973 ) ) ;
#22847 = CARTESIAN_POINT ( 'NONE',  ( -60.61073679674431958, -2.452477434632136077, -1.083948463035139476 ) ) ;
#22848 = VERTEX_POINT ( 'NONE', #6710 ) ;
#22849 = CARTESIAN_POINT ( 'NONE',  ( 21.97286177946902797, 8.089633431579400735, -1.950000000000075895 ) ) ;
#22850 = ORIENTED_EDGE ( 'NONE', *, *, #25501, .T. ) ;
#22851 = EDGE_CURVE ( 'NONE', #19841, #27197, #21781, .T. ) ;
#22852 = CARTESIAN_POINT ( 'NONE',  ( 16.10660252424456829, 2.945786441214607532, -4.543674732827721385 ) ) ;
#22853 = DIRECTION ( 'NONE',  ( 0.000000000000000000, 1.000000000000000000, 3.491481338843130594E-15 ) ) ;
#22854 = ORIENTED_EDGE ( 'NONE', *, *, #3320, .F. ) ;
#22855 = EDGE_CURVE ( 'NONE', #3662, #22512, #26552, .T. ) ;
#22856 = CARTESIAN_POINT ( 'NONE',  ( 50.35762544161294585, 8.151359338959888845, -1.950000000000174927 ) ) ;
#22857 = CIRCLE ( 'NONE', #4641, 0.2500000000000002220 ) ;
#22858 = CARTESIAN_POINT ( 'NONE',  ( -56.14405989232413674, -3.920666489018339623E-15, 3.399999999999799627 ) ) ;
#22859 = VERTEX_POINT ( 'NONE', #11779 ) ;
#22860 = CARTESIAN_POINT ( 'NONE',  ( 57.02478278053006022, 0.7769964508979760875, -1.733862565638740305 ) ) ;
#22861 = ADVANCED_FACE ( 'NONE', ( #7043 ), #26347, .T. ) ;
#22862 = VERTEX_POINT ( 'NONE', #4968 ) ;
#22863 = TOROIDAL_SURFACE ( 'NONE', #29390, 1.302039949377232331, 0.05000000000000000278 ) ;
#22864 = CARTESIAN_POINT ( 'NONE',  ( -57.24999999999997158, 2.944486372867092250, 1.699999999999808109 ) ) ;
#22865 = CARTESIAN_POINT ( 'NONE',  ( 60.99999998418542901, 0.8156891353822055546, 1.406736638527498195 ) ) ;
#22866 = CARTESIAN_POINT ( 'NONE',  ( 60.75000000000001421, 0.5000000000006363798, -1.863080903343375061 ) ) ;
#22867 = CARTESIAN_POINT ( 'NONE',  ( 56.95150694030147775, -0.7014737422875408912, -1.765795469766037185 ) ) ;
#22868 = CARTESIAN_POINT ( 'NONE',  ( -54.49999999999996447, 1.400000000000023670, -3.959797974644871044 ) ) ;
#22869 = ADVANCED_FACE ( 'NONE', ( #16705 ), #13670, .T. ) ;
#22870 = CARTESIAN_POINT ( 'NONE',  ( 50.80657076746749112, 8.706740374280103723, 1.949999999999822764 ) ) ;
#22871 = DIRECTION ( 'NONE',  ( 2.614381936396368743E-16, -0.2008964009354147762, 0.9796124928211139560 ) ) ;
#22872 = DIRECTION ( 'NONE',  ( 1.000000000000000000, -1.219044193948983948E-29, 3.491481338843133355E-15 ) ) ;
#22873 = CARTESIAN_POINT ( 'NONE',  ( -54.44999999999997442, 1.499999999999999556, -3.300094695611021312 ) ) ;
#22874 = CARTESIAN_POINT ( 'NONE',  ( 51.80000000000001137, 6.475000000000062705, -2.050000000000180123 ) ) ;
#22875 = CIRCLE ( 'NONE', #9724, 2.600000000000000089 ) ;
#22876 = ORIENTED_EDGE ( 'NONE', *, *, #20266, .T. ) ;
#22877 = DIRECTION ( 'NONE',  ( -1.000000000000000000, -0.000000000000000000, 1.047444401652940007E-14 ) ) ;
#22878 = DIRECTION ( 'NONE',  ( 1.047444401652940007E-14, 0.000000000000000000, 1.000000000000000000 ) ) ;
#22879 = ORIENTED_EDGE ( 'NONE', *, *, #20028, .F. ) ;
#22880 = EDGE_LOOP ( 'NONE', ( #22405, #24225, #18772, #14823 ) ) ;
#22881 = CARTESIAN_POINT ( 'NONE',  ( -62.09999999999997300, -2.509696570289218442, -0.2775754403374581791 ) ) ;
#22882 = DIRECTION ( 'NONE',  ( 1.000000000000000000, -0.000000000000000000, -1.047444401652940007E-14 ) ) ;
#22884 = CARTESIAN_POINT ( 'NONE',  ( -61.37479624186750016, -2.602756195442594844, 0.6931813454126620755 ) ) ;
#22883 = CARTESIAN_POINT ( 'NONE',  ( -58.74999999999997158, 2.944486372867092250, 1.699999999999803002 ) ) ;
#22885 = ORIENTED_EDGE ( 'NONE', *, *, #9811, .T. ) ;
#22886 = ORIENTED_EDGE ( 'NONE', *, *, #10032, .T. ) ;
#22887 = CARTESIAN_POINT ( 'NONE',  ( 63.50000000000004263, -0.7500000000000000000, 1.988246715072691018 ) ) ;
#22888 = ORIENTED_EDGE ( 'NONE', *, *, #4402, .F. ) ;
#22889 = EDGE_CURVE ( 'NONE', #1787, #9517, #22913, .T. ) ;
#22890 = CARTESIAN_POINT ( 'NONE',  ( 51.72405698199537483, 3.851083960639936077, -1.414090016722021614 ) ) ;
#22891 = ORIENTED_EDGE ( 'NONE', *, *, #25338, .F. ) ;
#22892 = CARTESIAN_POINT ( 'NONE',  ( 61.05386123796799325, 0.5990422800903768552, 1.861884024791375714 ) ) ;
#22893 = CIRCLE ( 'NONE', #17847, 0.1500000000000001887 ) ;
#22894 = DIRECTION ( 'NONE',  ( -0.8660254037844369313, 1.745740669421577130E-15, -0.5000000000000029976 ) ) ;
#22895 = DIRECTION ( 'NONE',  ( -2.614381936396368743E-16, 0.2008964009354147762, -0.9796124928211139560 ) ) ;
#22896 = CARTESIAN_POINT ( 'NONE',  ( 47.00000000000002842, -4.144729964592912097, -1.074323956810995240 ) ) ;
#22897 = CARTESIAN_POINT ( 'NONE',  ( -58.45655989232412963, 1.962990915244722245, 3.399999999999800071 ) ) ;
#22898 = CARTESIAN_POINT ( 'NONE',  ( -57.84585481156723574, 3.673546848079182414, 0.7533615035078065070 ) ) ;
#22899 = CARTESIAN_POINT ( 'NONE',  ( 16.10667815269232506, 3.062358472872010129, 4.459001320275609359 ) ) ;
#22900 = EDGE_CURVE ( 'NONE', #18265, #2938, #28574, .T. ) ;
#22901 = DIRECTION ( 'NONE',  ( 0.000000000000000000, 0.000000000000000000, -1.000000000000000000 ) ) ;
#22902 = CARTESIAN_POINT ( 'NONE',  ( 51.80000000000002558, 3.949999999998452971, 1.949999999999818767 ) ) ;
#22904 = DIRECTION ( 'NONE',  ( 0.000000000000000000, 0.000000000000000000, 1.000000000000000000 ) ) ;
#22903 = CARTESIAN_POINT ( 'NONE',  ( -54.39999999999999147, 1.499999999999995781, 4.029888335921750553 ) ) ;
#22905 =( NAMED_UNIT ( * ) PLANE_ANGLE_UNIT ( ) SI_UNIT ( $, .RADIAN. ) );
#22906 = CARTESIAN_POINT ( 'NONE',  ( 58.50000000000001421, -0.8000000000000000444, 2.489477856900920383 ) ) ;
#22907 = CARTESIAN_POINT ( 'NONE',  ( -36.40878371307407235, 0.9780988077348086174, 5.318542208600379517 ) ) ;
#22908 =( BOUNDED_CURVE ( )  B_SPLINE_CURVE ( 3, ( #26797, #30084, #11092, #3511 ),
 .UNSPECIFIED., .F., .T. ) 
 B_SPLINE_CURVE_WITH_KNOTS ( ( 4, 4 ),
 ( 5.008787943776981777, 5.118553210748935989 ),
 .UNSPECIFIED. ) 
 CURVE ( )  GEOMETRIC_REPRESENTATION_ITEM ( )  RATIONAL_B_SPLINE_CURVE ( ( 1.000000000000000000, 0.9989962175098912045, 0.9989962175098912045, 1.000000000000000000 ) ) 
 REPRESENTATION_ITEM ( '' )  );
#22909 = VECTOR ( 'NONE', #30778, 1000.000000000000000 ) ;
#22910 = ORIENTED_EDGE ( 'NONE', *, *, #23601, .F. ) ;
#22911 = CARTESIAN_POINT ( 'NONE',  ( 54.28867365409866608, 5.640057820322917692, -1.843143693225357538E-13 ) ) ;
#22912 = ORIENTED_EDGE ( 'NONE', *, *, #12571, .F. ) ;
#22913 = B_SPLINE_CURVE_WITH_KNOTS ( 'NONE', 3,
 ( #2900, #7790, #12698, #9873, #7966, #3055, #831, #29192, #19845, #22378, #27427, #20172, #3203, #17630, #12386, #22077 ),
 .UNSPECIFIED., .F., .F.,
 ( 4, 2, 2, 2, 2, 2, 2, 4 ),
 ( 1.734723475976807094E-18, 0.0004351083927046410721, 0.0008702167854092804095, 0.001740433570818558434, 0.002175541963523197446, 0.002610650356227836241, 0.003045758748932475037, 0.003480867141637114266 ),
 .UNSPECIFIED. ) ;
#22914 = CARTESIAN_POINT ( 'NONE',  ( 51.67711951922819225, -3.662677325876138035, 1.845585774149405944 ) ) ;
#22915 = EDGE_LOOP ( 'NONE', ( #24710, #9690, #5687, #27965 ) ) ;
#22916 = CARTESIAN_POINT ( 'NONE',  ( -54.15835481156724285, 4.108500314926515351, -1.367561758111409009 ) ) ;
#22918 = LINE ( 'NONE', #17857, #26787 ) ;
#22917 = CYLINDRICAL_SURFACE ( 'NONE', #29693, 2.000000000000000000 ) ;
#22919 = ORIENTED_EDGE ( 'NONE', *, *, #7620, .T. ) ;
#22920 = VERTEX_POINT ( 'NONE', #12245 ) ;
#22921 = CYLINDRICAL_SURFACE ( 'NONE', #25006, 4.384222560975607585 ) ;
#22922 = EDGE_CURVE ( 'NONE', #66, #7997, #6826, .T. ) ;
#22923 = CARTESIAN_POINT ( 'NONE',  ( 47.00000000000002132, 2.428612866367529932E-14, 0.000000000000000000 ) ) ;
#22924 = ORIENTED_EDGE ( 'NONE', *, *, #3615, .T. ) ;
#22926 = CARTESIAN_POINT ( 'NONE',  ( 50.25000000000000000, 1.470078920828055358, -1.320078920826817992 ) ) ;
#22925 = CARTESIAN_POINT ( 'NONE',  ( 57.05000000000001847, -0.6999999999999999556, 0.000000000000000000 ) ) ;
#22927 = FACE_OUTER_BOUND ( 'NONE', #20130, .T. ) ;
#22928 = ORIENTED_EDGE ( 'NONE', *, *, #18116, .F. ) ;
#22929 = CARTESIAN_POINT ( 'NONE',  ( -36.30347965937239962, 4.910307320510253426, -1.715181477143334021 ) ) ;
#22930 = DIRECTION ( 'NONE',  ( 1.000000000000000000, 3.053848253006669023E-16, -2.042510438544995415E-16 ) ) ;
#22931 = DIRECTION ( 'NONE',  ( -1.000000000000000000, 1.219044193948983948E-29, -3.491481338843133355E-15 ) ) ;
#22932 = CARTESIAN_POINT ( 'NONE',  ( 15.03925126672132961, 3.056483311920805690, 4.206888370749768846 ) ) ;
#22934 = CARTESIAN_POINT ( 'NONE',  ( -62.04999999999998295, -2.692921195145432822, 0.1479728852616695456 ) ) ;
#22933 = CIRCLE ( 'NONE', #24436, 4.100000000000022737 ) ;
#22935 = TOROIDAL_SURFACE ( 'NONE', #25451, 3.675000000000029132, 0.05000000000000000278 ) ;
#22936 = ORIENTED_EDGE ( 'NONE', *, *, #18830, .T. ) ;
#22937 = EDGE_CURVE ( 'NONE', #28072, #1808, #11384, .T. ) ;
#22938 = CARTESIAN_POINT ( 'NONE',  ( 15.22842924604237069, -2.525801262579322248, 4.794550356815982184 ) ) ;
#22939 = B_SPLINE_CURVE_WITH_KNOTS ( 'NONE', 3,
 ( #12159, #12760, #29090, #5319 ),
 .UNSPECIFIED., .F., .F.,
 ( 4, 4 ),
 ( 0.000000000000000000, 0.0003113238203253930773 ),
 .UNSPECIFIED. ) ;
#22940 = CARTESIAN_POINT ( 'NONE',  ( -60.59999999999997300, -2.476825173781434852, 0.9422510591782664591 ) ) ;
#22941 =( BOUNDED_SURFACE ( )  B_SPLINE_SURFACE ( 3, 2, ( 
 ( #15142, #725, #10385 ),
 ( #17690, #27332, #8948 ),
 ( #1512, #13539, #11170 ),
 ( #23372, #11494, #21175 ) ),
 .UNSPECIFIED., .F., .F., .F. ) 
 B_SPLINE_SURFACE_WITH_KNOTS ( ( 4, 4 ),
 ( 3, 3 ),
 ( 5.207223707550983072, 5.342072618596839462 ),
 ( 0.000000000000000000, 1.000000000000000000 ),
 .UNSPECIFIED. ) 
 GEOMETRIC_REPRESENTATION_ITEM ( )  RATIONAL_B_SPLINE_SURFACE ( (
 ( 1.000000000000000000, 0.8400189050393593870, 1.000000000000000000),
 ( 1.000000000000000000, 0.8502146092435617364, 1.000000000000000000),
 ( 1.000000000000000000, 0.8598532762618735781, 1.000000000000000000),
 ( 1.000000000000000000, 0.8689053228414193031, 1.000000000000000000) ) ) 
 REPRESENTATION_ITEM ( '' )  SURFACE ( )  );
#22942 = CARTESIAN_POINT ( 'NONE',  ( 49.00000000000002132, 1.401298464324817071E-42, -5.132477568099407673E-13 ) ) ;
#22943 = EDGE_CURVE ( 'NONE', #13554, #236, #31100, .T. ) ;
#22944 = CARTESIAN_POINT ( 'NONE',  ( -57.32202994616203995, 2.078460969082687626, -3.600000000000187494 ) ) ;
#22945 = CARTESIAN_POINT ( 'NONE',  ( 48.47161145301956253, 1.409900272549317268, -3.850000494969540554 ) ) ;
#22946 = ORIENTED_EDGE ( 'NONE', *, *, #2261, .F. ) ;
#22947 = CARTESIAN_POINT ( 'NONE',  ( 51.70000000000000995, 7.038595743567426471E-14, -4.600000000000215472 ) ) ;
#22948 = ORIENTED_EDGE ( 'NONE', *, *, #8203, .T. ) ;
#22949 = CARTESIAN_POINT ( 'NONE',  ( 49.00000000000002132, 5.529431079676072613E-15, -5.132477568099407673E-13 ) ) ;
#22950 = CIRCLE ( 'NONE', #21449, 3.075000000000000622 ) ;
#22952 = CARTESIAN_POINT ( 'NONE',  ( 53.96142581635486124, 5.170113101904351360, 2.049999999999811529 ) ) ;
#22951 = CARTESIAN_POINT ( 'NONE',  ( 48.34352038844360777, 1.212999249975939886, 3.917061424767716016 ) ) ;
#22953 = EDGE_LOOP ( 'NONE', ( #12918, #24417, #26780, #21622 ) ) ;
#22954 = ORIENTED_EDGE ( 'NONE', *, *, #29207, .T. ) ;
#22955 = AXIS2_PLACEMENT_3D ( 'NONE', #16397, #28587, #23522 ) ;
#22956 = EDGE_CURVE ( 'NONE', #19244, #9597, #7353, .T. ) ;
#22957 = CARTESIAN_POINT ( 'NONE',  ( 24.57460841532291695, 5.893272594507614315, 1.424999999999913447 ) ) ;
#22959 = PLANE ( 'NONE',  #11484 ) ;
#22958 = CARTESIAN_POINT ( 'NONE',  ( -60.82202994616204705, 2.078460969082646770, 3.599999999999791367 ) ) ;
#22960 = CARTESIAN_POINT ( 'NONE',  ( -55.79792740578360366, 3.330682475591789871, 0.6830477631804102723 ) ) ;
#22961 = EDGE_CURVE ( 'NONE', #24734, #27277, #3788, .T. ) ;
#22962 = CARTESIAN_POINT ( 'NONE',  ( -35.85663232820592583, -4.804073783693453059, -2.042134687550363648 ) ) ;
#22963 = DIRECTION ( 'NONE',  ( 0.000000000000000000, 0.2793919678926571337, 0.9601771338024398528 ) ) ;
#22964 =( NAMED_UNIT ( * ) PLANE_ANGLE_UNIT ( ) SI_UNIT ( $, .RADIAN. ) );
#22965 = ORIENTED_EDGE ( 'NONE', *, *, #30680, .T. ) ;
#22966 = EDGE_CURVE ( 'NONE', #22370, #26302, #1255, .T. ) ;
#22967 = CARTESIAN_POINT ( 'NONE',  ( 47.00000000000002132, -4.131056160354152240, -1.100000000000000089 ) ) ;
#22968 = CARTESIAN_POINT ( 'NONE',  ( 53.16217804548191594, 8.131925109091586279, -1.902110155464870944 ) ) ;
#22969 = DIRECTION ( 'NONE',  ( 1.000000000000000000, 0.000000000000000000, 0.000000000000000000 ) ) ;
#22970 = AXIS2_PLACEMENT_3D ( 'NONE', #26743, #28802, #283 ) ;
#22971 = CARTESIAN_POINT ( 'NONE',  ( 15.66436536804551238, -0.4008586329626869782, 5.396496690166844523 ) ) ;
#22972 = CARTESIAN_POINT ( 'NONE',  ( -59.69064771065831110, -2.230806985424941047, 1.533412112958392859 ) ) ;
#22974 = DIRECTION ( 'NONE',  ( 0.000000000000000000, 0.000000000000000000, 1.000000000000000000 ) ) ;
#22973 = CARTESIAN_POINT ( 'NONE',  ( -56.62499999999996447, 2.944486372867110457, -1.700000000000181810 ) ) ;
#22975 = PRODUCT_DEFINITION_SHAPE ( 'NONE', 'NONE',  #31337 ) ;
#22976 = AXIS2_PLACEMENT_3D ( 'NONE', #153, #7269, #17561 ) ;
#22977 = EDGE_CURVE ( 'NONE', #1571, #6093, #15389, .T. ) ;
#22978 = TOROIDAL_SURFACE ( 'NONE', #9335, 3.950000000000000178, 0.05000000000000000278 ) ;
#22979 = CARTESIAN_POINT ( 'NONE',  ( 53.43485098824196911, 4.477779790996729403, -2.048706274183198506 ) ) ;
#22981 = CARTESIAN_POINT ( 'NONE',  ( -54.49999999999997158, 1.284124781083705313, -3.226451220649914742 ) ) ;
#22980 = CARTESIAN_POINT ( 'NONE',  ( 69.20000000000004547, 0.6441176470588243497, 1.707553061179923892 ) ) ;
#22982 = VERTEX_POINT ( 'NONE', #29339 ) ;
#22983 = LINE ( 'NONE', #29943, #15454 ) ;
#22984 = EDGE_CURVE ( 'NONE', #17367, #4648, #28174, .T. ) ;
#22985 = CARTESIAN_POINT ( 'NONE',  ( 69.25000000000004263, 0.8558823529411765385, 2.268940368965340237 ) ) ;
#22987 = CARTESIAN_POINT ( 'NONE',  ( 58.65000000000001990, -0.8794134543721436881, -1.656314228058597848 ) ) ;
#22986 = CARTESIAN_POINT ( 'NONE',  ( 58.65000038048045639, 1.830965513785524967, 0.4043111005673222791 ) ) ;
#22988 = CARTESIAN_POINT ( 'NONE',  ( 47.00000000000002132, -3.976179070414207928, 1.000000000000000000 ) ) ;
#22989 = VERTEX_POINT ( 'NONE', #7649 ) ;
#22990 = CARTESIAN_POINT ( 'NONE',  ( 54.17887612135722009, 6.867997567695679706, 2.049999999999811973 ) ) ;
#22991 = CARTESIAN_POINT ( 'NONE',  ( 69.24999999999998579, 4.557543281186736018E-17, -2.729289321882064190 ) ) ;
#22992 = B_SPLINE_CURVE_WITH_KNOTS ( 'NONE', 3,
 ( #20352, #12873, #8141, #17814, #27451, #15419 ),
 .UNSPECIFIED., .F., .F.,
 ( 4, 2, 4 ),
 ( 3.337428612691802767E-06, 0.0002849599470117442990, 0.0005665824654107963184 ),
 .UNSPECIFIED. ) ;
#22993 = ORIENTED_EDGE ( 'NONE', *, *, #6018, .F. ) ;
#22994 = EDGE_CURVE ( 'NONE', #28523, #31227, #29570, .T. ) ;
#22995 = CIRCLE ( 'NONE', #4264, 0.4600000000000000755 ) ;
#22996 = CARTESIAN_POINT ( 'NONE',  ( -54.44999999999997442, 0.000000000000000000, 0.000000000000000000 ) ) ;
#22997 = ORIENTED_EDGE ( 'NONE', *, *, #10698, .F. ) ;
#22998 = EDGE_CURVE ( 'NONE', #19884, #9147, #24515, .T. ) ;
#22999 = DIRECTION ( 'NONE',  ( 0.000000000000000000, 0.000000000000000000, 1.000000000000000000 ) ) ;
#23000 = VERTEX_POINT ( 'NONE', #11107 ) ;
#23001 = CARTESIAN_POINT ( 'NONE',  ( -56.07202994616204705, -4.156921938165296204, -2.235752804180006664E-13 ) ) ;
#23002 = CARTESIAN_POINT ( 'NONE',  ( -59.26905989232412253, 2.944486372867092250, 1.699999999999800782 ) ) ;
#23003 = ORIENTED_EDGE ( 'NONE', *, *, #3201, .T. ) ;
#23004 = CARTESIAN_POINT ( 'NONE',  ( -54.39999999999997726, -3.524999999999988365, -2.336116317925493832E-13 ) ) ;
#23005 = VECTOR ( 'NONE', #12660, 1000.000000000000000 ) ;
#23006 = ORIENTED_EDGE ( 'NONE', *, *, #2711, .F. ) ;
#23007 = ORIENTED_EDGE ( 'NONE', *, *, #25476, .T. ) ;
#23008 = CARTESIAN_POINT ( 'NONE',  ( -58.81249999999996447, 3.925981830489463142, -1.945260624050196617E-13 ) ) ;
#23009 = CARTESIAN_POINT ( 'NONE',  ( 50.80000000000002558, -3.908336260473453727, 1.238913909465742202 ) ) ;
#23010 = CARTESIAN_POINT ( 'NONE',  ( 23.09424125814508244, 6.161968159343408580, -1.425000000000080647 ) ) ;
#23011 = DIRECTION ( 'NONE',  ( -1.000000000000000000, -3.054025858079668409E-16, 2.042474015755241579E-16 ) ) ;
#23012 = AXIS2_PLACEMENT_3D ( 'NONE', #11492, #14005, #19103 ) ;
#23013 = CARTESIAN_POINT ( 'NONE',  ( 15.03925126672132784, 5.377732432866644707, -0.5657657256215208319 ) ) ;
#23015 = DIRECTION ( 'NONE',  ( 1.000000000000000000, 1.047444401652940007E-14, 0.000000000000000000 ) ) ;
#23014 = CARTESIAN_POINT ( 'NONE',  ( 58.65000000000001990, 6.143261415694495821E-13, 3.111507638930570854E-58 ) ) ;
#23016 = VECTOR ( 'NONE', #6357, 1000.000000000000000 ) ;
#23017 = EDGE_CURVE ( 'NONE', #24464, #15593, #3669, .T. ) ;
#23018 = FILL_AREA_STYLE_COLOUR ( '', #21064 ) ;
#23019 = DIRECTION ( 'NONE',  ( 1.000000000000000000, 1.047444401652940007E-14, 0.000000000000000000 ) ) ;
#23020 = CARTESIAN_POINT ( 'NONE',  ( 48.30000000000001847, 0.6304760106459519342, 3.950000000000022826 ) ) ;
#23021 = CARTESIAN_POINT ( 'NONE',  ( 56.96603746669009638, 0.7703957983921196906, 2.483260519405945388 ) ) ;
#23022 = CARTESIAN_POINT ( 'NONE',  ( 53.96623127887670535, 7.375919661206682854, -2.050000000000187228 ) ) ;
#23023 = AXIS2_PLACEMENT_3D ( 'NONE', #4764, #4462, #2406 ) ;
#23024 = EDGE_CURVE ( 'NONE', #9046, #11104, #9368, .T. ) ;
#23025 = FACE_OUTER_BOUND ( 'NONE', #15269, .T. ) ;
#23026 = EDGE_LOOP ( 'NONE', ( #13818, #29231, #18873, #27969 ) ) ;
#23027 = B_SPLINE_CURVE_WITH_KNOTS ( 'NONE', 3,
 ( #18381, #27403, #10628, #5712, #8395, #22972, #30393 ),
 .UNSPECIFIED., .F., .F.,
 ( 4, 3, 4 ),
 ( 0.000000000000000000, 3.294740569033884786E-05, 5.798545858612056943E-05 ),
 .UNSPECIFIED. ) ;
#23028 = CARTESIAN_POINT ( 'NONE',  ( 50.38476904405314372, -1.115727354199205879, 3.895947837398489266 ) ) ;
#23029 = ORIENTED_EDGE ( 'NONE', *, *, #5958, .F. ) ;
#23030 =( NAMED_UNIT ( * ) PLANE_ANGLE_UNIT ( ) SI_UNIT ( $, .RADIAN. ) );
#23031 = CARTESIAN_POINT ( 'NONE',  ( 61.25000000000001421, 0.8813478542995215603, -1.623476567772370815 ) ) ;
#23033 = CARTESIAN_POINT ( 'NONE',  ( 47.10000000000000853, 2.479435708532144956E-14, -4.100000000000157740 ) ) ;
#23032 = CARTESIAN_POINT ( 'NONE',  ( -57.87499999999997868, -3.920666489018319112E-15, 3.399999999999793854 ) ) ;
#23034 = VERTEX_POINT ( 'NONE', #6207 ) ;
#23035 = ORIENTED_EDGE ( 'NONE', *, *, #5092, .T. ) ;
#23036 = AXIS2_PLACEMENT_3D ( 'NONE', #4626, #11912, #14284 ) ;
#23037 = DIRECTION ( 'NONE',  ( 0.000000000000000000, -0.2008964009354147484, 0.9796124928211139560 ) ) ;
#23038 = VERTEX_POINT ( 'NONE', #22703 ) ;
#23039 = AXIS2_PLACEMENT_3D ( 'NONE', #18553, #28199, #3806 ) ;
#23040 = CARTESIAN_POINT ( 'NONE',  ( 58.72200624034190497, -1.634766674883864956, 0.9185080301421469917 ) ) ;
#23041 = VERTEX_POINT ( 'NONE', #17933 ) ;
#23042 = CARTESIAN_POINT ( 'NONE',  ( 25.69798005928776874, 5.334073409756094009, -2.050000000000088640 ) ) ;
#23043 = CARTESIAN_POINT ( 'NONE',  ( 58.45000000000001705, 0.8000000000000000444, -2.421260002560649660 ) ) ;
#23044 = CARTESIAN_POINT ( 'NONE',  ( -59.69999999999997442, -3.399999999999991473, -2.235080921937235780E-13 ) ) ;
#23045 = ORIENTED_EDGE ( 'NONE', *, *, #15891, .F. ) ;
#23046 = CIRCLE ( 'NONE', #15440, 2.114644660940672605 ) ;
#23047 = CARTESIAN_POINT ( 'NONE',  ( 47.10000000000002274, -4.179189514726513011, -1.000000000000000000 ) ) ;
#23048 = AXIS2_PLACEMENT_3D ( 'NONE', #2366, #2533, #7125 ) ;
#23049 = CARTESIAN_POINT ( 'NONE',  ( 51.64281244548084260, -0.8321733326261766539, -1.569379851958523808 ) ) ;
#23050 = CARTESIAN_POINT ( 'NONE',  ( -58.51905989232412253, 2.944486372867092250, 1.699999999999803446 ) ) ;
#23051 = DIRECTION ( 'NONE',  ( -0.000000000000000000, 1.000000000000000000, 3.491481338843133355E-15 ) ) ;
#23052 = DIRECTION ( 'NONE',  ( 0.000000000000000000, 0.000000000000000000, -1.000000000000000000 ) ) ;
#23053 = DIRECTION ( 'NONE',  ( 0.000000000000000000, 0.2008964009354147484, -0.9796124928211138450 ) ) ;
#23054 = DIRECTION ( 'NONE',  ( -5.585208838989776544E-16, 0.05332224631852468255, -0.9985773570673163180 ) ) ;
#23056 = CARTESIAN_POINT ( 'NONE',  ( 51.80000000000003268, -3.933368109459640660, 2.186004417992994053 ) ) ;
#23055 = DIRECTION ( 'NONE',  ( 1.000000000000000000, 1.047444401652940007E-14, 0.000000000000000000 ) ) ;
#23057 = CIRCLE ( 'NONE', #10416, 0.1000000000000000333 ) ;
#23058 = CARTESIAN_POINT ( 'NONE',  ( -54.49999999999998579, -1.514093959731547701, 3.183260039818139209 ) ) ;
#23059 = EDGE_CURVE ( 'NONE', #27852, #19299, #25404, .T. ) ;
#23060 = CIRCLE ( 'NONE', #24071, 4.500000000000037303 ) ;
#23061 = DIRECTION ( 'NONE',  ( 0.8262273428075421755, 0.5633368246415175751, 0.000000000000000000 ) ) ;
#23062 = DIRECTION ( 'NONE',  ( 1.000000000000000000, 0.000000000000000000, -3.491481338843133355E-15 ) ) ;
#23063 = VERTEX_POINT ( 'NONE', #20787 ) ;
#23064 = VECTOR ( 'NONE', #5527, 1000.000000000000000 ) ;
#23065 = CARTESIAN_POINT ( 'NONE',  ( -58.81249999999996447, -0.7533615035078081723, 3.673546848079176197 ) ) ;
#23066 = AXIS2_PLACEMENT_3D ( 'NONE', #20949, #2242, #20800 ) ;
#23067 = ORIENTED_EDGE ( 'NONE', *, *, #22994, .F. ) ;
#23068 = VECTOR ( 'NONE', #9384, 1000.000000000000000 ) ;
#23069 = CARTESIAN_POINT ( 'NONE',  ( 50.93159257904724058, -4.031600731367472434, 1.173113608354092730 ) ) ;
#23070 = EDGE_LOOP ( 'NONE', ( #7654, #18792, #20485, #8418, #195, #26107, #3126, #3829 ) ) ;
#23071 = COLOUR_RGB ( '', 0.31764706, 0.68627451, 0.89019608) ;
#23072 = CARTESIAN_POINT ( 'NONE',  ( 51.80000000000002558, 8.600000000000108002, 1.949999999999818767 ) ) ;
#23073 = CARTESIAN_POINT ( 'NONE',  ( -58.47085481156723574, 1.184343223768590692, 3.558065644182727194 ) ) ;
#23075 = CARTESIAN_POINT ( 'NONE',  ( 57.00000000000001421, -0.7500000000000000000, -2.421260002560649216 ) ) ;
#23074 = CARTESIAN_POINT ( 'NONE',  ( 60.98985426489760187, -0.5466942006285966382, 1.538695758318286311 ) ) ;
#23076 = EDGE_LOOP ( 'NONE', ( #13249, #16371, #19029, #3913 ) ) ;
#23077 = ORIENTED_EDGE ( 'NONE', *, *, #6721, .F. ) ;
#23078 = CARTESIAN_POINT ( 'NONE',  ( 29.93623257617671030, 6.616414062163364029, -2.050000000000104183 ) ) ;
#23079 = EDGE_CURVE ( 'NONE', #6282, #20869, #22393, .T. ) ;
#23080 = CARTESIAN_POINT ( 'NONE',  ( 47.00000000000002132, 2.478823385132571406E-14, 4.100000000000022737 ) ) ;
#23081 = CIRCLE ( 'NONE', #23574, 0.1000000000000000472 ) ;
#23082 = ORIENTED_EDGE ( 'NONE', *, *, #22566, .F. ) ;
#23084 = DIRECTION ( 'NONE',  ( -1.000000000000000000, 0.000000000000000000, 0.000000000000000000 ) ) ;
#23083 = CYLINDRICAL_SURFACE ( 'NONE', #28209, 0.05000000000000143219 ) ;
#23085 = CARTESIAN_POINT ( 'NONE',  ( -67.99999999999995737, -3.266925685480207642E-16, 2.202315069465528948E-15 ) ) ;
#23086 = ORIENTED_EDGE ( 'NONE', *, *, #16282, .F. ) ;
#23087 = CARTESIAN_POINT ( 'NONE',  ( -35.85663232820600399, 5.377732432866631385, -0.5657657256215193886 ) ) ;
#23088 = CIRCLE ( 'NONE', #28135, 0.09999999999999982514 ) ;
#23089 = CARTESIAN_POINT ( 'NONE',  ( 58.75000000000000000, 1.877732920581777654, -0.6121634413828943577 ) ) ;
#23090 = CARTESIAN_POINT ( 'NONE',  ( -36.40878371307407235, -2.334862116275012944, 4.877703086529554533 ) ) ;
#23091 = CIRCLE ( 'NONE', #24585, 4.100000000000001421 ) ;
#23092 = DIRECTION ( 'NONE',  ( -1.000000000000000000, 1.219044193948983948E-29, -3.491481338843133355E-15 ) ) ;
#23093 = PRODUCT_RELATED_PRODUCT_CATEGORY ( 'part', '', ( #16726 ) ) ;
#23094 = FACE_OUTER_BOUND ( 'NONE', #11691, .T. ) ;
#23095 = CIRCLE ( 'NONE', #4360, 0.1000000000000000472 ) ;
#23096 = AXIS2_PLACEMENT_3D ( 'NONE', #6766, #8810, #26080 ) ;
#23097 = AXIS2_PLACEMENT_3D ( 'NONE', #7177, #30764, #25853 ) ;
#23098 = STYLED_ITEM ( 'NONE', ( #23844 ), #25800 ) ;
#23099 = CARTESIAN_POINT ( 'NONE',  ( 15.03925126672132961, 3.779372838781728916, 3.883777296072592922 ) ) ;
#23100 =( BOUNDED_SURFACE ( )  B_SPLINE_SURFACE ( 3, 2, ( 
 ( #13663, #23345, #31044 ),
 ( #9367, #19034, #7005 ),
 ( #17274, #10292, #26778 ),
 ( #24850, #19665, #22195 ) ),
 .UNSPECIFIED., .F., .F., .F. ) 
 B_SPLINE_SURFACE_WITH_KNOTS ( ( 4, 4 ),
 ( 3, 3 ),
 ( 6.291704175186453303E-05, 0.0002258017310250082428 ),
 ( 0.000000000000000000, 1.000000000000000000 ),
 .UNSPECIFIED. ) 
 GEOMETRIC_REPRESENTATION_ITEM ( )  RATIONAL_B_SPLINE_SURFACE ( (
 ( 1.000000000000000000, 0.8397191227596314533, 1.000000000000000000),
 ( 1.000000000000000000, 0.8408372669632975249, 1.000000000000000000),
 ( 1.000000000000000000, 0.7715695853058209819, 1.000000000000000000),
 ( 1.000000000000000000, 0.7071067811864981678, 1.000000000000000000) ) ) 
 REPRESENTATION_ITEM ( '' )  SURFACE ( )  );
#23101 = CARTESIAN_POINT ( 'NONE',  ( -55.11042740578361077, 3.725040285533371964, -1.239922660687673650 ) ) ;
#23102 = ADVANCED_FACE ( 'NONE', ( #25511 ), #30268, .T. ) ;
#23103 = DIRECTION ( 'NONE',  ( -1.000000000000000000, -1.786976680021873984E-16, -2.459562394685737870E-16 ) ) ;
#23104 = AXIS2_PLACEMENT_3D ( 'NONE', #29369, #17341, #26987 ) ;
#23105 = AXIS2_PLACEMENT_3D ( 'NONE', #9816, #7448, #17118 ) ;
#23106 = CARTESIAN_POINT ( 'NONE',  ( -59.29999999999997584, 2.330309927981285032E-15, 4.253626757584724400E-16 ) ) ;
#23107 = CIRCLE ( 'NONE', #29159, 0.2500000000000000000 ) ;
#23108 = CARTESIAN_POINT ( 'NONE',  ( 58.75000000000004263, -1.964000600390203743, 0.09700564724538153494 ) ) ;
#23109 = CARTESIAN_POINT ( 'NONE',  ( 48.40000000000002700, 0.7707709757764751313, -3.938803467580343831 ) ) ;
#23110 = ORIENTED_EDGE ( 'NONE', *, *, #16676, .T. ) ;
#23111 = CARTESIAN_POINT ( 'NONE',  ( 58.75000000000000000, 1.571497941946486288, 1.022750809562083418 ) ) ;
#23112 = CIRCLE ( 'NONE', #15000, 0.1000000000000000472 ) ;
#23113 = ORIENTED_EDGE ( 'NONE', *, *, #20911, .F. ) ;
#23114 = CARTESIAN_POINT ( 'NONE',  ( 61.25000000000000000, 1.895722432253201140, -0.6373668173460090847 ) ) ;
#23116 = DIRECTION ( 'NONE',  ( 1.000000000000000000, -0.000000000000000000, -1.047444401652940007E-14 ) ) ;
#23115 = CARTESIAN_POINT ( 'NONE',  ( 57.00059118976931671, 0.7088470050679284151, -2.446935707828179485 ) ) ;
#23117 = VECTOR ( 'NONE', #29321, 1000.000000000000000 ) ;
#23118 = ORIENTED_EDGE ( 'NONE', *, *, #18313, .F. ) ;
#23119 = VERTEX_POINT ( 'NONE', #3983 ) ;
#23120 = DIRECTION ( 'NONE',  ( 1.000000000000000000, 1.047444401652940007E-14, 0.000000000000000000 ) ) ;
#23121 = AXIS2_PLACEMENT_3D ( 'NONE', #22355, #7940, #21328 ) ;
#23122 = EDGE_CURVE ( 'NONE', #6274, #16870, #10649, .T. ) ;
#23123 = DIRECTION ( 'NONE',  ( 3.002035892788116966E-16, -0.9996898646859343485, -0.02490330187381123786 ) ) ;
#23124 = COLOUR_RGB ( '', 0.08235294, 0.09019608, 0.10196078) ;
#23125 = CARTESIAN_POINT ( 'NONE',  ( 57.00000000000001421, 0.000000000000000000, 0.000000000000000000 ) ) ;
#23126 = EDGE_LOOP ( 'NONE', ( #2509, #25626, #2898, #27701 ) ) ;
#23127 = CARTESIAN_POINT ( 'NONE',  ( -57.42292740578360366, 2.256877952708269408, -2.542931754211925188 ) ) ;
#23128 = CARTESIAN_POINT ( 'NONE',  ( -36.22909104983323658, -4.895911367891200960, -2.323639554370684035 ) ) ;
#23129 = APPLICATION_PROTOCOL_DEFINITION ( 'draft international standard', 'automotive_design', 1998, #9192 ) ;
#23130 = CARTESIAN_POINT ( 'NONE',  ( -59.35396298745919097, 2.308928725093315926, 1.300518551040214188 ) ) ;
#23131 = CIRCLE ( 'NONE', #7925, 2.374999999999998668 ) ;
#23132 = ORIENTED_EDGE ( 'NONE', *, *, #13970, .T. ) ;
#23133 = AXIS2_PLACEMENT_3D ( 'NONE', #4059, #11036, #25283 ) ;
#23134 = CARTESIAN_POINT ( 'NONE',  ( 47.06945706549019093, -4.177413309949347564, -1.004109922956873069 ) ) ;
#23135 = CIRCLE ( 'NONE', #21644, 0.1500000000000001887 ) ;
#23136 = CARTESIAN_POINT ( 'NONE',  ( -36.25997906085253675, 2.880023619481788533, -4.335093843541867109 ) ) ;
#23137 = DIRECTION ( 'NONE',  ( -1.000000000000000000, -0.000000000000000000, -0.000000000000000000 ) ) ;
#23138 = FACE_OUTER_BOUND ( 'NONE', #26332, .T. ) ;
#23139 = FACE_OUTER_BOUND ( 'NONE', #17423, .T. ) ;
#23140 = CIRCLE ( 'NONE', #17577, 4.100000000000001421 ) ;
#23141 = EDGE_CURVE ( 'NONE', #14302, #29895, #9237, .T. ) ;
#23142 = CIRCLE ( 'NONE', #21629, 5.407411300779133789 ) ;
#23144 = CARTESIAN_POINT ( 'NONE',  ( -35.98994760229917489, 0.4576450652446111267, -5.200000002521294462 ) ) ;
#23143 = CARTESIAN_POINT ( 'NONE',  ( 50.59602332238209499, -0.1408342061598477080, -1.212874140286674507 ) ) ;
#23145 = VECTOR ( 'NONE', #28709, 1000.000000000000000 ) ;
#23146 = EDGE_CURVE ( 'NONE', #9190, #26864, #17650, .T. ) ;
#23147 = CARTESIAN_POINT ( 'NONE',  ( 52.54176024732381478, 4.030513272393515756, -2.045987183813463783 ) ) ;
#23149 = CARTESIAN_POINT ( 'NONE',  ( -54.49999999999997868, 3.433573722926734462, -1.225502693192425774 ) ) ;
#23148 = CARTESIAN_POINT ( 'NONE',  ( -44.59999999999999432, -1.400000000000007017, 4.029888335921774534 ) ) ;
#23150 = EDGE_LOOP ( 'NONE', ( #5300, #26228, #14179, #4872 ) ) ;
#23151 = CARTESIAN_POINT ( 'NONE',  ( 61.01567056675808942, -0.5566600462012117889, -1.706616170210760508 ) ) ;
#23152 = CYLINDRICAL_SURFACE ( 'NONE', #14329, 0.05000000000000143219 ) ;
#23153 = AXIS2_PLACEMENT_3D ( 'NONE', #16113, #25762, #30979 ) ;
#23155 = PLANE ( 'NONE',  #17685 ) ;
#23154 = CARTESIAN_POINT ( 'NONE',  ( 58.65000045311409593, 1.787855644602297067, 0.5652242121858112034 ) ) ;
#23156 = LINE ( 'NONE', #25203, #20113 ) ;
#23157 = VERTEX_POINT ( 'NONE', #13018 ) ;
#23158 = CARTESIAN_POINT ( 'NONE',  ( 53.60009913848112717, 4.619321414059948339, 2.049999999999812861 ) ) ;
#23159 = CARTESIAN_POINT ( 'NONE',  ( 15.03925126672132961, 3.056483311920904278, -4.206888370749696904 ) ) ;
#23160 = AXIS2_PLACEMENT_3D ( 'NONE', #5292, #19586, #5624 ) ;
#23161 = EDGE_CURVE ( 'NONE', #29689, #18491, #13165, .T. ) ;
#23162 = VECTOR ( 'NONE', #17365, 1000.000000000000000 ) ;
#23163 = ORIENTED_EDGE ( 'NONE', *, *, #15153, .T. ) ;
#23164 = CARTESIAN_POINT ( 'NONE',  ( 50.25000000000000711, 1.039502773796242119, 1.800471618825331355 ) ) ;
#23165 = ORIENTED_EDGE ( 'NONE', *, *, #9527, .T. ) ;
#23166 = CARTESIAN_POINT ( 'NONE',  ( 15.32752150720753370, 2.228039998204479843, -4.927410888447814052 ) ) ;
#23167 = CARTESIAN_POINT ( 'NONE',  ( 47.43974768990582902, -4.327031471043519595, -1.563408443049195018 ) ) ;
#23168 = ORIENTED_EDGE ( 'NONE', *, *, #967, .F. ) ;
#23169 = CARTESIAN_POINT ( 'NONE',  ( -54.82202994616206126, 2.078460969082646770, 3.599999999999812683 ) ) ;
#23170 = AXIS2_PLACEMENT_3D ( 'NONE', #12277, #11980, #14804 ) ;
#23171 = CARTESIAN_POINT ( 'NONE',  ( -56.58155989232411542, -1.962990915244706924, -3.400000000000206857 ) ) ;
#23172 = ORIENTED_EDGE ( 'NONE', *, *, #15803, .T. ) ;
#23173 = CARTESIAN_POINT ( 'NONE',  ( 58.64999999999999858, 1.872332544501737361, 0.09997921184905503300 ) ) ;
#23174 = ORIENTED_EDGE ( 'NONE', *, *, #20982, .T. ) ;
#23175 = EDGE_CURVE ( 'NONE', #17048, #26590, #18105, .T. ) ;
#23176 = ORIENTED_EDGE ( 'NONE', *, *, #20952, .F. ) ;
#23177 = CARTESIAN_POINT ( 'NONE',  ( -55.31249999999997158, -1.962990915244707368, -3.400000000000203304 ) ) ;
#23178 = FACE_OUTER_BOUND ( 'NONE', #31041, .T. ) ;
#23179 = CARTESIAN_POINT ( 'NONE',  ( 25.71580480958624193, 5.235626398479810817, -1.425000000000088862 ) ) ;
#23180 = DIRECTION ( 'NONE',  ( 0.000000000000000000, 0.000000000000000000, -1.000000000000000000 ) ) ;
#23181 = DIRECTION ( 'NONE',  ( 0.000000000000000000, 0.000000000000000000, 1.000000000000000000 ) ) ;
#23182 = CIRCLE ( 'NONE', #15065, 0.04999999999999988481 ) ;
#23184 = FACE_OUTER_BOUND ( 'NONE', #26958, .T. ) ;
#23183 = PLANE ( 'NONE',  #5407 ) ;
#23185 = ADVANCED_FACE ( 'NONE', ( #8423 ), #6064, .T. ) ;
#23186 = EDGE_CURVE ( 'NONE', #9168, #18443, #8574, .T. ) ;
#23187 = LINE ( 'NONE', #1949, #26606 ) ;
#23188 = CARTESIAN_POINT ( 'NONE',  ( -59.61639066107911589, 2.342446846742921807, -1.242019481833310568 ) ) ;
#23189 = CARTESIAN_POINT ( 'NONE',  ( -59.69824320556942610, 2.099492949945970466, 1.747093667920370352 ) ) ;
#23190 = CARTESIAN_POINT ( 'NONE',  ( 57.01033040358699111, 0.8080171122822069618, 2.471263581425196421 ) ) ;
#23191 = CARTESIAN_POINT ( 'NONE',  ( 51.80000000000002558, -4.179189514726507682, 0.9999999999999997780 ) ) ;
#23192 = CARTESIAN_POINT ( 'NONE',  ( -59.29999999999997584, 3.111192537532289304, 2.093557019620777115 ) ) ;
#23193 = VERTEX_POINT ( 'NONE', #5049 ) ;
#23194 = CARTESIAN_POINT ( 'NONE',  ( -67.98046642889043767, -3.207269654211098678E-16, 2.198325388322918801E-15 ) ) ;
#23195 = CARTESIAN_POINT ( 'NONE',  ( 58.65000000000002700, -0.8495817349406442620, 1.671477153793675896 ) ) ;
#23196 = ORIENTED_EDGE ( 'NONE', *, *, #28366, .T. ) ;
#23197 = FACE_OUTER_BOUND ( 'NONE', #6023, .T. ) ;
#23199 = CARTESIAN_POINT ( 'NONE',  ( 61.25000000000004263, -1.791164585741916282, 0.8897917884436183922 ) ) ;
#23198 = CARTESIAN_POINT ( 'NONE',  ( -54.87499999999998579, -3.920666489018356189E-15, 3.399999999999804068 ) ) ;
#23200 = EDGE_LOOP ( 'NONE', ( #4202, #16760, #8038, #28449 ) ) ;
#23201 = ORIENTED_EDGE ( 'NONE', *, *, #20324, .F. ) ;
#23202 = AXIS2_PLACEMENT_3D ( 'NONE', #22949, #776, #10603 ) ;
#23203 = CARTESIAN_POINT ( 'NONE',  ( 51.69999999079093556, -4.079797993893543584, -2.128382101831790330 ) ) ;
#23204 = ORIENTED_EDGE ( 'NONE', *, *, #21902, .T. ) ;
#23205 = CARTESIAN_POINT ( 'NONE',  ( 48.50000000000002132, -1.391941090707485396, 3.850000000000022737 ) ) ;
#23206 = ORIENTED_EDGE ( 'NONE', *, *, #12313, .F. ) ;
#23207 = CARTESIAN_POINT ( 'NONE',  ( 58.65000000000004121, -1.834410884275093911, -0.3880228184666750235 ) ) ;
#23208 = CARTESIAN_POINT ( 'NONE',  ( -54.39999999999997726, -6.102218906431378987E-14, -2.213041600731275921E-13 ) ) ;
#23209 = EDGE_CURVE ( 'NONE', #26303, #25442, #12684, .T. ) ;
#23210 = LINE ( 'NONE', #18770, #14673 ) ;
#23211 = ORIENTED_EDGE ( 'NONE', *, *, #17328, .F. ) ;
#23212 = EDGE_CURVE ( 'NONE', #468, #9147, #13251, .T. ) ;
#23213 = DIRECTION ( 'NONE',  ( 3.489354422748178582E-15, -1.218509414717996338E-16, 1.000000000000000000 ) ) ;
#23214 = CARTESIAN_POINT ( 'NONE',  ( -54.78335481156722864, 3.238593381231848145, 2.874284765127022023 ) ) ;
#23215 = DIRECTION ( 'NONE',  ( -1.000000000000000000, -3.053848253006669023E-16, 2.042510438544995415E-16 ) ) ;
#23216 = DIRECTION ( 'NONE',  ( 1.000000000000000000, 0.000000000000000000, -1.047444401652940007E-14 ) ) ;
#23217 = CARTESIAN_POINT ( 'NONE',  ( -60.49999999999997868, 2.524216908331986975, 0.06288083723137545544 ) ) ;
#23218 = CARTESIAN_POINT ( 'NONE',  ( 53.81456879268866800, 5.799118509429035839, -1.784594539754255749 ) ) ;
#23220 = CARTESIAN_POINT ( 'NONE',  ( 58.75000000000000711, 1.800471618824440734, 1.039502773797588597 ) ) ;
#23219 = CARTESIAN_POINT ( 'NONE',  ( -61.38768957378469793, -2.555570530917468997, 0.6498638426362197684 ) ) ;
#23221 = PRESENTATION_LAYER_ASSIGNMENT (  '', '', ( #16140 ) ) ;
#23222 = LINE ( 'NONE', #1357, #29118 ) ;
#23223 = DIRECTION ( 'NONE',  ( 0.000000000000000000, -1.224646799147353947E-16, 1.000000000000000000 ) ) ;
#23224 = AXIS2_PLACEMENT_3D ( 'NONE', #26555, #5026, #24032 ) ;
#23225 = CARTESIAN_POINT ( 'NONE',  ( -44.49999999999997868, 2.750000000000007994, -1.490445676513672770E-13 ) ) ;
#23226 = ORIENTED_EDGE ( 'NONE', *, *, #4707, .F. ) ;
#23227 = CARTESIAN_POINT ( 'NONE',  ( 54.11187982984932887, 5.509389740176599659, -2.050000000000188560 ) ) ;
#23228 = ORIENTED_EDGE ( 'NONE', *, *, #30506, .F. ) ;
#23229 = ORIENTED_EDGE ( 'NONE', *, *, #19188, .T. ) ;
#23230 = CARTESIAN_POINT ( 'NONE',  ( 51.60235211085279161, -3.901663320877444718, 1.540393549661617456 ) ) ;
#23231 = VERTEX_POINT ( 'NONE', #26573 ) ;
#23232 = CARTESIAN_POINT ( 'NONE',  ( 53.55869261961985472, 7.702978059423599255, 1.861455469535095331 ) ) ;
#23233 = CARTESIAN_POINT ( 'NONE',  ( -56.90835481156723574, -0.8699069336946628761, 4.241846523238430144 ) ) ;
#23234 = AXIS2_PLACEMENT_3D ( 'NONE', #28498, #6802, #11718 ) ;
#23236 = CARTESIAN_POINT ( 'NONE',  ( -36.39645873810206211, 3.590618801409514838, 4.051716037497281597 ) ) ;
#23235 = CARTESIAN_POINT ( 'NONE',  ( 60.89332643996541350, -0.4999999999993604560, 1.718465855720804569 ) ) ;
#23237 = ORIENTED_EDGE ( 'NONE', *, *, #10592, .F. ) ;
#23238 = ORIENTED_EDGE ( 'NONE', *, *, #27242, .T. ) ;
#23239 = CARTESIAN_POINT ( 'NONE',  ( 24.21343478405543692, 5.692107421281859203, -2.050000000000083755 ) ) ;
#23240 = AXIS2_PLACEMENT_3D ( 'NONE', #25172, #13127, #22816 ) ;
#23241 = ORIENTED_EDGE ( 'NONE', *, *, #4608, .F. ) ;
#23243 = DIRECTION ( 'NONE',  ( -3.491481338843133355E-15, 0.000000000000000000, -1.000000000000000000 ) ) ;
#23242 = DIRECTION ( 'NONE',  ( 0.000000000000000000, 0.000000000000000000, -1.000000000000000000 ) ) ;
#23244 = CARTESIAN_POINT ( 'NONE',  ( 47.00000000000002132, -1.391941090707485396, 3.750000000000022649 ) ) ;
#23245 = ORIENTED_EDGE ( 'NONE', *, *, #7085, .T. ) ;
#23246 = CARTESIAN_POINT ( 'NONE',  ( -36.48174642953002689, 5.008501212420958026, -2.048848402342137387 ) ) ;
#23247 = ADVANCED_FACE ( 'NONE', ( #21858 ), #2193, .T. ) ;
#23248 = DIRECTION ( 'NONE',  ( 0.000000000000000000, 1.000000000000000000, 4.336808689942015369E-15 ) ) ;
#23249 = ADVANCED_FACE ( 'NONE', ( #289 ), #17101, .T. ) ;
#23250 = AXIS2_PLACEMENT_3D ( 'NONE', #6514, #22843, #30091 ) ;
#23251 = CARTESIAN_POINT ( 'NONE',  ( -54.39999999999999147, 1.599999999999998090, 3.363870538531247512 ) ) ;
#23252 = DIRECTION ( 'NONE',  ( -1.000000000000000000, -1.047444401652940007E-14, 0.000000000000000000 ) ) ;
#23253 = EDGE_CURVE ( 'NONE', #2488, #20831, #20877, .T. ) ;
#23254 = CARTESIAN_POINT ( 'NONE',  ( -57.50952994616203995, -3.117691453623963938, -1.800000000000215206 ) ) ;
#23255 = AXIS2_PLACEMENT_3D ( 'NONE', #26955, #24582, #8268 ) ;
#23256 = FACE_OUTER_BOUND ( 'NONE', #11038, .T. ) ;
#23257 = CARTESIAN_POINT ( 'NONE',  ( -59.04792740578360366, -1.073804522883505363, -3.225979517392338902 ) ) ;
#23258 = EDGE_CURVE ( 'NONE', #15457, #28051, #15804, .T. ) ;
#23259 = CARTESIAN_POINT ( 'NONE',  ( -35.85663232820584057, 0.4576450603546987628, 5.200000000000000178 ) ) ;
#23260 = CARTESIAN_POINT ( 'NONE',  ( 44.98443556292537693, -3.726179070414207928, 1.100000000000000311 ) ) ;
#23261 = CARTESIAN_POINT ( 'NONE',  ( -57.22499999999997300, 2.964020293532818446E-15, 1.549317489258312010E-18 ) ) ;
#23262 = CARTESIAN_POINT ( 'NONE',  ( 53.31625799375803609, 4.986123645165291940, 1.613809813132785820 ) ) ;
#23263 = DIRECTION ( 'NONE',  ( 0.000000000000000000, 0.000000000000000000, 1.000000000000000000 ) ) ;
#23264 = ORIENTED_EDGE ( 'NONE', *, *, #22956, .T. ) ;
#23265 = CIRCLE ( 'NONE', #5041, 2.600000000000000089 ) ;
#23266 = CARTESIAN_POINT ( 'NONE',  ( 58.65844932252345245, 1.607045716458644913, 0.9660788770032165962 ) ) ;
#23267 = ORIENTED_EDGE ( 'NONE', *, *, #12779, .T. ) ;
#23268 = CARTESIAN_POINT ( 'NONE',  ( -44.59999999999996589, 1.500000000000023759, -3.959797974644836405 ) ) ;
#23270 = CARTESIAN_POINT ( 'NONE',  ( 58.75000000000003553, -1.320082690054269703, 1.469015551795342933 ) ) ;
#23269 = CARTESIAN_POINT ( 'NONE',  ( 68.00000000000000000, -0.7500000000000000000, -2.238246715074068582 ) ) ;
#23271 = ORIENTED_EDGE ( 'NONE', *, *, #20813, .T. ) ;
#23272 = VERTEX_POINT ( 'NONE', #19633 ) ;
#23273 = FACE_BOUND ( 'NONE', #10355, .T. ) ;
#23274 = CIRCLE ( 'NONE', #9120, 3.625000000000024869 ) ;
#23275 = SPHERICAL_SURFACE ( 'NONE', #485, 0.1000000000000000056 ) ;
#23277 = CARTESIAN_POINT ( 'NONE',  ( -55.78335481156724285, 0.7533615035078067290, -3.673546848079180194 ) ) ;
#23276 = CARTESIAN_POINT ( 'NONE',  ( -60.13452994616204705, 3.117691453623979481, 1.799999999999798428 ) ) ;
#23278 = VERTEX_POINT ( 'NONE', #29272 ) ;
#23279 = CARTESIAN_POINT ( 'NONE',  ( -58.67292740578360366, 1.073804522883521351, 3.225979517392336682 ) ) ;
#23280 = CARTESIAN_POINT ( 'NONE',  ( -36.92405921417685022, 3.294441450831133711, 4.290383166762168798 ) ) ;
#23281 = PRODUCT_CONTEXT ( 'NONE', #5898, 'mechanical' ) ;
#23282 = EDGE_CURVE ( 'NONE', #16493, #31001, #10735, .T. ) ;
#23283 = DIRECTION ( 'NONE',  ( 0.000000000000000000, 0.000000000000000000, 1.000000000000000000 ) ) ;
#23284 = AXIS2_PLACEMENT_3D ( 'NONE', #30615, #30314, #21158 ) ;
#23285 = DIRECTION ( 'NONE',  ( 1.000000000000000000, 0.000000000000000000, 0.000000000000000000 ) ) ;
#23286 = CARTESIAN_POINT ( 'NONE',  ( -60.89492752328840908, -2.499300970757945439, -1.026269669383801153 ) ) ;
#23287 = ORIENTED_EDGE ( 'NONE', *, *, #5001, .T. ) ;
#23288 = DIRECTION ( 'NONE',  ( 0.03489949670247565611, 0.9993908270190966503, 0.000000000000000000 ) ) ;
#23289 = CARTESIAN_POINT ( 'NONE',  ( 61.24019690292467999, 0.9013423465692351755, -1.739682280369793999 ) ) ;
#23290 = CARTESIAN_POINT ( 'NONE',  ( 51.17950113889408925, 0.9670426259161513105, 1.523577707254208269 ) ) ;
#23291 = LINE ( 'NONE', #23766, #8375 ) ;
#23292 = AXIS2_PLACEMENT_3D ( 'NONE', #4806, #21460, #9418 ) ;
#23293 = CARTESIAN_POINT ( 'NONE',  ( 15.03925126672132961, -1.123735532908297863, -5.289358697221544503 ) ) ;
#23294 = ADVANCED_FACE ( 'NONE', ( #4578 ), #9509, .T. ) ;
#23296 = LINE ( 'NONE', #8854, #18498 ) ;
#23295 = DIRECTION ( 'NONE',  ( 1.000000000000000000, 1.047444401652940007E-14, 0.000000000000000000 ) ) ;
#23297 = LINE ( 'NONE', #3966, #15977 ) ;
#23299 = CARTESIAN_POINT ( 'NONE',  ( -35.85663232820584057, -5.086913985776155833, -1.171642053949114803 ) ) ;
#23298 = LINE ( 'NONE', #21403, #2380 ) ;
#23300 = ORIENTED_EDGE ( 'NONE', *, *, #8623, .F. ) ;
#23301 = CARTESIAN_POINT ( 'NONE',  ( -62.06722781964786151, -2.633694437091016027, -0.3282923398133328896 ) ) ;
#23302 = DIRECTION ( 'NONE',  ( 1.000000000000000000, 1.047444401652940007E-14, 0.000000000000000000 ) ) ;
#23304 = DIRECTION ( 'NONE',  ( -0.4999999999999965583, 3.023711536277464094E-15, -0.8660254037844407060 ) ) ;
#23303 = CARTESIAN_POINT ( 'NONE',  ( -59.19834903927996805, 2.558621439192835023, -0.9489102922513357186 ) ) ;
#23305 = DIRECTION ( 'NONE',  ( 1.000000000000000000, 0.000000000000000000, -1.047444401652940007E-14 ) ) ;
#23306 = VERTEX_POINT ( 'NONE', #9958 ) ;
#23307 = CARTESIAN_POINT ( 'NONE',  ( 53.05088594538233338, 4.168914605591084843, 2.049999999999814637 ) ) ;
#23308 = DIRECTION ( 'NONE',  ( -1.000000000000000000, 1.219044193948983948E-29, -3.491481338843133355E-15 ) ) ;
#23309 = VERTEX_POINT ( 'NONE', #2674 ) ;
#23310 = DIRECTION ( 'NONE',  ( 0.000000000000000000, 1.000000000000000000, 3.491481338843133355E-15 ) ) ;
#23311 = ORIENTED_EDGE ( 'NONE', *, *, #12019, .F. ) ;
#23312 = CARTESIAN_POINT ( 'NONE',  ( 58.75000000000000000, 1.972190280208463653, 0.1053114364810046333 ) ) ;
#23313 = ORIENTED_EDGE ( 'NONE', *, *, #8234, .F. ) ;
#23314 = AXIS2_PLACEMENT_3D ( 'NONE', #27435, #13901, #29814 ) ;
#23315 = CARTESIAN_POINT ( 'NONE',  ( 15.03925126672132961, 0.4576450603546987628, 5.200000000000000178 ) ) ;
#23316 = EDGE_CURVE ( 'NONE', #5946, #26529, #28505, .T. ) ;
#23317 = CARTESIAN_POINT ( 'NONE',  ( -57.64405989232413674, -3.920666489018320690E-15, 3.399999999999794298 ) ) ;
#23318 = EDGE_LOOP ( 'NONE', ( #17579, #29752, #4672, #25980 ) ) ;
#23319 = VERTEX_POINT ( 'NONE', #16930 ) ;
#23320 = VERTEX_POINT ( 'NONE', #145 ) ;
#23321 = CARTESIAN_POINT ( 'NONE',  ( -58.06249999999997158, 3.925981830489463142, -1.919074514008873212E-13 ) ) ;
#23322 = CARTESIAN_POINT ( 'NONE',  ( -54.86505354137801760, 3.400000000000011458, -0.9110272542659999528 ) ) ;
#23323 = CARTESIAN_POINT ( 'NONE',  ( 26.87602198329691916, 5.247164978609347052, -1.425000000000093747 ) ) ;
#23324 = CARTESIAN_POINT ( 'NONE',  ( 51.50000000000002132, 1.163569835200988601E-28, -1.798112889504214751E-13 ) ) ;
#23325 = TOROIDAL_SURFACE ( 'NONE', #13696, 1.975000000000001865, 0.1000000000000000056 ) ;
#23326 = DIRECTION ( 'NONE',  ( 1.282749433769087582E-30, 1.000000000000000000, 1.224646799147353207E-16 ) ) ;
#23327 = B_SPLINE_CURVE_WITH_KNOTS ( 'NONE', 3,
 ( #24418, #21767, #2728, #19063 ),
 .UNSPECIFIED., .F., .F.,
 ( 4, 4 ),
 ( 0.000000000000000000, 0.0002896601805182694557 ),
 .UNSPECIFIED. ) ;
#23328 = EDGE_CURVE ( 'NONE', #6022, #4064, #4678, .T. ) ;
#23330 = CARTESIAN_POINT ( 'NONE',  ( -71.44781903063172024, 0.2962147058074188766, -1.444404304980887455 ) ) ;
#23329 = CARTESIAN_POINT ( 'NONE',  ( -44.49999999999996447, 1.400000000000021450, -3.363870538531645416 ) ) ;
#23331 = B_SPLINE_CURVE_WITH_KNOTS ( 'NONE', 3,
 ( #22693, #1132, #988, #1439, #3974, #10640, #13614, #8413, #29948, #1275, #20630, #8565, #18248, #30406, #8256, #6199 ),
 .UNSPECIFIED., .F., .F.,
 ( 4, 3, 3, 3, 3, 4 ),
 ( -2.177409780393270631E-06, 0.000000000000000000, 1.647199373531996907E-05, 5.453032561112638088E-05, 8.914430023005323329E-05, 0.0001239676331529264105 ),
 .UNSPECIFIED. ) ;
#23332 = DIRECTION ( 'NONE',  ( 1.000000000000000000, -1.219044193948983948E-29, 3.491481338843133355E-15 ) ) ;
#23333 = CARTESIAN_POINT ( 'NONE',  ( -59.64819772016205235, 2.360117159334230053, -1.232121303804335488 ) ) ;
#23334 = CARTESIAN_POINT ( 'NONE',  ( 58.74154451056422488, -1.575232816092377197, -1.017012227664425117 ) ) ;
#23335 = DIRECTION ( 'NONE',  ( 3.002035892788117459E-16, -0.9996898646859343485, -0.02490330187381124133 ) ) ;
#23336 = CARTESIAN_POINT ( 'NONE',  ( 53.91574522233626965, 6.672251602764244893, -1.774295313897662485 ) ) ;
#23337 = ORIENTED_EDGE ( 'NONE', *, *, #14704, .F. ) ;
#23339 = LINE ( 'NONE', #17962, #8026 ) ;
#23338 = CARTESIAN_POINT ( 'NONE',  ( 68.00000000000007105, 1.401298464324817071E-42, 3.499999999999288569 ) ) ;
#23340 = EDGE_CURVE ( 'NONE', #7928, #16870, #5239, .T. ) ;
#23341 = SURFACE_STYLE_FILL_AREA ( #25708 ) ;
#23342 = ORIENTED_EDGE ( 'NONE', *, *, #8474, .F. ) ;
#23343 = CARTESIAN_POINT ( 'NONE',  ( 50.25000000000000711, 1.323060376181943720, -1.499837071477343242 ) ) ;
#23345 = CARTESIAN_POINT ( 'NONE',  ( 57.05000000000001137, -0.7500000000000000000, -1.746008434843730583 ) ) ;
#23344 = CARTESIAN_POINT ( 'NONE',  ( -60.74999999999997158, -2.944486372867089141, 1.699999999999773248 ) ) ;
#23346 = ORIENTED_EDGE ( 'NONE', *, *, #4617, .T. ) ;
#23347 = ORIENTED_EDGE ( 'NONE', *, *, #29207, .F. ) ;
#23348 = CARTESIAN_POINT ( 'NONE',  ( 51.67698846994527173, -4.134673935618214280, -2.019140663350203369 ) ) ;
#23349 = ORIENTED_EDGE ( 'NONE', *, *, #15574, .F. ) ;
#23350 = CARTESIAN_POINT ( 'NONE',  ( 51.34893360928145256, 1.002183861493406436, -1.396106892655430975 ) ) ;
#23351 = AXIS2_PLACEMENT_3D ( 'NONE', #25447, #8661, #8516 ) ;
#23352 = EDGE_CURVE ( 'NONE', #9147, #468, #10237, .T. ) ;
#23353 = CARTESIAN_POINT ( 'NONE',  ( -61.12499999999996447, 1.184343223768589803, 3.558065644182725862 ) ) ;
#23354 = EDGE_LOOP ( 'NONE', ( #22363, #5989, #30416, #22695 ) ) ;
#23355 = CARTESIAN_POINT ( 'NONE',  ( 24.21299357973748201, 5.692280404210901423, -2.050000000000084199 ) ) ;
#23356 = EDGE_CURVE ( 'NONE', #19192, #2931, #14844, .T. ) ;
#23357 = CARTESIAN_POINT ( 'NONE',  ( -44.59999999999998721, -1.514093959731547478, 3.183260039818173404 ) ) ;
#23358 = EDGE_CURVE ( 'NONE', #24179, #17195, #1130, .T. ) ;
#23359 = CARTESIAN_POINT ( 'NONE',  ( -54.48232515324713177, -2.803024266087990934, -2.239002676711937312 ) ) ;
#23360 = ORIENTED_EDGE ( 'NONE', *, *, #27663, .F. ) ;
#23361 = VERTEX_POINT ( 'NONE', #11498 ) ;
#23362 = FACE_OUTER_BOUND ( 'NONE', #16189, .T. ) ;
#23363 = CARTESIAN_POINT ( 'NONE',  ( -55.43749999999997868, -3.399999999999991473, -2.094585006122325661E-13 ) ) ;
#23364 = CARTESIAN_POINT ( 'NONE',  ( 61.25000000000001421, 1.000000000000641709, -1.586072192556190474 ) ) ;
#23365 = CARTESIAN_POINT ( 'NONE',  ( -59.41132486540517021, 2.413993528760422613, 1.250136525132548027 ) ) ;
#23366 = CARTESIAN_POINT ( 'NONE',  ( 58.75000018595669360, 1.404395290252203665, 1.333791840694332320 ) ) ;
#23367 = EDGE_CURVE ( 'NONE', #29967, #30656, #24901, .T. ) ;
#23368 = CARTESIAN_POINT ( 'NONE',  ( 15.03925126672132961, -0.9159215771349724644, -4.311190327366005270 ) ) ;
#23369 = DIRECTION ( 'NONE',  ( 0.000000000000000000, 0.000000000000000000, 1.000000000000000000 ) ) ;
#23371 = CARTESIAN_POINT ( 'NONE',  ( 51.67614500439950831, -4.149773407329040431, 1.728861777175572101 ) ) ;
#23370 = CARTESIAN_POINT ( 'NONE',  ( -36.50489844130401451, -2.884962146574324926, 4.577321775072974219 ) ) ;
#23372 = CARTESIAN_POINT ( 'NONE',  ( -59.68966108275621707, -2.222588089596432059, 1.532842483073527884 ) ) ;
#23373 = AXIS2_PLACEMENT_3D ( 'NONE', #14474, #17026, #24146 ) ;
#23374 = DIRECTION ( 'NONE',  ( -1.000000000000000000, -0.000000000000000000, -0.000000000000000000 ) ) ;
#23375 = DIRECTION ( 'NONE',  ( -0.9993908270190957621, 0.03489949670250100389, 3.491481338843133355E-15 ) ) ;
#23376 = VERTEX_POINT ( 'NONE', #21479 ) ;
#23377 = EDGE_CURVE ( 'NONE', #15671, #2569, #6589, .T. ) ;
#23378 = ORIENTED_EDGE ( 'NONE', *, *, #11433, .T. ) ;
#23379 = CARTESIAN_POINT ( 'NONE',  ( -43.84599839145305111, -8.171597657156649598E-15, 0.000000000000000000 ) ) ;
#23380 = ORIENTED_EDGE ( 'NONE', *, *, #30832, .T. ) ;
#23381 = ADVANCED_FACE ( 'NONE', ( #10737 ), #4357, .F. ) ;
#23382 = CARTESIAN_POINT ( 'NONE',  ( 54.23473434925104897, 6.620089622897159742, 2.049999999999810640 ) ) ;
#23383 = CARTESIAN_POINT ( 'NONE',  ( -55.65835481156724285, 4.108500314926515351, -1.367561758111408343 ) ) ;
#23385 = CARTESIAN_POINT ( 'NONE',  ( -36.89017861347080185, 3.436881753486414670, 4.177093996075273097 ) ) ;
#23384 = CARTESIAN_POINT ( 'NONE',  ( 60.82166330297945223, -0.6500000603358897511, 1.489337074527665505 ) ) ;
#23386 = ORIENTED_EDGE ( 'NONE', *, *, #19161, .F. ) ;
#23387 = ORIENTED_EDGE ( 'NONE', *, *, #23526, .T. ) ;
#23388 = DIRECTION ( 'NONE',  ( 0.000000000000000000, -0.9996898646859344595, -0.02490330187381124480 ) ) ;
#23389 = VERTEX_POINT ( 'NONE', #30808 ) ;
#23390 = DIRECTION ( 'NONE',  ( -1.000000000000000000, -3.054025858079668409E-16, 2.042474015755241579E-16 ) ) ;
#23391 = ORIENTED_EDGE ( 'NONE', *, *, #27633, .T. ) ;
#23393 = CARTESIAN_POINT ( 'NONE',  ( -54.49999999999999289, -1.433333333333339343, 4.054078878802656938 ) ) ;
#23392 = DIRECTION ( 'NONE',  ( 0.000000000000000000, 0.000000000000000000, 1.000000000000000000 ) ) ;
#23394 = CARTESIAN_POINT ( 'NONE',  ( -56.08155989232414385, -1.962990915244736678, 3.399999999999788969 ) ) ;
#23395 = ADVANCED_FACE ( 'NONE', ( #1823 ), #21177, .T. ) ;
#23396 = VERTEX_POINT ( 'NONE', #26215 ) ;
#23397 = CARTESIAN_POINT ( 'NONE',  ( -36.80043232705879319, 4.951626736499065373, -2.174059107776711297 ) ) ;
#23398 = EDGE_CURVE ( 'NONE', #16762, #24288, #7702, .T. ) ;
#23399 = FACE_OUTER_BOUND ( 'NONE', #3875, .T. ) ;
#23400 = CARTESIAN_POINT ( 'NONE',  ( 47.27530108852192114, -4.265589706924724389, 1.723997649431065149 ) ) ;
#23401 = CARTESIAN_POINT ( 'NONE',  ( 57.00000000000001421, 0.6820512820512794061, 1.773360101234991326 ) ) ;
#23402 = CARTESIAN_POINT ( 'NONE',  ( -58.13452994616202574, 2.093608279459371404E-14, -3.600000000000206146 ) ) ;
#23403 =( BOUNDED_CURVE ( )  B_SPLINE_CURVE ( 3, ( #28957, #16934, #26578, #2048 ),
 .UNSPECIFIED., .F., .T. ) 
 B_SPLINE_CURVE_WITH_KNOTS ( ( 4, 4 ),
 ( 5.204828459469180935, 5.421579857342605280 ),
 .UNSPECIFIED. ) 
 CURVE ( )  GEOMETRIC_REPRESENTATION_ITEM ( )  RATIONAL_B_SPLINE_CURVE ( ( 1.000000000000000000, 0.9960887331235708242, 0.9960887331235708242, 1.000000000000000000 ) ) 
 REPRESENTATION_ITEM ( '' )  );
#23404 = DIRECTION ( 'NONE',  ( 0.000000000000000000, 2.818925648462304271E-14, 1.000000000000000000 ) ) ;
#23405 = VECTOR ( 'NONE', #14991, 1000.000000000000000 ) ;
#23406 = CARTESIAN_POINT ( 'NONE',  ( -59.29999999999997584, -2.208048483361063852, 2.585444235547710967 ) ) ;
#23407 = DIRECTION ( 'NONE',  ( 1.015447888376667464E-14, 0.000000000000000000, 1.000000000000000000 ) ) ;
#23408 = ORIENTED_EDGE ( 'NONE', *, *, #3991, .F. ) ;
#23409 = DIRECTION ( 'NONE',  ( -1.000000000000000000, 0.000000000000000000, 0.000000000000000000 ) ) ;
#23410 = EDGE_CURVE ( 'NONE', #26766, #10675, #26047, .T. ) ;
#23411 = CARTESIAN_POINT ( 'NONE',  ( 61.00000000000002842, -0.8666666666660278739, -1.374595900215364708 ) ) ;
#23412 = CARTESIAN_POINT ( 'NONE',  ( 53.30600611140961576, 4.975802279707719045, 1.612825013952412956 ) ) ;
#23413 = DIRECTION ( 'NONE',  ( 1.282749433769087582E-30, 1.000000000000000000, 1.224646799147353207E-16 ) ) ;
#23414 = EDGE_CURVE ( 'NONE', #8262, #20483, #16837, .T. ) ;
#23415 = ORIENTED_EDGE ( 'NONE', *, *, #5495, .F. ) ;
#23416 = CARTESIAN_POINT ( 'NONE',  ( -57.06249999999997868, -1.962990915244744006, 3.399999999999782307 ) ) ;
#23417 = EDGE_LOOP ( 'NONE', ( #2848, #2701, #11144, #16913 ) ) ;
#23418 = ADVANCED_FACE ( 'NONE', ( #31112 ), #11246, .T. ) ;
#23419 = LINE ( 'NONE', #20744, #18791 ) ;
#23421 = CARTESIAN_POINT ( 'NONE',  ( 58.66122797211808404, -1.337438849764076121, 1.314214529126705777 ) ) ;
#23420 = DIRECTION ( 'NONE',  ( 0.000000000000000000, -0.9996898646859343485, -0.02490330187381123786 ) ) ;
#23422 = ORIENTED_EDGE ( 'NONE', *, *, #26274, .T. ) ;
#23423 = CARTESIAN_POINT ( 'NONE',  ( -59.31908585006426904, -2.449738638601608010, -1.018617722459757458 ) ) ;
#23424 = LINE ( 'NONE', #6636, #9601 ) ;
#23426 = CARTESIAN_POINT ( 'NONE',  ( 58.65263613458537151, 0.9947326234272455547, 1.589467873455418845 ) ) ;
#23425 = FACE_OUTER_BOUND ( 'NONE', #7791, .T. ) ;
#23427 = ORIENTED_EDGE ( 'NONE', *, *, #7889, .F. ) ;
#23428 = CARTESIAN_POINT ( 'NONE',  ( -60.48542740578360366, 0.7887156198831658527, -3.845940847736173840 ) ) ;
#23429 = VECTOR ( 'NONE', #18672, 1000.000000000000114 ) ;
#23430 = DIRECTION ( 'NONE',  ( 1.000000000000000000, -7.137062321648221502E-17, -7.924918191827128155E-17 ) ) ;
#23431 = APPLICATION_PROTOCOL_DEFINITION ( 'draft international standard', 'automotive_design', 1998, #24304 ) ;
#23432 = DIRECTION ( 'NONE',  ( 0.000000000000000000, -1.224646799147362821E-16, 1.000000000000000000 ) ) ;
#23433 = CARTESIAN_POINT ( 'NONE',  ( -67.99999999999997158, -3.266925685480240183E-16, 2.202315069465531314E-15 ) ) ;
#23434 = DIRECTION ( 'NONE',  ( 0.9480661539417378769, -0.3180732113053867383, -3.310155284476359054E-15 ) ) ;
#23435 = ORIENTED_EDGE ( 'NONE', *, *, #1502, .F. ) ;
#23436 = CARTESIAN_POINT ( 'NONE',  ( -57.12499999999997158, -3.673546848079173532, -0.7533615035078090605 ) ) ;
#23437 = CARTESIAN_POINT ( 'NONE',  ( -36.48821680285229974, 3.495540671458303716, -4.131527132740814956 ) ) ;
#23438 = CARTESIAN_POINT ( 'NONE',  ( 51.12687253673779253, 0.9194130538826112975, -1.491219977510798378 ) ) ;
#23439 = CARTESIAN_POINT ( 'NONE',  ( 49.05000000000005400, 1.401298464324817071E-42, 2.674999999999485123 ) ) ;
#23440 = CARTESIAN_POINT ( 'NONE',  ( 16.10667815269232506, 0.1434351685890397909, -5.407416993630365987 ) ) ;
#23441 = SPHERICAL_SURFACE ( 'NONE', #16963, 0.05000000000000000278 ) ;
#23442 = AXIS2_PLACEMENT_3D ( 'NONE', #20427, #8367, #22654 ) ;
#23443 = CARTESIAN_POINT ( 'NONE',  ( -62.09999999999998010, -2.687742116683883520, -0.2820114153134715140 ) ) ;
#23445 = LINE ( 'NONE', #1582, #18043 ) ;
#23444 = DIRECTION ( 'NONE',  ( -2.117927888850090838E-16, 0.02490330187381123786, -0.9996898646859343485 ) ) ;
#23446 = ADVANCED_FACE ( 'NONE', ( #16248 ), #30636, .T. ) ;
#23447 = ORIENTED_EDGE ( 'NONE', *, *, #13638, .T. ) ;
#23448 = LINE ( 'NONE', #1915, #12398 ) ;
#23449 = DIRECTION ( 'NONE',  ( 0.000000000000000000, 0.9996898646859344595, 0.02490330187381124133 ) ) ;
#23451 = DIRECTION ( 'NONE',  ( -1.000000000000000000, 0.000000000000000000, 0.000000000000000000 ) ) ;
#23450 = CARTESIAN_POINT ( 'NONE',  ( 58.66122797211864537, 1.806862593129175965, 0.5011487553415301388 ) ) ;
#23452 = EDGE_LOOP ( 'NONE', ( #13542, #20093, #521, #13695 ) ) ;
#23453 = EDGE_LOOP ( 'NONE', ( #6966, #19248, #18134, #7007 ) ) ;
#23454 = CARTESIAN_POINT ( 'NONE',  ( 48.33022520384532328, 1.142230555601122965, 3.938343097974785767 ) ) ;
#23455 = CYLINDRICAL_SURFACE ( 'NONE', #6265, 0.1000000000000000472 ) ;
#23456 = EDGE_LOOP ( 'NONE', ( #10707, #2073, #28155, #30514 ) ) ;
#23457 = DIRECTION ( 'NONE',  ( -1.047444401652940007E-14, 0.000000000000000000, -1.000000000000000000 ) ) ;
#23458 = VERTEX_POINT ( 'NONE', #16094 ) ;
#23459 = DIRECTION ( 'NONE',  ( -1.000000000000000000, 0.000000000000000000, 0.000000000000000000 ) ) ;
#23460 = ORIENTED_EDGE ( 'NONE', *, *, #18885, .T. ) ;
#23461 = CARTESIAN_POINT ( 'NONE',  ( -55.38452994616205416, -3.117691453623978148, 1.799999999999789102 ) ) ;
#23462 = ADVANCED_FACE ( 'NONE', ( #20421 ), #30045, .T. ) ;
#23463 = CARTESIAN_POINT ( 'NONE',  ( -58.14405989232411542, -2.944486372867076263, -1.700000000000216893 ) ) ;
#23464 = ORIENTED_EDGE ( 'NONE', *, *, #25702, .T. ) ;
#23465 = VERTEX_POINT ( 'NONE', #28109 ) ;
#23466 = CIRCLE ( 'NONE', #9813, 0.1500000000000001887 ) ;
#23467 = EDGE_LOOP ( 'NONE', ( #17043, #21740, #11806, #25627 ) ) ;
#23468 = CARTESIAN_POINT ( 'NONE',  ( -55.94702994616203995, -2.078460969082631227, -3.600000000000205258 ) ) ;
#23469 = DIRECTION ( 'NONE',  ( 0.000000000000000000, 0.000000000000000000, 1.000000000000000000 ) ) ;
#23470 = DIRECTION ( 'NONE',  ( 1.000000000000000000, -0.000000000000000000, 0.000000000000000000 ) ) ;
#23471 = DIRECTION ( 'NONE',  ( 1.000000000000000000, 0.000000000000000000, -1.047444401652940007E-14 ) ) ;
#23472 = CIRCLE ( 'NONE', #9826, 1.375000000000001332 ) ;
#23473 = CARTESIAN_POINT ( 'NONE',  ( -54.49999999999997158, -0.6998428355231358644, -3.385667905176602321 ) ) ;
#23475 = DIRECTION ( 'NONE',  ( -1.000000000000000000, 1.219044193948983948E-29, -3.491481338843133355E-15 ) ) ;
#23474 = DIRECTION ( 'NONE',  ( 0.000000000000000000, 0.000000000000000000, -1.000000000000000000 ) ) ;
#23476 = CIRCLE ( 'NONE', #4259, 2.549999999999999822 ) ;
#23477 = DIRECTION ( 'NONE',  ( 0.9991330730923518866, -0.04161763361012198875, -0.001036738022138846901 ) ) ;
#23478 = CARTESIAN_POINT ( 'NONE',  ( 15.98305126557416500, 5.283830060792412020, -1.151642405604206720 ) ) ;
#23479 = EDGE_CURVE ( 'NONE', #20434, #15271, #30010, .T. ) ;
#23480 = CARTESIAN_POINT ( 'NONE',  ( 58.74999999999981526, -1.671477153793549331, -0.8495817349403145258 ) ) ;
#23481 = FACE_OUTER_BOUND ( 'NONE', #28447, .T. ) ;
#23482 = CARTESIAN_POINT ( 'NONE',  ( 50.30000000000001847, 1.391941090707534023, -3.850000000000022737 ) ) ;
#23483 = ORIENTED_EDGE ( 'NONE', *, *, #8840, .F. ) ;
#23484 = EDGE_CURVE ( 'NONE', #20201, #4847, #6692, .T. ) ;
#23486 = CARTESIAN_POINT ( 'NONE',  ( 63.50000000000000000, -0.7500000000000000000, -1.988246715074021731 ) ) ;
#23485 = CARTESIAN_POINT ( 'NONE',  ( 51.38214458811558671, -1.084857585945107505, -1.209959298770751923 ) ) ;
#23487 = DIRECTION ( 'NONE',  ( -3.491481338843133355E-15, 0.000000000000000000, -1.000000000000000000 ) ) ;
#23488 = ORIENTED_EDGE ( 'NONE', *, *, #17984, .T. ) ;
#23489 = LINE ( 'NONE', #21145, #730 ) ;
#23490 = DIRECTION ( 'NONE',  ( 0.000000000000000000, 0.000000000000000000, -1.000000000000000000 ) ) ;
#23491 = CARTESIAN_POINT ( 'NONE',  ( -54.63452994616206126, -3.117691453623976816, 1.799999999999793765 ) ) ;
#23492 = EDGE_LOOP ( 'NONE', ( #12505, #11195, #26222, #5331 ) ) ;
#23493 = ORIENTED_EDGE ( 'NONE', *, *, #7165, .T. ) ;
#23494 = CYLINDRICAL_SURFACE ( 'NONE', #20497, 3.750000000000000444 ) ;
#23495 = ORIENTED_EDGE ( 'NONE', *, *, #2062, .F. ) ;
#23496 = DIRECTION ( 'NONE',  ( -1.000000000000000000, -1.047444401652940007E-14, -0.000000000000000000 ) ) ;
#23497 = EDGE_CURVE ( 'NONE', #24203, #1635, #23906, .T. ) ;
#23498 = FACE_OUTER_BOUND ( 'NONE', #5868, .T. ) ;
#23499 = EDGE_LOOP ( 'NONE', ( #12803, #23525, #14758, #21779 ) ) ;
#23500 = DIRECTION ( 'NONE',  ( 0.000000000000000000, -0.9996898646859343485, -0.02490330187381143562 ) ) ;
#23501 = CARTESIAN_POINT ( 'NONE',  ( 67.95000000000003126, -1.025519176787267142E-28, -7.117384709231726808E-13 ) ) ;
#23502 = AXIS2_PLACEMENT_3D ( 'NONE', #3548, #18273, #25698 ) ;
#23503 = LINE ( 'NONE', #11476, #9117 ) ;
#23504 = EDGE_LOOP ( 'NONE', ( #21344, #30461 ) ) ;
#23505 = ORIENTED_EDGE ( 'NONE', *, *, #24867, .F. ) ;
#23506 = FACE_OUTER_BOUND ( 'NONE', #24466, .T. ) ;
#23507 = CARTESIAN_POINT ( 'NONE',  ( 50.30000000000001847, -1.426739617975173013, -3.843750000000023093 ) ) ;
#23509 = CARTESIAN_POINT ( 'NONE',  ( 60.88479802533563401, 0.5000000000006354917, -1.718465885608769339 ) ) ;
#23508 = TOROIDAL_SURFACE ( 'NONE', #9858, 0.3000000000000000444, 0.05000000000000000278 ) ;
#23510 = EDGE_LOOP ( 'NONE', ( #21218, #7249, #25302, #26176 ) ) ;
#23511 = EDGE_CURVE ( 'NONE', #5493, #16551, #10202, .T. ) ;
#23512 = CARTESIAN_POINT ( 'NONE',  ( -59.69999999999997442, 8.366749974758454467E-15, -2.120534355533670266E-13 ) ) ;
#23513 = DIRECTION ( 'NONE',  ( 0.000000000000000000, 0.000000000000000000, -1.000000000000000000 ) ) ;
#23514 = AXIS2_PLACEMENT_3D ( 'NONE', #18724, #16820, #9052 ) ;
#23515 = CARTESIAN_POINT ( 'NONE',  ( -54.39999999999996305, 1.400000000000023892, -3.959797974644871932 ) ) ;
#23517 = CARTESIAN_POINT ( 'NONE',  ( 58.72204580543434105, -0.9179489429356002539, 1.635081356932753804 ) ) ;
#23516 = CARTESIAN_POINT ( 'NONE',  ( 58.73309930451018346, -0.5681566835778693036, -1.786899855579580310 ) ) ;
#23518 = PRODUCT ( 'Cap Ring', 'Cap Ring', '', ( #1417 ) ) ;
#23519 = CARTESIAN_POINT ( 'NONE',  ( -67.99999999999995737, -3.266925685480207642E-16, 2.202315069465528948E-15 ) ) ;
#23520 = CARTESIAN_POINT ( 'NONE',  ( 51.50000000000002842, 1.163569835200988601E-28, 1.624999999999821920 ) ) ;
#23521 = EDGE_CURVE ( 'NONE', #1478, #30797, #22893, .T. ) ;
#23522 = DIRECTION ( 'NONE',  ( 0.000000000000000000, 0.000000000000000000, -1.000000000000000000 ) ) ;
#23523 = CARTESIAN_POINT ( 'NONE',  ( 63.50000000000004263, 0.8382352941176473005, 2.222158093316616068 ) ) ;
#23524 = EDGE_CURVE ( 'NONE', #4648, #27829, #10264, .T. ) ;
#23525 = ORIENTED_EDGE ( 'NONE', *, *, #3407, .F. ) ;
#23526 = EDGE_CURVE ( 'NONE', #25236, #9362, #12783, .T. ) ;
#23527 = AXIS2_PLACEMENT_3D ( 'NONE', #30249, #15219, #24866 ) ;
#23528 = ORIENTED_EDGE ( 'NONE', *, *, #22485, .F. ) ;
#23529 = VECTOR ( 'NONE', #10674, 1000.000000000000000 ) ;
#23530 = VERTEX_POINT ( 'NONE', #4825 ) ;
#23531 = DIRECTION ( 'NONE',  ( 1.000000000000000000, 1.047444401652940007E-14, 0.000000000000000000 ) ) ;
#23532 = ORIENTED_EDGE ( 'NONE', *, *, #13244, .F. ) ;
#23533 = CARTESIAN_POINT ( 'NONE',  ( 51.80000000000003268, 8.600000000000104450, 2.049999999999819522 ) ) ;
#23534 = CARTESIAN_POINT ( 'NONE',  ( -58.78335481156723574, 0.8699069336946689823, -4.241846523238430144 ) ) ;
#23536 = CARTESIAN_POINT ( 'NONE',  ( -36.27260443516980359, 3.212533369474494638, 4.093511368021819585 ) ) ;
#23535 = CARTESIAN_POINT ( 'NONE',  ( 58.75000000000000000, 1.996089927834530542, -0.1249999999989956784 ) ) ;
#23537 = VERTEX_POINT ( 'NONE', #12264 ) ;
#23538 = DIRECTION ( 'NONE',  ( 1.000000000000000000, -0.000000000000000000, -0.000000000000000000 ) ) ;
#23539 = ORIENTED_EDGE ( 'NONE', *, *, #11641, .T. ) ;
#23540 = CIRCLE ( 'NONE', #26584, 4.100000000000022737 ) ;
#23541 = CARTESIAN_POINT ( 'NONE',  ( -54.39999999999996305, 1.433333333333357329, -4.054078878803077934 ) ) ;
#23542 = EDGE_CURVE ( 'NONE', #5737, #7647, #5702, .T. ) ;
#23543 = ORIENTED_EDGE ( 'NONE', *, *, #21802, .T. ) ;
#23545 = DIRECTION ( 'NONE',  ( 1.000000000000000000, 3.385297212316258532E-16, -2.459562394685744279E-16 ) ) ;
#23544 = CARTESIAN_POINT ( 'NONE',  ( 22.06071280439819660, 8.185410187602871090, -1.950000000000076339 ) ) ;
#23546 = AXIS2_PLACEMENT_3D ( 'NONE', #11150, #26021, #1075 ) ;
#23547 = ORIENTED_EDGE ( 'NONE', *, *, #12096, .T. ) ;
#23548 = CARTESIAN_POINT ( 'NONE',  ( 53.45668161578581845, 7.806773462440032674, 1.876589663053878088 ) ) ;
#23549 = B_SPLINE_CURVE_WITH_KNOTS ( 'NONE', 3,
 ( #9040, #2068, #11882, #9358 ),
 .UNSPECIFIED., .F., .F.,
 ( 4, 4 ),
 ( 0.000000000000000000, 1.000000000000000000 ),
 .UNSPECIFIED. ) ;
#23550 = CARTESIAN_POINT ( 'NONE',  ( 58.74154451056406856, 1.832994048939196263, -0.3947215634740703916 ) ) ;
#23551 = CARTESIAN_POINT ( 'NONE',  ( 68.04999999999998295, 1.401298464324817071E-42, -4.000000000000713207 ) ) ;
#23552 = CARTESIAN_POINT ( 'NONE',  ( 57.05000000000001847, 0.7500000000000000000, 1.778341924377873751 ) ) ;
#23553 = CARTESIAN_POINT ( 'NONE',  ( -58.19702994616203284, -2.078460969082631227, -3.600000000000212363 ) ) ;
#23554 = AXIS2_PLACEMENT_3D ( 'NONE', #22784, #1073, #7721 ) ;
#23555 = ADVANCED_FACE ( 'NONE', ( #546 ), #31268, .T. ) ;
#23556 = CARTESIAN_POINT ( 'NONE',  ( 51.86040321072245263, 0.1224230307917539146, 4.365444804395989919 ) ) ;
#23557 = CIRCLE ( 'NONE', #291, 4.275000000000000355 ) ;
#23558 = CIRCLE ( 'NONE', #11431, 1.625000000000001332 ) ;
#23559 = CARTESIAN_POINT ( 'NONE',  ( 33.47623932017462778, 4.375000000000001776, 5.948056943527305374E-16 ) ) ;
#23560 = CARTESIAN_POINT ( 'NONE',  ( 41.48619405472010158, -151.3359592902261852, -1.425000000000163691 ) ) ;
#23561 = AXIS2_PLACEMENT_3D ( 'NONE', #27950, #1653, #28273 ) ;
#23562 = TOROIDAL_SURFACE ( 'NONE', #29120, 2.424999999999998934, 0.05000000000000000278 ) ;
#23563 = CARTESIAN_POINT ( 'NONE',  ( -56.04792740578360366, -1.073804522883513579, -3.225979517392337126 ) ) ;
#23564 = EDGE_CURVE ( 'NONE', #28412, #7544, #7728, .T. ) ;
#23565 = CARTESIAN_POINT ( 'NONE',  ( -55.58155989232413674, 3.400000000000007461, -1.857527951337884861E-13 ) ) ;
#23566 = ADVANCED_FACE ( 'NONE', ( #30263 ), #17231, .F. ) ;
#23567 = VERTEX_POINT ( 'NONE', #13769 ) ;
#23568 = EDGE_CURVE ( 'NONE', #3768, #8968, #28464, .T. ) ;
#23569 = DIRECTION ( 'NONE',  ( -1.000000000000000000, 0.000000000000000000, 3.491481338843133355E-15 ) ) ;
#23570 = DIRECTION ( 'NONE',  ( 0.000000000000000000, 5.942513678379226626E-16, 1.000000000000000000 ) ) ;
#23571 = CARTESIAN_POINT ( 'NONE',  ( -36.92362342067168868, 0.1627367787822124878, 5.407318510437578496 ) ) ;
#23572 = DIRECTION ( 'NONE',  ( 1.000000000000000000, 0.000000000000000000, -3.491481338843133355E-15 ) ) ;
#23573 = ORIENTED_EDGE ( 'NONE', *, *, #8280, .F. ) ;
#23574 = AXIS2_PLACEMENT_3D ( 'NONE', #26090, #4403, #23734 ) ;
#23575 = CARTESIAN_POINT ( 'NONE',  ( 47.00000000000002132, 2.428612866367529932E-14, -4.100000000000022737 ) ) ;
#23576 = ORIENTED_EDGE ( 'NONE', *, *, #19781, .T. ) ;
#23578 = CARTESIAN_POINT ( 'NONE',  ( 58.75000018595672913, -1.333791840694231956, 1.404395290251547079 ) ) ;
#23577 = DIRECTION ( 'NONE',  ( -3.491481338843133355E-15, 0.000000000000000000, -1.000000000000000000 ) ) ;
#23579 = EDGE_LOOP ( 'NONE', ( #12607, #19946, #21521, #28789 ) ) ;
#23580 = VECTOR ( 'NONE', #7491, 1000.000000000000000 ) ;
#23581 = EDGE_LOOP ( 'NONE', ( #4066, #3766, #20682, #1339, #6819, #5152, #2152, #30516, #3405, #10132 ) ) ;
#23582 = CARTESIAN_POINT ( 'NONE',  ( -59.51761855918061883, -2.467398989037727031, -1.133240635510040173 ) ) ;
#23583 = DIRECTION ( 'NONE',  ( 0.000000000000000000, 0.000000000000000000, -1.000000000000000000 ) ) ;
#23584 = AXIS2_PLACEMENT_3D ( 'NONE', #11916, #9074, #11275 ) ;
#23586 = CARTESIAN_POINT ( 'NONE',  ( -44.59999999999997300, -3.524999999999988365, -1.993951146718866637E-13 ) ) ;
#23585 = DIRECTION ( 'NONE',  ( 0.000000000000000000, 0.000000000000000000, 1.000000000000000000 ) ) ;
#23587 = ORIENTED_EDGE ( 'NONE', *, *, #19270, .T. ) ;
#23588 = CARTESIAN_POINT ( 'NONE',  ( -60.67292740578359656, -3.330682475591783653, -0.6830477631804101613 ) ) ;
#23589 = DIRECTION ( 'NONE',  ( -1.000000000000000000, 0.000000000000000000, 1.047444401652940007E-14 ) ) ;
#23590 = SHAPE_DEFINITION_REPRESENTATION ( #7112, #29923 ) ;
#23591 = AXIS2_PLACEMENT_3D ( 'NONE', #2167, #28782, #7239 ) ;
#23592 = TOROIDAL_SURFACE ( 'NONE', #30148, -24.59258869922086888, 30.00000000000000000 ) ;
#23593 = CARTESIAN_POINT ( 'NONE',  ( 50.55258015808398397, 0.05185913279273118848, -1.177580158083963324 ) ) ;
#23594 =( BOUNDED_SURFACE ( )  B_SPLINE_SURFACE ( 3, 2, ( 
 ( #200, #7782, #10031 ),
 ( #27265, #659, #29468 ),
 ( #17003, #5583, #17302 ),
 ( #2888, #19537, #10319 ),
 ( #3194, #9862, #19988 ),
 ( #17452, #7955, #24878 ),
 ( #24422, #7332, #29183 ),
 ( #5421, #12836, #2732 ),
 ( #58, #12377, #27101 ),
 ( #362, #19380, #19696 ) ),
 .UNSPECIFIED., .F., .F., .F. ) 
 B_SPLINE_SURFACE_WITH_KNOTS ( ( 4, 2, 2, 2, 4 ),
 ( 3, 3 ),
 ( -4.878909776184769953E-18, 0.0003534454412679785659, 0.0007068908825359620108, 0.001060336323803945293, 0.001413781765071928792 ),
 ( 0.000000000000000000, 1.000000000000000000 ),
 .UNSPECIFIED. ) 
 GEOMETRIC_REPRESENTATION_ITEM ( )  RATIONAL_B_SPLINE_SURFACE ( (
 ( 1.000000000000000000, 0.6992058987801026415, 1.000000000000000000),
 ( 1.000000000000000000, 0.6992660572539753927, 1.000000000000000000),
 ( 1.000000000000000000, 0.6974033530214182042, 1.000000000000000000),
 ( 1.000000000000000000, 0.6920435876590419477, 1.000000000000000000),
 ( 1.000000000000000000, 0.6885661196048414867, 1.000000000000000000),
 ( 1.000000000000000000, 0.6845372766838363487, 1.000000000000000000),
 ( 1.000000000000000000, 0.6841195446900723010, 1.000000000000000000),
 ( 1.000000000000000000, 0.6902705495933709745, 1.000000000000000000),
 ( 1.000000000000000000, 0.6968978290759786365, 1.000000000000000000),
 ( 1.000000000000000000, 0.7071067811865482389, 1.000000000000000000) ) ) 
 REPRESENTATION_ITEM ( '' )  SURFACE ( )  );
#23595 = DIRECTION ( 'NONE',  ( -1.000000000000000000, 0.000000000000000000, -0.000000000000000000 ) ) ;
#23596 = AXIS2_PLACEMENT_3D ( 'NONE', #364, #19698, #7957 ) ;
#23597 = FACE_OUTER_BOUND ( 'NONE', #22373, .T. ) ;
#23598 = EDGE_CURVE ( 'NONE', #21195, #16714, #9946, .T. ) ;
#23599 = ORIENTED_EDGE ( 'NONE', *, *, #6615, .F. ) ;
#23600 = CARTESIAN_POINT ( 'NONE',  ( -69.18535533905931345, 0.4248245016402701912, -2.071532327734947110 ) ) ;
#23601 = EDGE_CURVE ( 'NONE', #10142, #618, #26981, .T. ) ;
#23602 = AXIS2_PLACEMENT_3D ( 'NONE', #27758, #10970, #1462 ) ;
#23603 = CARTESIAN_POINT ( 'NONE',  ( -36.11692583559977976, 2.199885872770852124, -4.939696258129341544 ) ) ;
#23604 = CARTESIAN_POINT ( 'NONE',  ( 69.20000000000001705, 0.7500000000000000000, -1.988246715074081017 ) ) ;
#23605 = CARTESIAN_POINT ( 'NONE',  ( -59.19999999999997442, 8.366749974758448157E-15, -2.103076948839454410E-13 ) ) ;
#23606 = VECTOR ( 'NONE', #24187, 1000.000000000000000 ) ;
#23607 = AXIS2_PLACEMENT_3D ( 'NONE', #17888, #5847, #622 ) ;
#23608 = CARTESIAN_POINT ( 'NONE',  ( 57.00000000000001421, -0.6999999999999999556, -2.452039967047845437 ) ) ;
#23609 = CIRCLE ( 'NONE', #11991, 0.1500000000000001887 ) ;
#23610 = LINE ( 'NONE', #16468, #17470 ) ;
#23611 = AXIS2_PLACEMENT_3D ( 'NONE', #26173, #7488, #5101 ) ;
#23612 = EDGE_CURVE ( 'NONE', #3631, #30600, #12269, .T. ) ;
#23613 = CARTESIAN_POINT ( 'NONE',  ( 48.00000000000001421, -4.387164041431065087, -1.383037119376925528 ) ) ;
#23614 = AXIS2_PLACEMENT_3D ( 'NONE', #6984, #25960, #8852 ) ;
#23616 = CARTESIAN_POINT ( 'NONE',  ( 50.30000000000001847, -1.391941090707485396, -3.850000000000022737 ) ) ;
#23615 = DIRECTION ( 'NONE',  ( -1.000000000000000000, 0.000000000000000000, 8.673617379883787770E-15 ) ) ;
#23617 = EDGE_LOOP ( 'NONE', ( #920, #22827, #27117, #13469 ) ) ;
#23618 = CONICAL_SURFACE ( 'NONE', #27149, 2.099999999999999645, 0.7853981633974396193 ) ;
#23619 = CIRCLE ( 'NONE', #27651, 0.05000000000000012768 ) ;
#23620 = CARTESIAN_POINT ( 'NONE',  ( 48.00000000000001421, -4.031600731908413948, -1.173113608511841877 ) ) ;
#23622 = FACE_OUTER_BOUND ( 'NONE', #24081, .T. ) ;
#23621 = CARTESIAN_POINT ( 'NONE',  ( 58.65844932252355193, 1.802326573994337044, 0.5172264997599709258 ) ) ;
#23623 = CARTESIAN_POINT ( 'NONE',  ( 15.61552784268231520, -4.977698683490599407, 2.127480166903654268 ) ) ;
#23624 = ORIENTED_EDGE ( 'NONE', *, *, #19892, .T. ) ;
#23625 = VERTEX_POINT ( 'NONE', #11586 ) ;
#23626 = CARTESIAN_POINT ( 'NONE',  ( -36.30347965937279753, -4.910307320510546525, 1.715181477143133071 ) ) ;
#23627 = CARTESIAN_POINT ( 'NONE',  ( 47.05963571244990362, 8.266527678078146479, -2.050000000000163691 ) ) ;
#23628 = ORIENTED_EDGE ( 'NONE', *, *, #794, .F. ) ;
#23629 = CARTESIAN_POINT ( 'NONE',  ( 36.50000000000002132, -0.8000000000000000444, -1.778341924377873751 ) ) ;
#23630 = CIRCLE ( 'NONE', #14510, 0.2499999999999997780 ) ;
#23631 = ORIENTED_EDGE ( 'NONE', *, *, #25233, .F. ) ;
#23632 = DIRECTION ( 'NONE',  ( 1.000000000000000000, 3.054025858079668409E-16, -2.042474015755241579E-16 ) ) ;
#23633 = ORIENTED_EDGE ( 'NONE', *, *, #26592, .T. ) ;
#23634 = VECTOR ( 'NONE', #20858, 1000.000000000000000 ) ;
#23635 = CARTESIAN_POINT ( 'NONE',  ( 58.74999981404334903, -1.441842230225807819, -1.321446761053086449 ) ) ;
#23636 = VERTEX_POINT ( 'NONE', #24351 ) ;
#23637 = VECTOR ( 'NONE', #10785, 1000.000000000000114 ) ;
#23638 = EDGE_LOOP ( 'NONE', ( #30949, #9728, #26142, #28261 ) ) ;
#23639 = ADVANCED_FACE ( 'NONE', ( #21266 ), #9641, .T. ) ;
#23640 = VERTEX_POINT ( 'NONE', #17372 ) ;
#23641 = EDGE_CURVE ( 'NONE', #16210, #1060, #3278, .T. ) ;
#23642 = AXIS2_PLACEMENT_3D ( 'NONE', #14372, #14545, #12621 ) ;
#23643 = CARTESIAN_POINT ( 'NONE',  ( -61.24999999999995026, 2.023778652682512839E-14, -3.400000000000217515 ) ) ;
#23644 = CIRCLE ( 'NONE', #24141, 4.000000000000000000 ) ;
#23645 = ADVANCED_FACE ( 'NONE', ( #20397 ), #3595, .F. ) ;
#23646 = CIRCLE ( 'NONE', #3924, 2.136029617911934686 ) ;
#23647 = CARTESIAN_POINT ( 'NONE',  ( 57.00791613703923844, -0.8068646677135199452, 2.471635681327667644 ) ) ;
#23648 = CARTESIAN_POINT ( 'NONE',  ( 30.21341079104191607, 6.695592610073554773, -1.425000000000104849 ) ) ;
#23649 = CARTESIAN_POINT ( 'NONE',  ( -35.85663232820584767, 4.683225679163358635, -2.703237727951174563 ) ) ;
#23650 = DIRECTION ( 'NONE',  ( -1.000000000000000000, -1.047444401652940007E-14, -0.000000000000000000 ) ) ;
#23651 = B_SPLINE_CURVE_WITH_KNOTS ( 'NONE', 3,
 ( #64, #29189, #11775, #21450, #29028, #31080, #28729, #14300, #7337, #26342 ),
 .UNSPECIFIED., .F., .F.,
 ( 4, 2, 2, 2, 4 ),
 ( 8.673617379884035472E-19, 0.0003923434276460365509, 0.0007846868552920722344, 0.001177030282938107972, 0.001569373710584143601 ),
 .UNSPECIFIED. ) ;
#23653 = CARTESIAN_POINT ( 'NONE',  ( 57.05000000000001847, -0.8000000000000001554, -1.778341924377873973 ) ) ;
#23652 = CARTESIAN_POINT ( 'NONE',  ( -35.85663232820584057, 2.686240680702182804, -4.475885388010699018 ) ) ;
#23654 = AXIS2_PLACEMENT_3D ( 'NONE', #20405, #11043, #926 ) ;
#23655 = CIRCLE ( 'NONE', #5960, 4.275000000000000355 ) ;
#23656 = FILL_AREA_STYLE ('',( #28062 ) ) ;
#23657 = LINE ( 'NONE', #11609, #9932 ) ;
#23658 = CARTESIAN_POINT ( 'NONE',  ( 15.29384114148388818, 5.068511731019603062, -1.228278365481837220 ) ) ;
#23659 = EDGE_CURVE ( 'NONE', #21890, #23000, #2960, .T. ) ;
#23660 = CARTESIAN_POINT ( 'NONE',  ( 58.65000045311413857, -1.580645149930897109, -1.008695754909851416 ) ) ;
#23662 = CARTESIAN_POINT ( 'NONE',  ( 57.02184386277451722, 0.7500000000000000000, -2.421260326253384942 ) ) ;
#23661 = AXIS2_PLACEMENT_3D ( 'NONE', #10087, #19901, #574 ) ;
#23663 = CARTESIAN_POINT ( 'NONE',  ( 52.14970241235015891, 8.689026183520638824, 2.049999999999819078 ) ) ;
#23664 = VERTEX_POINT ( 'NONE', #12615 ) ;
#23666 = DIRECTION ( 'NONE',  ( 0.000000000000000000, -1.000000000000000000, -6.156016597943509841E-15 ) ) ;
#23665 = DIRECTION ( 'NONE',  ( 0.000000000000000000, 0.2008964009354148039, -0.9796124928211140670 ) ) ;
#23667 = CARTESIAN_POINT ( 'NONE',  ( 15.03925126672132961, -4.018128179617538542, -3.618665901676658248 ) ) ;
#23668 = ORIENTED_EDGE ( 'NONE', *, *, #27816, .F. ) ;
#23669 = DIRECTION ( 'NONE',  ( 1.000000000000000000, 3.053848253006669023E-16, -2.042510438544995415E-16 ) ) ;
#23670 = CYLINDRICAL_SURFACE ( 'NONE', #18368, 1.875000000000000000 ) ;
#23671 = CARTESIAN_POINT ( 'NONE',  ( -59.12499999999996447, -2.944486372867076707, -1.700000000000220446 ) ) ;
#23672 = ORIENTED_EDGE ( 'NONE', *, *, #22424, .F. ) ;
#23673 = VERTEX_POINT ( 'NONE', #1064 ) ;
#23674 = CARTESIAN_POINT ( 'NONE',  ( 15.76675455518196678, 5.174628573245020569, 1.572974725650792438 ) ) ;
#23675 = ORIENTED_EDGE ( 'NONE', *, *, #9386, .F. ) ;
#23676 = CARTESIAN_POINT ( 'NONE',  ( 51.17290532404582848, 0.9646187004851777269, -1.462925393634799232 ) ) ;
#23677 = DIRECTION ( 'NONE',  ( -1.000000000000000000, 0.000000000000000000, 0.000000000000000000 ) ) ;
#23678 = EDGE_LOOP ( 'NONE', ( #14460, #9266, #1878, #22190 ) ) ;
#23679 = DIRECTION ( 'NONE',  ( 2.466396912850936180E-16, -0.1459676528264960971, 0.9892893632948469573 ) ) ;
#23680 = CYLINDRICAL_SURFACE ( 'NONE', #24794, 0.09999999999999982514 ) ;
#23681 = CIRCLE ( 'NONE', #22587, 0.1500000000000001887 ) ;
#23682 = CARTESIAN_POINT ( 'NONE',  ( 58.75000000000002132, 6.153735859711025284E-13, 3.111507638930570854E-58 ) ) ;
#23683 = ORIENTED_EDGE ( 'NONE', *, *, #8643, .F. ) ;
#23684 = EDGE_LOOP ( 'NONE', ( #27076, #22483 ) ) ;
#23685 = CIRCLE ( 'NONE', #10019, 0.05000000000000143219 ) ;
#23686 = EDGE_CURVE ( 'NONE', #20639, #24678, #649, .T. ) ;
#23687 = VECTOR ( 'NONE', #28512, 999.9999999999998863 ) ;
#23688 = DIRECTION ( 'NONE',  ( 0.000000000000000000, -1.000000000000000000, 0.000000000000000000 ) ) ;
#23689 = DIRECTION ( 'NONE',  ( 0.000000000000000000, -1.000000000000000000, 0.000000000000000000 ) ) ;
#23690 = CARTESIAN_POINT ( 'NONE',  ( -54.84585481156724285, 3.673546848079182858, 0.7533615035078058408 ) ) ;
#23691 = EDGE_LOOP ( 'NONE', ( #9721, #14723, #2066 ) ) ;
#23692 = DIRECTION ( 'NONE',  ( 0.000000000000000000, 1.000000000000000000, 0.000000000000000000 ) ) ;
#23693 = CARTESIAN_POINT ( 'NONE',  ( 56.96274124341056222, 0.7308628367038140228, 1.753832840855930719 ) ) ;
#23694 = DIRECTION ( 'NONE',  ( 1.000000000000000000, 3.054027077731387480E-16, -2.042479963029832083E-16 ) ) ;
#23695 = CARTESIAN_POINT ( 'NONE',  ( -58.95655989232411542, -3.399999999999991029, -2.281093130107142867E-13 ) ) ;
#23696 = CARTESIAN_POINT ( 'NONE',  ( 58.65000000000001990, 6.143261415694495821E-13, 3.111507638930570854E-58 ) ) ;
#23697 = PLANE ( 'NONE',  #30614 ) ;
#23698 = CARTESIAN_POINT ( 'NONE',  ( 46.99309270008836847, -4.271967808728817317, 0.9446991603439680585 ) ) ;
#23699 = EDGE_CURVE ( 'NONE', #18829, #28844, #22408, .T. ) ;
#23700 = DIRECTION ( 'NONE',  ( 3.489354422748178582E-15, -1.218509414717996338E-16, 1.000000000000000000 ) ) ;
#23701 = ORIENTED_EDGE ( 'NONE', *, *, #8536, .T. ) ;
#23702 = AXIS2_PLACEMENT_3D ( 'NONE', #25319, #24841, #22478 ) ;
#23703 = AXIS2_PLACEMENT_3D ( 'NONE', #6213, #3538, #839 ) ;
#23704 = CARTESIAN_POINT ( 'NONE',  ( 58.73794315689197987, 0.5000000000006152856, -1.843373610710533628 ) ) ;
#23705 = EDGE_LOOP ( 'NONE', ( #11242, #17796, #22839, #25513 ) ) ;
#23706 = CARTESIAN_POINT ( 'NONE',  ( 51.75611399313550720, 4.330462468343535321, 2.050000000000262279 ) ) ;
#23707 = CARTESIAN_POINT ( 'NONE',  ( -57.59585481156722864, -2.489203624310587060, 2.804704140674918467 ) ) ;
#23709 = CARTESIAN_POINT ( 'NONE',  ( -36.42771574642738130, 3.560621078037010001, 4.077054076718899189 ) ) ;
#23708 = CARTESIAN_POINT ( 'NONE',  ( -55.20655989232412963, -3.399999999999991473, -2.086450695418937968E-13 ) ) ;
#23710 = ORIENTED_EDGE ( 'NONE', *, *, #21241, .T. ) ;
#23711 = ADVANCED_FACE ( 'NONE', ( #17541 ), #6222, .T. ) ;
#23712 = CARTESIAN_POINT ( 'NONE',  ( 23.38852972788364326, 6.106843900651806933, -2.050000000000079758 ) ) ;
#23713 = ORIENTED_EDGE ( 'NONE', *, *, #22485, .T. ) ;
#23714 = DIRECTION ( 'NONE',  ( 1.000000000000000000, 2.586136946169074517E-16, -0.000000000000000000 ) ) ;
#23715 = ORIENTED_EDGE ( 'NONE', *, *, #3963, .T. ) ;
#23717 = DIRECTION ( 'NONE',  ( 0.000000000000000000, 1.000000000000000000, 0.000000000000000000 ) ) ;
#23716 = CARTESIAN_POINT ( 'NONE',  ( 50.40918227724429812, 1.198378070452317257, 3.921585382224057614 ) ) ;
#23718 = EDGE_LOOP ( 'NONE', ( #30071, #10538, #550, #4486 ) ) ;
#23719 = CARTESIAN_POINT ( 'NONE',  ( 56.99137905793185155, -0.7079296279778910517, 1.763407125847052725 ) ) ;
#23720 = CYLINDRICAL_SURFACE ( 'NONE', #1119, 0.1000000000000000472 ) ;
#23721 = EDGE_CURVE ( 'NONE', #8161, #19150, #8732, .T. ) ;
#23722 = CARTESIAN_POINT ( 'NONE',  ( -61.34999999999997300, -2.635021238245644160, -0.5887810068220489246 ) ) ;
#23723 = PLANE ( 'NONE',  #16277 ) ;
#23724 = CARTESIAN_POINT ( 'NONE',  ( -57.38452994616203284, 2.093608279459370457E-14, -3.600000000000203926 ) ) ;
#23725 = FACE_OUTER_BOUND ( 'NONE', #10324, .T. ) ;
#23726 = CIRCLE ( 'NONE', #10061, 0.1000000000000001166 ) ;
#23727 = DIRECTION ( 'NONE',  ( 0.000000000000000000, -0.2008964009354147484, 0.9796124928211139560 ) ) ;
#23728 = CARTESIAN_POINT ( 'NONE',  ( 50.50000000000001421, 0.6462379109120998111, -4.048750000000022276 ) ) ;
#23729 = CARTESIAN_POINT ( 'NONE',  ( -57.67292740578359656, -3.330682475591780101, -0.6830477631804258154 ) ) ;
#23730 = ADVANCED_FACE ( 'NONE', ( #8336 ), #16935, .T. ) ;
#23731 = CARTESIAN_POINT ( 'NONE',  ( 61.16864364483315342, 0.7080009476653978950, 1.871974308545524490 ) ) ;
#23732 = AXIS2_PLACEMENT_3D ( 'NONE', #19181, #14240, #16793 ) ;
#23733 = VERTEX_POINT ( 'NONE', #13198 ) ;
#23734 = DIRECTION ( 'NONE',  ( 0.000000000000000000, -1.000000000000000000, 0.000000000000000000 ) ) ;
#23735 = CARTESIAN_POINT ( 'NONE',  ( -36.23324115033522475, -0.2667568399897324860, 5.200000000294890512 ) ) ;
#23736 = CARTESIAN_POINT ( 'NONE',  ( -77.29999999999998295, -3.473832742311974792E-15, 5.302342620690189014E-15 ) ) ;
#23737 = ORIENTED_EDGE ( 'NONE', *, *, #27843, .F. ) ;
#23738 = CARTESIAN_POINT ( 'NONE',  ( -36.89831264271880684, -5.047763082740456930, 1.943828653492516212 ) ) ;
#23739 = ORIENTED_EDGE ( 'NONE', *, *, #4237, .T. ) ;
#23741 = CARTESIAN_POINT ( 'NONE',  ( 58.72419296898098651, -1.357170035999222035, 1.293880926823872457 ) ) ;
#23740 = CARTESIAN_POINT ( 'NONE',  ( 50.59602332238209499, -0.1408342061598477080, -1.212874140286674507 ) ) ;
#23742 = ADVANCED_FACE ( 'NONE', ( #23197 ), #18286, .F. ) ;
#23743 = ORIENTED_EDGE ( 'NONE', *, *, #24282, .F. ) ;
#23744 = FACE_BOUND ( 'NONE', #14850, .T. ) ;
#23745 =( GEOMETRIC_REPRESENTATION_CONTEXT ( 3 ) GLOBAL_UNCERTAINTY_ASSIGNED_CONTEXT ( ( #5371 ) ) GLOBAL_UNIT_ASSIGNED_CONTEXT ( ( #4761, #19505, #7305 ) ) REPRESENTATION_CONTEXT ( 'NONE', 'WORKASPACE' ) );
#23746 = CIRCLE ( 'NONE', #4015, 4.300000000000016698 ) ;
#23747 = DIRECTION ( 'NONE',  ( 1.000000000000000000, -1.219044193948983948E-29, 3.491481338843133355E-15 ) ) ;
#23749 = CARTESIAN_POINT ( 'NONE',  ( 58.72419296898083019, 0.8985315506027614640, 1.645806614395225242 ) ) ;
#23748 = DIRECTION ( 'NONE',  ( 1.000000000000000000, 1.047444401652940007E-14, 0.000000000000000000 ) ) ;
#23750 = VERTEX_POINT ( 'NONE', #6095 ) ;
#23751 = CARTESIAN_POINT ( 'NONE',  ( -60.04792740578359656, -2.256877952708263635, 2.542931754211925188 ) ) ;
#23752 = DIRECTION ( 'NONE',  ( 1.000000000000000000, 3.054025858079668409E-16, -2.042474015755241579E-16 ) ) ;
#23753 = CARTESIAN_POINT ( 'NONE',  ( -54.59585481156724285, -2.489203624310586616, 2.804704140674918023 ) ) ;
#23754 = CARTESIAN_POINT ( 'NONE',  ( 68.00000000000004263, 0.6617647058823536987, 1.754335336828722003 ) ) ;
#23755 = EDGE_CURVE ( 'NONE', #2624, #3490, #19371, .T. ) ;
#23756 = DIRECTION ( 'NONE',  ( 0.000000000000000000, 0.000000000000000000, 1.000000000000000000 ) ) ;
#23757 = FACE_OUTER_BOUND ( 'NONE', #20648, .T. ) ;
#23758 = ADVANCED_FACE ( 'NONE', ( #28403 ), #14310, .T. ) ;
#23759 = CARTESIAN_POINT ( 'NONE',  ( -54.45487361440510909, 1.499999999999999556, -4.029888335921975262 ) ) ;
#23760 = ADVANCED_FACE ( 'NONE', ( #16061 ), #20816, .F. ) ;
#23761 = ORIENTED_EDGE ( 'NONE', *, *, #22889, .T. ) ;
#23762 = DIRECTION ( 'NONE',  ( 0.000000000000000000, -0.3529411764705882026, 0.9356455129756979794 ) ) ;
#23763 = AXIS2_PLACEMENT_3D ( 'NONE', #26103, #23583, #18682 ) ;
#23764 = CARTESIAN_POINT ( 'NONE',  ( 61.24672990992799981, 0.9412912739139536189, -1.685898893892158412 ) ) ;
#23765 = DIRECTION ( 'NONE',  ( -1.168655815394902336E-14, 0.000000000000000000, -1.000000000000000000 ) ) ;
#23766 = CARTESIAN_POINT ( 'NONE',  ( -59.29999999999997584, 0.7533615035078071731, -3.673546848079177529 ) ) ;
#23767 = DIRECTION ( 'NONE',  ( 0.000000000000000000, -0.9996898646859344595, -0.02490330187381105745 ) ) ;
#23768 = AXIS2_PLACEMENT_3D ( 'NONE', #6632, #30856, #6781 ) ;
#23770 = CARTESIAN_POINT ( 'NONE',  ( 58.45000000000001705, -0.8000000000000000444, 1.778341924377873751 ) ) ;
#23769 = CARTESIAN_POINT ( 'NONE',  ( 52.06628335902946247, -0.5434431642975677823, 1.718465885608439603 ) ) ;
#23772 = CIRCLE ( 'NONE', #7577, 2.650000000000000799 ) ;
#23771 = CARTESIAN_POINT ( 'NONE',  ( 50.50000000000002132, 2.428612866367529932E-14, 0.000000000000000000 ) ) ;
#23774 = CARTESIAN_POINT ( 'NONE',  ( 68.00000000000001421, -1.025519176787267142E-28, -7.122621931239990530E-13 ) ) ;
#23773 = CARTESIAN_POINT ( 'NONE',  ( -35.85663232820584057, 3.275050215668543263, 2.949461045527633996 ) ) ;
#23775 = ORIENTED_EDGE ( 'NONE', *, *, #27991, .F. ) ;
#23776 = DIRECTION ( 'NONE',  ( 3.491481338843133355E-15, 0.000000000000000000, 1.000000000000000000 ) ) ;
#23777 = CARTESIAN_POINT ( 'NONE',  ( -60.59999999999997300, 1.626093840209163176E-15, 1.891350188320046374E-15 ) ) ;
#23778 = CARTESIAN_POINT ( 'NONE',  ( 15.41080140630260686, -2.595266697484886365, -4.757426534476337565 ) ) ;
#23779 = CARTESIAN_POINT ( 'NONE',  ( 15.76675455518197388, -5.110933801299744950, 1.769007076671009093 ) ) ;
#23780 = EDGE_CURVE ( 'NONE', #12772, #5904, #10759, .T. ) ;
#23781 = ORIENTED_EDGE ( 'NONE', *, *, #30008, .F. ) ;
#23782 = ORIENTED_EDGE ( 'NONE', *, *, #31068, .F. ) ;
#23783 = CARTESIAN_POINT ( 'NONE',  ( -35.85663232820578372, -4.683225679163362187, 2.703237727951222968 ) ) ;
#23784 = LINE ( 'NONE', #4134, #20944 ) ;
#23785 =( BOUNDED_SURFACE ( )  B_SPLINE_SURFACE ( 3, 2, ( 
 ( #29708, #27333, #14245 ),
 ( #23916, #21718, #2209 ),
 ( #11874, #5644, #31196 ),
 ( #9675, #4903, #15297 ) ),
 .UNSPECIFIED., .F., .F., .F. ) 
 B_SPLINE_SURFACE_WITH_KNOTS ( ( 4, 4 ),
 ( 3, 3 ),
 ( 1.353422612224536969, 1.454597276681381723 ),
 ( 0.000000000000000000, 1.000000000000000000 ),
 .UNSPECIFIED. ) 
 GEOMETRIC_REPRESENTATION_ITEM ( )  RATIONAL_B_SPLINE_SURFACE ( (
 ( 1.000000000000000000, 0.6314033403188393789, 1.000000000000000000),
 ( 1.000000000000000000, 0.6436559554927198112, 1.000000000000000000),
 ( 1.000000000000000000, 0.6556885524390240194, 1.000000000000000000),
 ( 1.000000000000000000, 0.6674781514195016197, 1.000000000000000000) ) ) 
 REPRESENTATION_ITEM ( '' )  SURFACE ( )  );
#23786 = VERTEX_POINT ( 'NONE', #1173 ) ;
#23787 = EDGE_CURVE ( 'NONE', #15114, #27829, #11268, .T. ) ;
#23788 = CARTESIAN_POINT ( 'NONE',  ( 58.75000000000002132, 6.153735859711025284E-13, 3.111507638930570854E-58 ) ) ;
#23789 = ORIENTED_EDGE ( 'NONE', *, *, #27536, .F. ) ;
#23790 = DIRECTION ( 'NONE',  ( -1.000000000000000000, 0.000000000000000000, 1.047444401652940007E-14 ) ) ;
#23791 = ORIENTED_EDGE ( 'NONE', *, *, #2864, .F. ) ;
#23792 = SURFACE_SIDE_STYLE ('',( #2565 ) ) ;
#23793 = CARTESIAN_POINT ( 'NONE',  ( -59.83155989232413674, -1.962990915244731571, 3.399999999999779199 ) ) ;
#23794 = EDGE_CURVE ( 'NONE', #12232, #19795, #13661, .T. ) ;
#23795 = EDGE_LOOP ( 'NONE', ( #14942, #14901, #21932, #19399 ) ) ;
#23796 = CIRCLE ( 'NONE', #21282, 3.625000000000024869 ) ;
#23797 = CARTESIAN_POINT ( 'NONE',  ( -59.62499999999996447, 2.944486372867106905, -1.700000000000199130 ) ) ;
#23798 = CARTESIAN_POINT ( 'NONE',  ( 56.95640338720422591, -0.7513613876702617267, 2.489093304807997509 ) ) ;
#23799 = FACE_BOUND ( 'NONE', #1963, .T. ) ;
#23800 = DIRECTION ( 'NONE',  ( -1.000000000000000000, -1.047444401652940007E-14, 0.000000000000000000 ) ) ;
#23801 = LINE ( 'NONE', #15061, #24644 ) ;
#23803 = CARTESIAN_POINT ( 'NONE',  ( 51.71860689488131868, 4.174878657598904752, -1.931421652553907187 ) ) ;
#23802 = CARTESIAN_POINT ( 'NONE',  ( -35.85663232820584767, 4.683225679163358635, -2.703237727951174563 ) ) ;
#23804 = B_SPLINE_CURVE_WITH_KNOTS ( 'NONE', 3,
 ( #28546, #23663, #21605, #1954, #11614, #21297, #30926, #9572, #6856, #16523, #26180, #14135, #23810, #26334, #31071, #9396, #19064 ),
 .UNSPECIFIED., .F., .F.,
 ( 4, 2, 2, 2, 2, 1, 2, 2, 4 ),
 ( 0.000000000000000000, 0.1147774566006787567, 0.1721661849010180101, 0.2295549132013572635, 0.2869436415016964892, 0.3443323698020356871, 0.3730267339522053693, 0.4017210981023749961, 0.4591098264027145270 ),
 .UNSPECIFIED. ) ;
#23805 = DIRECTION ( 'NONE',  ( -1.000000000000000000, -0.000000000000000000, -0.000000000000000000 ) ) ;
#23806 = LINE ( 'NONE', #21437, #13954 ) ;
#23807 = CARTESIAN_POINT ( 'NONE',  ( 15.57907767661756182, 5.286410563980352251, -1.167394352644079314 ) ) ;
#23808 = ORIENTED_EDGE ( 'NONE', *, *, #30295, .T. ) ;
#23809 = CARTESIAN_POINT ( 'NONE',  ( -54.83155989232413674, 3.400000000000008349, -1.845326485282803322E-13 ) ) ;
#23810 = CARTESIAN_POINT ( 'NONE',  ( 54.02661639416933781, 7.247660624457942014, 2.049999999999812417 ) ) ;
#23811 = ORIENTED_EDGE ( 'NONE', *, *, #10338, .F. ) ;
#23813 = CARTESIAN_POINT ( 'NONE',  ( 50.42118334212123898, -1.311095223031168766, 3.884869838566831657 ) ) ;
#23812 = CARTESIAN_POINT ( 'NONE',  ( 50.25000000000004263, -1.996089927834392208, -0.1249999999999982098 ) ) ;
#23814 = CARTESIAN_POINT ( 'NONE',  ( 54.42157971047652865, 6.359826807111529590, -2.020139939762307879 ) ) ;
#23815 = ADVANCED_FACE ( 'NONE', ( #27926 ), #27441, .F. ) ;
#23816 = CARTESIAN_POINT ( 'NONE',  ( 58.75000000000002132, 6.153735859711025284E-13, 3.111507638930570854E-58 ) ) ;
#23817 = AXIS2_PLACEMENT_3D ( 'NONE', #21863, #151, #26277 ) ;
#23818 = ADVANCED_FACE ( 'NONE', ( #20969, #30602 ), #13339, .F. ) ;
#23819 = ORIENTED_EDGE ( 'NONE', *, *, #4791, .F. ) ;
#23820 = EDGE_CURVE ( 'NONE', #31094, #7978, #16218, .T. ) ;
#23821 = FACE_OUTER_BOUND ( 'NONE', #28479, .T. ) ;
#23822 = LINE ( 'NONE', #4963, #25925 ) ;
#23823 = CARTESIAN_POINT ( 'NONE',  ( -60.56249999999995026, -1.962990915244707368, -3.400000000000221956 ) ) ;
#23824 = ORIENTED_EDGE ( 'NONE', *, *, #22943, .F. ) ;
#23825 = ORIENTED_EDGE ( 'NONE', *, *, #22966, .T. ) ;
#23826 = CARTESIAN_POINT ( 'NONE',  ( 15.76623786017564122, 5.109611055794853307, 1.772889539330601449 ) ) ;
#23827 = VERTEX_POINT ( 'NONE', #1485 ) ;
#23828 = CARTESIAN_POINT ( 'NONE',  ( 51.80056195330648450, 4.599988466687112698, 0.2643113378676240077 ) ) ;
#23829 = CARTESIAN_POINT ( 'NONE',  ( -56.00952994616203995, -3.117691453623963938, -1.800000000000210099 ) ) ;
#23830 = VERTEX_POINT ( 'NONE', #1783 ) ;
#23831 = CARTESIAN_POINT ( 'NONE',  ( -60.59999999999998010, -2.292917048100124866, -1.057429151542457868 ) ) ;
#23832 = FACE_OUTER_BOUND ( 'NONE', #12387, .T. ) ;
#23833 = CARTESIAN_POINT ( 'NONE',  ( 27.81683722849680507, 5.540920426341900296, 2.049999999999902567 ) ) ;
#23834 = ORIENTED_EDGE ( 'NONE', *, *, #3436, .T. ) ;
#23835 = ORIENTED_EDGE ( 'NONE', *, *, #29957, .T. ) ;
#23836 = EDGE_CURVE ( 'NONE', #9397, #8955, #13763, .T. ) ;
#23837 = LINE ( 'NONE', #23984, #24863 ) ;
#23838 = CARTESIAN_POINT ( 'NONE',  ( -62.09999999999997300, -2.724924404790626031, 0.2013854104211484086 ) ) ;
#23839 = CARTESIAN_POINT ( 'NONE',  ( 51.43641343869300186, -0.9728999281633509133, 1.446772403416499930 ) ) ;
#23840 = ORIENTED_EDGE ( 'NONE', *, *, #22799, .T. ) ;
#23841 = CARTESIAN_POINT ( 'NONE',  ( -60.64999999999998437, -2.511038422848939078, 0.9923134781793048198 ) ) ;
#23842 = DIRECTION ( 'NONE',  ( -3.002035892788116966E-16, 0.9996898646859343485, 0.02490330187381123786 ) ) ;
#23843 = CARTESIAN_POINT ( 'NONE',  ( -58.61505354137800339, 3.400000000000014566, -0.9110272542660011741 ) ) ;
#23845 = DIRECTION ( 'NONE',  ( 0.000000000000000000, 0.000000000000000000, 1.000000000000000000 ) ) ;
#23844 = PRESENTATION_STYLE_ASSIGNMENT (( #4519 ) ) ;
#23846 = CARTESIAN_POINT ( 'NONE',  ( 51.72668767004672929, -4.179189507150981697, 0.9999999999999995559 ) ) ;
#23847 = CARTESIAN_POINT ( 'NONE',  ( 15.03925126672132784, 5.086913985776138070, 1.171642053949162987 ) ) ;
#23848 = DIRECTION ( 'NONE',  ( 0.000000000000000000, 1.000000000000000000, 8.673617379884030739E-15 ) ) ;
#23849 = EDGE_LOOP ( 'NONE', ( #13635, #29001, #17784 ) ) ;
#23850 = ADVANCED_FACE ( 'NONE', ( #30139 ), #3970, .T. ) ;
#23851 = EDGE_LOOP ( 'NONE', ( #5463, #7789, #27669, #22764 ) ) ;
#23852 = AXIS2_PLACEMENT_3D ( 'NONE', #18159, #1185, #3876 ) ;
#23853 = CARTESIAN_POINT ( 'NONE',  ( 58.75000000000001421, 0.5000000000003640421, -1.863080903343440786 ) ) ;
#23854 = ORIENTED_EDGE ( 'NONE', *, *, #23659, .F. ) ;
#23855 = DIRECTION ( 'NONE',  ( 1.520093157366863638E-16, -0.5877852522924685852, -0.8090169943749507819 ) ) ;
#23856 = CARTESIAN_POINT ( 'NONE',  ( -56.23542740578360366, -3.725040285533364859, 1.239922660687674982 ) ) ;
#23858 = CARTESIAN_POINT ( 'NONE',  ( -36.31440869660544024, 3.012234853004066348, 4.239036759381678898 ) ) ;
#23857 = DIRECTION ( 'NONE',  ( 0.000000000000000000, 0.2008964009354147762, -0.9796124928211140670 ) ) ;
#23859 = ORIENTED_EDGE ( 'NONE', *, *, #25005, .T. ) ;
#23860 = EDGE_LOOP ( 'NONE', ( #14592, #9045, #408, #29392 ) ) ;
#23861 = CARTESIAN_POINT ( 'NONE',  ( -61.34999999999997300, -2.583824419212624957, -0.5885162450438690129 ) ) ;
#23862 = EDGE_LOOP ( 'NONE', ( #7159, #27866, #19202, #3173 ) ) ;
#23863 = CARTESIAN_POINT ( 'NONE',  ( -44.59999999999998721, 1.399999999999998135, 3.363870538531280818 ) ) ;
#23864 = ORIENTED_EDGE ( 'NONE', *, *, #19496, .T. ) ;
#23866 = DIRECTION ( 'NONE',  ( 1.000000000000000000, 3.385297212316223527E-16, 2.459562394685754633E-16 ) ) ;
#23865 = CARTESIAN_POINT ( 'NONE',  ( -35.85663232820584767, 5.377732432866621615, 0.5657657256216177544 ) ) ;
#23867 = ORIENTED_EDGE ( 'NONE', *, *, #2293, .T. ) ;
#23868 = CARTESIAN_POINT ( 'NONE',  ( 68.00000000000004263, 0.7500000000000000000, 1.988246715072646387 ) ) ;
#23869 = CARTESIAN_POINT ( 'NONE',  ( 57.01262970566578758, 0.7335977677777304473, 1.792760110902297921 ) ) ;
#23870 = EDGE_CURVE ( 'NONE', #25369, #16804, #21910, .T. ) ;
#23871 = CARTESIAN_POINT ( 'NONE',  ( -36.40793637698146057, 0.9785522574021833231, -5.318456145981288685 ) ) ;
#23872 = TOROIDAL_SURFACE ( 'NONE', #1094, 2.674999999999998934, 0.05000000000000000278 ) ;
#23873 = DIRECTION ( 'NONE',  ( 0.000000000000000000, -0.000000000000000000, -1.000000000000000000 ) ) ;
#23874 = CARTESIAN_POINT ( 'NONE',  ( -56.94702994616206126, -2.078460969082657872, 3.599999999999789591 ) ) ;
#23875 = CARTESIAN_POINT ( 'NONE',  ( -44.49999999999999289, 1.499999999999999556, 3.300094695611021756 ) ) ;
#23876 = CIRCLE ( 'NONE', #601, 0.09999999999999982514 ) ;
#23877 = AXIS2_PLACEMENT_3D ( 'NONE', #19092, #9105, #26504 ) ;
#23878 = CARTESIAN_POINT ( 'NONE',  ( 30.31473038486000249, 6.776227631128586282, 1.549999999999894129 ) ) ;
#23879 = DIRECTION ( 'NONE',  ( 0.000000000000000000, 0.000000000000000000, -1.000000000000000000 ) ) ;
#23880 = CARTESIAN_POINT ( 'NONE',  ( -56.67292740578360366, 2.256877952708273849, -2.542931754211921191 ) ) ;
#23881 = DIRECTION ( 'NONE',  ( -3.491481338843133355E-15, 0.000000000000000000, -1.000000000000000000 ) ) ;
#23882 = EDGE_LOOP ( 'NONE', ( #22110, #4830, #18408, #21418 ) ) ;
#23883 = DIRECTION ( 'NONE',  ( -0.9993908270190958731, 0.03489949670249913732, 3.435095992031088928E-15 ) ) ;
#23884 = CARTESIAN_POINT ( 'NONE',  ( -36.31414349454749413, 0.05686983728433445129, 5.199999998842928406 ) ) ;
#23885 = CARTESIAN_POINT ( 'NONE',  ( 53.94314916079858335, 6.379172879799750007, -1.774223561664970861 ) ) ;
#23886 = VERTEX_POINT ( 'NONE', #9251 ) ;
#23887 = EDGE_CURVE ( 'NONE', #19028, #15276, #23926, .T. ) ;
#23888 = CARTESIAN_POINT ( 'NONE',  ( -54.49853245345825314, 1.536420219664552445, 4.055116445457032981 ) ) ;
#23889 = VERTEX_POINT ( 'NONE', #14146 ) ;
#23890 =( NAMED_UNIT ( * ) PLANE_ANGLE_UNIT ( ) SI_UNIT ( $, .RADIAN. ) );
#23892 = DIRECTION ( 'NONE',  ( 0.000000000000000000, 0.000000000000000000, -1.000000000000000000 ) ) ;
#23891 = CARTESIAN_POINT ( 'NONE',  ( 51.52469891147812575, -4.265589706924725277, -1.723997649431408430 ) ) ;
#23893 = ORIENTED_EDGE ( 'NONE', *, *, #29026, .T. ) ;
#23894 = CARTESIAN_POINT ( 'NONE',  ( -43.84599839145305111, -8.171597657156649598E-15, 0.000000000000000000 ) ) ;
#23895 = CARTESIAN_POINT ( 'NONE',  ( 61.25000000000001421, 1.039502773797213120, -1.650471618823823539 ) ) ;
#23897 = CARTESIAN_POINT ( 'NONE',  ( 58.73371041428920591, 0.8671977075797476786, 1.662559130998980894 ) ) ;
#23896 = CARTESIAN_POINT ( 'NONE',  ( 58.65000000000002700, -0.5540123067490997366, 1.791510860176260600 ) ) ;
#23898 = ORIENTED_EDGE ( 'NONE', *, *, #19121, .F. ) ;
#23899 = CARTESIAN_POINT ( 'NONE',  ( -59.79792740578359656, -1.073804522883517576, -3.225979517392334905 ) ) ;
#23900 = CARTESIAN_POINT ( 'NONE',  ( 61.24891880570152836, 0.9671362613610259285, 1.669082548207006633 ) ) ;
#23901 = CARTESIAN_POINT ( 'NONE',  ( 51.80000000000002558, -3.701043595308292300, 1.983423889356453751 ) ) ;
#23902 = CARTESIAN_POINT ( 'NONE',  ( -55.45655989232413674, 1.962990915244720247, 3.399999999999811173 ) ) ;
#23903 = EDGE_CURVE ( 'NONE', #24785, #25198, #15823, .T. ) ;
#23904 = CARTESIAN_POINT ( 'NONE',  ( -61.38641854932647135, -2.625280434238165483, -0.6244966117725891941 ) ) ;
#23905 = CARTESIAN_POINT ( 'NONE',  ( -56.67499999999996874, -0.9743475445367589804, 4.751120590182402736 ) ) ;
#23907 = CARTESIAN_POINT ( 'NONE',  ( -44.59999999999997300, 3.624999999999963585, -1.915392816594897430E-13 ) ) ;
#23906 = CIRCLE ( 'NONE', #31029, 2.685355339059328106 ) ;
#23908 = ORIENTED_EDGE ( 'NONE', *, *, #11165, .F. ) ;
#23909 = DIRECTION ( 'NONE',  ( 0.000000000000000000, 0.2008964009354148039, -0.9796124928211140670 ) ) ;
#23910 = CARTESIAN_POINT ( 'NONE',  ( 15.29954477411492242, -4.018128194441231926, 3.618665885216586720 ) ) ;
#23911 = DIRECTION ( 'NONE',  ( 0.7313537016191670181, 0.6819983600625022513, -2.468850131082252327E-15 ) ) ;
#23912 = LINE ( 'NONE', #2205, #28569 ) ;
#23913 = ADVANCED_FACE ( 'NONE', ( #11627 ), #23670, .T. ) ;
#23914 = CARTESIAN_POINT ( 'NONE',  ( 57.00000000000001421, 0.000000000000000000, 0.000000000000000000 ) ) ;
#23915 = B_SPLINE_CURVE_WITH_KNOTS ( 'NONE', 3,
 ( #3695, #30134, #20508, #30443, #27610, #23195 ),
 .UNSPECIFIED., .F., .F.,
 ( 4, 2, 4 ),
 ( 0.000000000000000000, 0.0001000270069598648232, 0.0002000540139197296463 ),
 .UNSPECIFIED. ) ;
#23917 = CARTESIAN_POINT ( 'NONE',  ( 58.65000000000001990, 6.143261415694495821E-13, 3.111507638930570854E-58 ) ) ;
#23916 = CARTESIAN_POINT ( 'NONE',  ( -61.60260218697150236, -2.667562526553216795, 0.4270849601371985993 ) ) ;
#23919 = CARTESIAN_POINT ( 'NONE',  ( 51.25000000000001421, 5.368152558471320595E-13, 3.111507638930570854E-58 ) ) ;
#23918 = DIRECTION ( 'NONE',  ( 0.000000000000000000, 0.000000000000000000, 1.000000000000000000 ) ) ;
#23920 = ORIENTED_EDGE ( 'NONE', *, *, #21542, .F. ) ;
#23921 = EDGE_CURVE ( 'NONE', #5946, #2387, #5199, .T. ) ;
#23922 = CARTESIAN_POINT ( 'NONE',  ( -60.49999999999997868, 1.656632322739229403E-15, 1.870925083934595927E-15 ) ) ;
#23923 = EDGE_CURVE ( 'NONE', #15131, #2938, #23822, .T. ) ;
#23924 =( BOUNDED_SURFACE ( )  B_SPLINE_SURFACE ( 3, 2, ( 
 ( #28828, #28673, #20919 ),
 ( #13917, #28195, #2063 ),
 ( #9201, #6809, #13757 ),
 ( #21402, #16471, #19189 ),
 ( #31030, #11400, #26130 ),
 ( #6504, #7140, #16801 ),
 ( #1580, #21089, #30549 ),
 ( #11876, #8857, #21557 ),
 ( #18548, #21253, #30883 ),
 ( #23613, #6989, #16164 ) ),
 .UNSPECIFIED., .F., .F., .F. ) 
 B_SPLINE_SURFACE_WITH_KNOTS ( ( 4, 2, 2, 2, 4 ),
 ( 3, 3 ),
 ( -5.421010862427522170E-20, 0.0003534648051082250452, 0.0007069296102164500904, 0.001060394415324675136, 0.001413859220432900181 ),
 ( 0.000000000000000000, 1.000000000000000000 ),
 .UNSPECIFIED. ) 
 GEOMETRIC_REPRESENTATION_ITEM ( )  RATIONAL_B_SPLINE_SURFACE ( (
 ( 1.000000000000000000, 0.7071067811865467956, 1.000000000000000000),
 ( 1.000000000000000000, 0.6969521241105990361, 1.000000000000000000),
 ( 1.000000000000000000, 0.6903264600368322901, 1.000000000000000000),
 ( 1.000000000000000000, 0.6841066566211814193, 1.000000000000000000),
 ( 1.000000000000000000, 0.6845305055655173110, 1.000000000000000000),
 ( 1.000000000000000000, 0.6885489555120742899, 1.000000000000000000),
 ( 1.000000000000000000, 0.6920376555000889995, 1.000000000000000000),
 ( 1.000000000000000000, 0.6973723772405847621, 1.000000000000000000),
 ( 1.000000000000000000, 0.6992679762638227547, 1.000000000000000000),
 ( 1.000000000000000000, 0.6992058987801016423, 1.000000000000000000) ) ) 
 REPRESENTATION_ITEM ( '' )  SURFACE ( )  );
#23925 = CARTESIAN_POINT ( 'NONE',  ( 50.40000000000001990, 2.428612866367529932E-14, 0.000000000000000000 ) ) ;
#23926 = CIRCLE ( 'NONE', #18868, 2.625000000001612044 ) ;
#23928 = CARTESIAN_POINT ( 'NONE',  ( -36.23324115033478421, 4.863061488092484730, 1.860589201779825341 ) ) ;
#23927 = CARTESIAN_POINT ( 'NONE',  ( 15.76623786017565187, -3.091683853621961298, -4.437651790014649045 ) ) ;
#23929 = CARTESIAN_POINT ( 'NONE',  ( 15.22842924604202786, -4.861582136950232780, 2.394243986684292391 ) ) ;
#23930 = ORIENTED_EDGE ( 'NONE', *, *, #11947, .F. ) ;
#23931 = ORIENTED_EDGE ( 'NONE', *, *, #10687, .F. ) ;
#23932 = DIRECTION ( 'NONE',  ( 0.000000000000000000, -3.469446951953614189E-15, 1.000000000000000000 ) ) ;
#23933 = EDGE_LOOP ( 'NONE', ( #10824, #12397, #1378, #14945, #23835, #12738, #22020, #27774, #14806, #1499, #579, #31211 ) ) ;
#23934 = CARTESIAN_POINT ( 'NONE',  ( 56.98113911906671092, 0.7884861235339004626, -2.477567088838556586 ) ) ;
#23935 = CARTESIAN_POINT ( 'NONE',  ( 51.80000048029783244, 4.021162535479849254, 2.019963026417355589 ) ) ;
#23936 = EDGE_LOOP ( 'NONE', ( #5446, #17453, #29289, #31186 ) ) ;
#23937 = CARTESIAN_POINT ( 'NONE',  ( 58.74999999999999289, 1.872332544501730256, 0.09997921184905476932 ) ) ;
#23938 = VERTEX_POINT ( 'NONE', #2265 ) ;
#23939 = SHAPE_REPRESENTATION_RELATIONSHIP ( 'NONE' , 'NONE' ,  #18201, #12719 ) ;
#23940 = EDGE_CURVE ( 'NONE', #22859, #27565, #14926, .T. ) ;
#23941 = CARTESIAN_POINT ( 'NONE',  ( 51.80000000000001137, -3.637377585518695611, -2.099877210783217318 ) ) ;
#23942 = ORIENTED_EDGE ( 'NONE', *, *, #22998, .F. ) ;
#23943 = VERTEX_POINT ( 'NONE', #9870 ) ;
#23944 = CARTESIAN_POINT ( 'NONE',  ( -59.99999999999997158, -2.944486372867089141, 1.699999999999775913 ) ) ;
#23945 = CARTESIAN_POINT ( 'NONE',  ( -57.65400635094607651, 1.737685414808524342, -3.471684241605563770 ) ) ;
#23946 = DIRECTION ( 'NONE',  ( 0.000000000000000000, -0.8740818021021516948, -0.4857787595540328796 ) ) ;
#23947 = AXIS2_PLACEMENT_3D ( 'NONE', #18714, #28510, #26135 ) ;
#23948 = DIRECTION ( 'NONE',  ( 0.000000000000000000, 0.000000000000000000, 1.000000000000000000 ) ) ;
#23949 = AXIS2_PLACEMENT_3D ( 'NONE', #27098, #19377, #10316 ) ;
#23950 = ADVANCED_FACE ( 'NONE', ( #19542 ), #12098, .T. ) ;
#23951 = DIRECTION ( 'NONE',  ( -1.000000000000000000, -0.000000000000000000, 3.491481338843133750E-15 ) ) ;
#23952 = EDGE_CURVE ( 'NONE', #17544, #125, #23651, .T. ) ;
#23954 = DIRECTION ( 'NONE',  ( 1.000000000000000000, 1.047444401652940007E-14, 0.000000000000000000 ) ) ;
#23953 = CARTESIAN_POINT ( 'NONE',  ( -73.89999999999997726, 0.4498604391086679644, 0.01120648584322002546 ) ) ;
#23955 = CARTESIAN_POINT ( 'NONE',  ( 50.35762544161294585, 8.151359338959888845, -1.550000000000175016 ) ) ;
#23956 = DIRECTION ( 'NONE',  ( 1.000000000000000000, -0.000000000000000000, -1.047444401652940007E-14 ) ) ;
#23957 = CARTESIAN_POINT ( 'NONE',  ( -36.00197790576392975, -2.199885893005944837, -4.939696249117692339 ) ) ;
#23958 = ORIENTED_EDGE ( 'NONE', *, *, #10719, .F. ) ;
#23959 =( BOUNDED_CURVE ( )  B_SPLINE_CURVE ( 2, ( #5981, #3731, #15633, #13229, #11032, #1202, #10859, #20549, #18176 ),
 .UNSPECIFIED., .F., .T. ) 
 B_SPLINE_CURVE_WITH_KNOTS ( ( 3, 2, 2, 2, 3 ),
 ( 0.7554589434467710030, 0.7592592592592593004, 0.7777777777777777901, 0.7962962962962962798, 0.7991619333968115191 ),
 .UNSPECIFIED. ) 
 CURVE ( )  GEOMETRIC_REPRESENTATION_ITEM ( )  RATIONAL_B_SPLINE_CURVE ( ( 0.9562966789351563524, 0.9725061280706346345, 1.000000000000000000, 0.8660254037844387076, 1.000000000000000000, 0.8660254037844387076, 1.000000000000000000, 0.9792681810341394844, 0.9649526279839704124 ) ) 
 REPRESENTATION_ITEM ( '' )  );
#23960 = CARTESIAN_POINT ( 'NONE',  ( -54.49999999999997868, -3.745083032500879039, 0.1919715595446555012 ) ) ;
#23961 = EDGE_CURVE ( 'NONE', #2253, #19424, #26935, .T. ) ;
#23962 = CARTESIAN_POINT ( 'NONE',  ( 50.30837315852409830, 1.391941090707552897, -3.850000000000020517 ) ) ;
#23964 = DIRECTION ( 'NONE',  ( 3.489354422748178582E-15, -1.218509414717996338E-16, 1.000000000000000000 ) ) ;
#23963 = CARTESIAN_POINT ( 'NONE',  ( 48.38952526309123670, -0.7808213810455604253, 4.027268569370238360 ) ) ;
#23966 = EDGE_CURVE ( 'NONE', #22535, #24580, #19877, .T. ) ;
#23965 = CARTESIAN_POINT ( 'NONE',  ( 54.28362896329676346, 5.641750298212469872, -1.990863909997389714 ) ) ;
#23967 = CARTESIAN_POINT ( 'NONE',  ( -73.89999999999997726, -0.4598573377555323360, -0.01145551886194856595 ) ) ;
#23968 = VERTEX_POINT ( 'NONE', #5116 ) ;
#23969 = DIRECTION ( 'NONE',  ( 1.000000000000000000, -0.000000000000000000, -0.000000000000000000 ) ) ;
#23970 = CIRCLE ( 'NONE', #3232, 3.950000000000000178 ) ;
#23971 = CARTESIAN_POINT ( 'NONE',  ( 30.89639353599806881, 7.705332861457931948, 1.424999999999892575 ) ) ;
#23972 = CARTESIAN_POINT ( 'NONE',  ( -60.43749999999995026, 1.962990915244749557, -3.400000000000205969 ) ) ;
#23973 = ORIENTED_EDGE ( 'NONE', *, *, #11843, .F. ) ;
#23974 = ORIENTED_EDGE ( 'NONE', *, *, #20283, .T. ) ;
#23975 = CARTESIAN_POINT ( 'NONE',  ( 15.57907767661755649, 4.962973169597125533, 2.162832296644338737 ) ) ;
#23976 = ORIENTED_EDGE ( 'NONE', *, *, #533, .F. ) ;
#23977 = CARTESIAN_POINT ( 'NONE',  ( 51.96339880813594192, 4.380689046771754747, 1.403568635141169807 ) ) ;
#23978 = CARTESIAN_POINT ( 'NONE',  ( -58.38452994616204705, -3.117691453623976816, 1.799999999999780442 ) ) ;
#23979 = VERTEX_POINT ( 'NONE', #8116 ) ;
#23980 = CYLINDRICAL_SURFACE ( 'NONE', #4978, 0.2500000000000000000 ) ;
#23981 = CARTESIAN_POINT ( 'NONE',  ( 51.87765138016307986, 8.698644590117595499, -1.950000000000180256 ) ) ;
#23982 = CARTESIAN_POINT ( 'NONE',  ( 30.93618511144813610, 7.271541257249599433, 2.049999999999891465 ) ) ;
#23983 = ORIENTED_EDGE ( 'NONE', *, *, #29857, .T. ) ;
#23984 = CARTESIAN_POINT ( 'NONE',  ( -35.85663232820584057, -0.4576450603546987628, 5.200000000000000178 ) ) ;
#23985 = DIRECTION ( 'NONE',  ( -1.000000000000000000, -0.000000000000000000, 1.047444401652940007E-14 ) ) ;
#23986 = CARTESIAN_POINT ( 'NONE',  ( -60.59999999999997300, -2.458552378503722657, 0.9390651652154902163 ) ) ;
#23987 = VERTEX_POINT ( 'NONE', #5589 ) ;
#23988 = DIRECTION ( 'NONE',  ( 1.000000000000000000, 0.000000000000000000, -0.000000000000000000 ) ) ;
#23989 = ADVANCED_FACE ( 'NONE', ( #14912 ), #827, .T. ) ;
#23990 = CARTESIAN_POINT ( 'NONE',  ( 56.99150396717417522, 0.7610778266783598811, 1.740907964752457904 ) ) ;
#23991 = ADVANCED_FACE ( 'NONE', ( #10646 ), #30572, .T. ) ;
#23992 = EDGE_CURVE ( 'NONE', #1882, #7461, #13790, .T. ) ;
#23994 = CARTESIAN_POINT ( 'NONE',  ( 57.05000000000001847, 0.7500000000000000000, 2.421260002560649660 ) ) ;
#23993 = CARTESIAN_POINT ( 'NONE',  ( -36.11692583559974423, -2.199885872771085271, 4.939696258129251838 ) ) ;
#23995 = AXIS2_PLACEMENT_3D ( 'NONE', #26417, #18993, #139 ) ;
#23996 = CARTESIAN_POINT ( 'NONE',  ( 51.59739104186226655, 1.010292945603182391, 1.272765950230260179 ) ) ;
#23997 = DIRECTION ( 'NONE',  ( -3.491481338843133355E-15, -3.491481338843133355E-15, 1.000000000000000000 ) ) ;
#23998 = DIRECTION ( 'NONE',  ( -1.000000000000000000, 1.219044193948983948E-29, -3.491481338843133355E-15 ) ) ;
#23999 = EDGE_LOOP ( 'NONE', ( #31222, #21319 ) ) ;
#24000 = ORIENTED_EDGE ( 'NONE', *, *, #4637, .T. ) ;
#24001 = CARTESIAN_POINT ( 'NONE',  ( 58.66864673770887606, 0.5000000000006145084, -1.807442289571237204 ) ) ;
#24002 = ORIENTED_EDGE ( 'NONE', *, *, #22387, .T. ) ;
#24003 = CARTESIAN_POINT ( 'NONE',  ( 54.16553928697277343, 6.951169537962178069, 2.049999999999812861 ) ) ;
#24004 = CARTESIAN_POINT ( 'NONE',  ( -55.67292740578360366, 1.073804522883522239, 3.225979517392336238 ) ) ;
#24005 = CARTESIAN_POINT ( 'NONE',  ( 51.41633779460606490, 0.9865878673145904720, -1.594768911165097558 ) ) ;
#24006 = VERTEX_POINT ( 'NONE', #20325 ) ;
#24007 = TOROIDAL_SURFACE ( 'NONE', #10343, 2.649999999999999911, 0.05000000000000000278 ) ;
#24008 = VERTEX_POINT ( 'NONE', #12543 ) ;
#24009 = CARTESIAN_POINT ( 'NONE',  ( 22.11607288752048461, 7.780659299909677529, -2.050000000000077094 ) ) ;
#24010 = ORIENTED_EDGE ( 'NONE', *, *, #14114, .F. ) ;
#24011 = CARTESIAN_POINT ( 'NONE',  ( 30.31473038486000249, 6.776227631128586282, 1.949999999999893818 ) ) ;
#24012 = ORIENTED_EDGE ( 'NONE', *, *, #1937, .F. ) ;
#24013 = DIRECTION ( 'NONE',  ( 0.000000000000000000, -0.9996898646859343485, -0.02490330187381124133 ) ) ;
#24014 = AXIS2_PLACEMENT_3D ( 'NONE', #11039, #1209, #4063 ) ;
#24015 = CARTESIAN_POINT ( 'NONE',  ( 34.50000000000001421, 0.000000000000000000, -3.200000000000000178 ) ) ;
#24016 = CARTESIAN_POINT ( 'NONE',  ( 57.04540039768303217, 0.7500000000000000000, 1.778341924377873751 ) ) ;
#24017 = DIRECTION ( 'NONE',  ( 0.000000000000000000, -0.2573099415204678775, -0.9663289263986324373 ) ) ;
#24018 = CARTESIAN_POINT ( 'NONE',  ( 58.45000000000001705, -0.8000000000000000444, -2.421260002560649660 ) ) ;
#24019 = AXIS2_PLACEMENT_3D ( 'NONE', #13304, #8572, #8263 ) ;
#24020 = CARTESIAN_POINT ( 'NONE',  ( -56.70655989232412253, -3.925981830489445379, -2.155497846303743205E-13 ) ) ;
#24021 = CARTESIAN_POINT ( 'NONE',  ( -59.25695844465221285, 3.255054294100257817, -0.9827484482200410376 ) ) ;
#24022 = ADVANCED_FACE ( 'NONE', ( #15238 ), #24739, .T. ) ;
#24023 = EDGE_CURVE ( 'NONE', #1800, #1101, #21504, .T. ) ;
#24024 = DIRECTION ( 'NONE',  ( 3.167104333282667910E-32, -1.224646799147353207E-16, 1.000000000000000000 ) ) ;
#24025 = DIRECTION ( 'NONE',  ( 0.000000000000000000, 0.000000000000000000, -1.000000000000000000 ) ) ;
#24026 = CARTESIAN_POINT ( 'NONE',  ( 61.25000000000002132, 6.415596960124259844E-13, 3.111507638930570854E-58 ) ) ;
#24027 = ORIENTED_EDGE ( 'NONE', *, *, #943, .F. ) ;
#24028 = DIRECTION ( 'NONE',  ( -0.000000000000000000, 1.000000000000000000, 3.491481338843133355E-15 ) ) ;
#24029 = CIRCLE ( 'NONE', #28061, 0.1000000000000001721 ) ;
#24030 = EDGE_LOOP ( 'NONE', ( #6918, #12890, #18289, #21213 ) ) ;
#24031 = LINE ( 'NONE', #11839, #28534 ) ;
#24032 = DIRECTION ( 'NONE',  ( 0.000000000000000000, 0.000000000000000000, -1.000000000000000000 ) ) ;
#24033 = CARTESIAN_POINT ( 'NONE',  ( 53.81464057712626925, 5.799094425976097256, -7.641258220787705557E-08 ) ) ;
#24034 = ORIENTED_EDGE ( 'NONE', *, *, #10347, .F. ) ;
#24035 = EDGE_CURVE ( 'NONE', #12135, #25275, #22136, .T. ) ;
#24036 = ORIENTED_EDGE ( 'NONE', *, *, #11732, .F. ) ;
#24037 = AXIS2_PLACEMENT_3D ( 'NONE', #7760, #17425, #27071 ) ;
#24038 = CARTESIAN_POINT ( 'NONE',  ( 15.29384114148384199, 0.3980941177579093715, -5.199999998461561468 ) ) ;
#24040 = DIRECTION ( 'NONE',  ( 0.000000000000000000, -0.9996898646859343485, -0.02490330187381143562 ) ) ;
#24039 = CARTESIAN_POINT ( 'NONE',  ( 50.92089186451759275, -4.387164041431066863, -1.383037119376936630 ) ) ;
#24041 = EDGE_LOOP ( 'NONE', ( #6436, #9584, #11965, #13348 ) ) ;
#24042 = DIRECTION ( 'NONE',  ( 1.000000000000000000, 2.586136946169074517E-16, -0.000000000000000000 ) ) ;
#24043 = DIRECTION ( 'NONE',  ( 1.000000000000000000, 0.000000000000000000, -1.047444401652940007E-14 ) ) ;
#24045 = CARTESIAN_POINT ( 'NONE',  ( 34.55000000000001847, 0.000000000000000000, 0.000000000000000000 ) ) ;
#24044 = FACE_OUTER_BOUND ( 'NONE', #20252, .T. ) ;
#24046 = ORIENTED_EDGE ( 'NONE', *, *, #29244, .F. ) ;
#24047 = CARTESIAN_POINT ( 'NONE',  ( -55.12499999999997868, 1.184343223768590692, 3.558065644182724530 ) ) ;
#24048 = DIRECTION ( 'NONE',  ( 0.000000000000000000, -1.000000000000000000, 0.000000000000000000 ) ) ;
#24049 = CARTESIAN_POINT ( 'NONE',  ( -54.62486116251335488, -1.737685414808515239, 3.471684241605564214 ) ) ;
#24050 = VECTOR ( 'NONE', #10158, 1000.000000000000000 ) ;
#24051 = CARTESIAN_POINT ( 'NONE',  ( 60.75000000000001421, 0.5000000000006363798, 1.863080903344386030 ) ) ;
#24052 = VECTOR ( 'NONE', #16843, 1000.000000000000000 ) ;
#24053 = CARTESIAN_POINT ( 'NONE',  ( 57.00000000000001421, 0.000000000000000000, 0.000000000000000000 ) ) ;
#24054 = CARTESIAN_POINT ( 'NONE',  ( -57.68749999999996447, -3.399999999999991029, -2.155011314204633625E-13 ) ) ;
#24055 = DIRECTION ( 'NONE',  ( 1.000000000000000000, -0.000000000000000000, -0.000000000000000000 ) ) ;
#24056 = AXIS2_PLACEMENT_3D ( 'NONE', #804, #15217, #1262 ) ;
#24057 = ORIENTED_EDGE ( 'NONE', *, *, #13, .T. ) ;
#24058 = CIRCLE ( 'NONE', #3330, 1.302039949377232331 ) ;
#24059 = ADVANCED_FACE ( 'NONE', ( #15385 ), #22013, .T. ) ;
#24060 = CARTESIAN_POINT ( 'NONE',  ( 48.00000000000001421, -3.937842575352406005, -1.145831896685989282 ) ) ;
#24061 = TOROIDAL_SURFACE ( 'NONE', #796, 0.2000000000000000111, 0.1000000000000000056 ) ;
#24062 = CARTESIAN_POINT ( 'NONE',  ( 15.76623786017565187, -3.265074799938555206, 4.311675893544620664 ) ) ;
#24063 = LINE ( 'NONE', #26437, #24730 ) ;
#24064 = DIRECTION ( 'NONE',  ( 1.000000000000000000, -0.000000000000000000, -1.047444401652940007E-14 ) ) ;
#24065 = CARTESIAN_POINT ( 'NONE',  ( -62.06488485593400384, -2.667381432228959515, 0.2068147105598954205 ) ) ;
#24067 = CARTESIAN_POINT ( 'NONE',  ( 33.47623932017462778, 4.018128179617571405, -3.618665901676623164 ) ) ;
#24066 = CARTESIAN_POINT ( 'NONE',  ( 33.47623932017462778, 5.377732432866640266, 0.5657657256216092057 ) ) ;
#24068 = CARTESIAN_POINT ( 'NONE',  ( 61.24796382359981806, -0.9549219522834025975, 1.676592304037839209 ) ) ;
#24070 = CARTESIAN_POINT ( 'NONE',  ( 50.40000000000001990, -0.6304760106459033064, -3.950000000000022826 ) ) ;
#24069 = FACE_OUTER_BOUND ( 'NONE', #22880, .T. ) ;
#24071 = AXIS2_PLACEMENT_3D ( 'NONE', #6804, #16156, #18700 ) ;
#24072 = ORIENTED_EDGE ( 'NONE', *, *, #17400, .T. ) ;
#24073 = EDGE_CURVE ( 'NONE', #19244, #18673, #22374, .T. ) ;
#24074 = LINE ( 'NONE', #14722, #15340 ) ;
#24075 = UNCERTAINTY_MEASURE_WITH_UNIT (LENGTH_MEASURE( 1.000000000000000082E-05 ), #15355, 'distance_accuracy_value', 'NONE');
#24076 = FACE_OUTER_BOUND ( 'NONE', #25067, .T. ) ;
#24078 = CARTESIAN_POINT ( 'NONE',  ( -36.11187263677958725, 4.822464347459026968, 1.985534350301239481 ) ) ;
#24077 = CARTESIAN_POINT ( 'NONE',  ( 15.39414421509785491, -2.821511581828335391, -4.377605326016334786 ) ) ;
#24079 = CYLINDRICAL_SURFACE ( 'NONE', #13526, 0.05000000000000012768 ) ;
#24080 = CIRCLE ( 'NONE', #3327, 4.100000000000022737 ) ;
#24081 = EDGE_LOOP ( 'NONE', ( #13742, #17858, #12175, #8957 ) ) ;
#24082 = ORIENTED_EDGE ( 'NONE', *, *, #29439, .T. ) ;
#24083 = CARTESIAN_POINT ( 'NONE',  ( 61.25000000000003553, -1.039502773796076474, -1.800471618824325493 ) ) ;
#24084 = AXIS2_PLACEMENT_3D ( 'NONE', #20192, #13034, #18122 ) ;
#24085 = AXIS2_PLACEMENT_3D ( 'NONE', #14249, #25965, #27219 ) ;
#24086 = EDGE_LOOP ( 'NONE', ( #24957, #25135, #25239, #29812 ) ) ;
#24087 = MECHANICAL_DESIGN_GEOMETRIC_PRESENTATION_REPRESENTATION (  '', ( #7402 ), #11970 ) ;
#24088 = LINE ( 'NONE', #8751, #22617 ) ;
#24089 = CARTESIAN_POINT ( 'NONE',  ( 58.69321565534330887, 0.5000000000006147305, 1.812725888577170430 ) ) ;
#24090 = ORIENTED_EDGE ( 'NONE', *, *, #20091, .T. ) ;
#24091 = CARTESIAN_POINT ( 'NONE',  ( -36.48821680285229263, -5.009497273852872468, -2.047744636826959397 ) ) ;
#24092 = VERTEX_POINT ( 'NONE', #22230 ) ;
#24093 = B_SPLINE_CURVE_WITH_KNOTS ( 'NONE', 3,
 ( #12168, #26261, #1880, #4568, #23891, #4875, #21848, #21523, #24039, #24205 ),
 .UNSPECIFIED., .F., .F.,
 ( 4, 2, 2, 2, 4 ),
 ( 0.000000000000000000, 0.0003601004132760234544, 0.0007202008265520462582, 0.001080301239828069170, 0.001440401653104092300 ),
 .UNSPECIFIED. ) ;
#24094 = VECTOR ( 'NONE', #28148, 1000.000000000000000 ) ;
#24095 = CARTESIAN_POINT ( 'NONE',  ( 51.06462745158204086, -4.023728077055554131, -1.198744011644903518 ) ) ;
#24096 = EDGE_LOOP ( 'NONE', ( #11147, #29587 ) ) ;
#24097 = AXIS2_PLACEMENT_3D ( 'NONE', #16249, #21001, #15774 ) ;
#24098 = EDGE_LOOP ( 'NONE', ( #24393, #29807, #23387, #14330 ) ) ;
#24099 = EDGE_CURVE ( 'NONE', #10647, #20935, #16948, .T. ) ;
#24100 = CARTESIAN_POINT ( 'NONE',  ( -60.06249999999997868, -1.962990915244731793, 3.399999999999778755 ) ) ;
#24101 = TOROIDAL_SURFACE ( 'NONE', #22082, 2.525000000001608846, 0.1000000000000000056 ) ;
#24102 = LINE ( 'NONE', #26927, #7485 ) ;
#24103 = CARTESIAN_POINT ( 'NONE',  ( 47.10000000000002274, -4.179189514726507682, 0.9999999999999997780 ) ) ;
#24105 = EDGE_CURVE ( 'NONE', #7417, #30820, #11873, .T. ) ;
#24104 = CYLINDRICAL_SURFACE ( 'NONE', #28107, 0.05000000000000143219 ) ;
#24106 = CONICAL_SURFACE ( 'NONE', #22085, 3.299999999999999822, 0.03997868712329010615 ) ;
#24107 = CARTESIAN_POINT ( 'NONE',  ( 50.80000000000001847, -3.908336260473453727, -1.238913909466097474 ) ) ;
#24108 = AXIS2_PLACEMENT_3D ( 'NONE', #28661, #26435, #23762 ) ;
#24109 = AXIS2_PLACEMENT_3D ( 'NONE', #13791, #16684, #23474 ) ;
#24111 = CARTESIAN_POINT ( 'NONE',  ( -36.31414349454749413, -0.05686983728438164964, -5.199999998842928406 ) ) ;
#24110 = CARTESIAN_POINT ( 'NONE',  ( -35.85663232820584057, 4.804073783693455724, -2.042134687550314354 ) ) ;
#24112 =( BOUNDED_SURFACE ( )  B_SPLINE_SURFACE ( 3, 2, ( 
 ( #4550, #22423, #13065 ),
 ( #5305, #567, #17835 ),
 ( #15286, #20224, #24933 ),
 ( #14811, #10078, #19602 ),
 ( #15133, #26998, #420 ),
 ( #7837, #19753, #715 ),
 ( #12747, #3254, #29383 ),
 ( #5635, #3097, #17680 ),
 ( #5787, #20058, #7553 ),
 ( #29852, #8166, #29523 ),
 ( #257, #15442, #27469 ),
 ( #17514, #10375, #2950 ),
 ( #24472, #27169, #12595 ),
 ( #25094, #5481, #29695 ),
 ( #7695, #17353, #8015 ),
 ( #12897, #10225, #890 ) ),
 .UNSPECIFIED., .F., .F., .F. ) 
 B_SPLINE_SURFACE_WITH_KNOTS ( ( 4, 2, 2, 2, 2, 2, 2, 4 ),
 ( 3, 3 ),
 ( 0.001780502285214213788, 0.002558945925323803227, 0.002753556835351200424, 0.002948167745378598055, 0.003337389565433392449, 0.003726611385488186844, 0.004115833205542981238, 0.004894276845652570894 ),
 ( 0.000000000000000000, 1.000000000000000000 ),
 .UNSPECIFIED. ) 
 GEOMETRIC_REPRESENTATION_ITEM ( )  RATIONAL_B_SPLINE_SURFACE ( (
 ( 1.000000000000000000, 0.9418517008537217183, 1.000000000000000000),
 ( 1.000000000000000000, 0.9417987965884941914, 1.000000000000000000),
 ( 1.000000000000000000, 0.9418198861734206062, 1.000000000000000000),
 ( 1.000000000000000000, 0.9434060303845515083, 1.000000000000000000),
 ( 1.000000000000000000, 0.9437939819948067965, 1.000000000000000000),
 ( 1.000000000000000000, 0.9445989566712852392, 1.000000000000000000),
 ( 1.000000000000000000, 0.9450169930049960865, 1.000000000000000000),
 ( 1.000000000000000000, 0.9461610507673310355, 1.000000000000000000),
 ( 1.000000000000000000, 0.9467217966427192710, 1.000000000000000000),
 ( 1.000000000000000000, 0.9467345476124342518, 1.000000000000000000),
 ( 1.000000000000000000, 0.9461964028052916031, 1.000000000000000000),
 ( 1.000000000000000000, 0.9446801822473820387, 1.000000000000000000),
 ( 1.000000000000000000, 0.9437582546536950057, 1.000000000000000000),
 ( 1.000000000000000000, 0.9418129560294778990, 1.000000000000000000),
 ( 1.000000000000000000, 0.9418016889778114686, 1.000000000000000000),
 ( 1.000000000000000000, 0.9418517008537208302, 1.000000000000000000) ) ) 
 REPRESENTATION_ITEM ( '' )  SURFACE ( )  );
#24113 = CARTESIAN_POINT ( 'NONE',  ( -59.28559899066483041, 3.161828374300069466, 1.250136525132556020 ) ) ;
#24115 = FACE_OUTER_BOUND ( 'NONE', #22231, .T. ) ;
#24114 = CARTESIAN_POINT ( 'NONE',  ( 15.87128154250932255, 4.872353571451126797, -2.347449169364848487 ) ) ;
#24116 = B_SPLINE_CURVE_WITH_KNOTS ( 'NONE', 3,
 ( #30924, #21136, #27918, #13653 ),
 .UNSPECIFIED., .F., .F.,
 ( 4, 4 ),
 ( 2.710505431213761085E-20, 0.0001543670095910070058 ),
 .UNSPECIFIED. ) ;
#24117 = ORIENTED_EDGE ( 'NONE', *, *, #29245, .F. ) ;
#24118 = EDGE_CURVE ( 'NONE', #13582, #30927, #7817, .T. ) ;
#24119 = CARTESIAN_POINT ( 'NONE',  ( 50.25000000000001421, 0.6373668173475077747, -1.895722432252298084 ) ) ;
#24120 = CARTESIAN_POINT ( 'NONE',  ( 48.00000000000001421, -4.319730106884873244, -1.256953381662404778 ) ) ;
#24121 = VECTOR ( 'NONE', #11376, 1000.000000000000000 ) ;
#24123 = LINE ( 'NONE', #14295, #28255 ) ;
#24122 = CARTESIAN_POINT ( 'NONE',  ( 58.65000000000001990, 6.143261415694495821E-13, 3.111507638930570854E-58 ) ) ;
#24124 = CARTESIAN_POINT ( 'NONE',  ( 54.33836953411530146, 6.362880879443651772, -2.050000000000188560 ) ) ;
#24125 = VERTEX_POINT ( 'NONE', #15852 ) ;
#24126 = CARTESIAN_POINT ( 'NONE',  ( 51.70000000000000995, -3.550773357292059007, -2.049880134336001802 ) ) ;
#24127 = AXIS2_PLACEMENT_3D ( 'NONE', #15467, #13702, #13089 ) ;
#24128 = AXIS2_PLACEMENT_3D ( 'NONE', #14250, #23444, #1732 ) ;
#24129 = VERTEX_POINT ( 'NONE', #5900 ) ;
#24130 = DIRECTION ( 'NONE',  ( -1.110223024625156540E-14, 0.000000000000000000, -1.000000000000000000 ) ) ;
#24131 = CARTESIAN_POINT ( 'NONE',  ( -56.82202994616205416, -4.156921938165296204, -2.167734102480683039E-13 ) ) ;
#24132 = ORIENTED_EDGE ( 'NONE', *, *, #13301, .F. ) ;
#24133 = ADVANCED_FACE ( 'NONE', ( #15559 ), #25208, .F. ) ;
#24134 = ORIENTED_EDGE ( 'NONE', *, *, #12347, .F. ) ;
#24135 = CARTESIAN_POINT ( 'NONE',  ( -54.49999999999997868, -6.102218906431378987E-14, -2.216533082070118739E-13 ) ) ;
#24136 = EDGE_LOOP ( 'NONE', ( #400, #15319, #29033, #28283 ) ) ;
#24137 = CARTESIAN_POINT ( 'NONE',  ( 51.25000000000001421, 1.100000000000534994, 1.001327244211404732 ) ) ;
#24138 = CARTESIAN_POINT ( 'NONE',  ( -54.94702994616205416, 4.156921938165313080, -1.801810997602979365E-13 ) ) ;
#24139 = ORIENTED_EDGE ( 'NONE', *, *, #18885, .F. ) ;
#24140 = CARTESIAN_POINT ( 'NONE',  ( 47.09453520915242564, 9.265918505097243241, -2.050000000000163691 ) ) ;
#24141 = AXIS2_PLACEMENT_3D ( 'NONE', #16318, #14089, #1728 ) ;
#24142 = CARTESIAN_POINT ( 'NONE',  ( -57.68749999999996447, -3.399999999999991029, -2.155011314204633625E-13 ) ) ;
#24143 = CARTESIAN_POINT ( 'NONE',  ( 28.66473729876423704, 5.839050301631238504, 2.049999999999899902 ) ) ;
#24144 = ORIENTED_EDGE ( 'NONE', *, *, #19031, .F. ) ;
#24145 = ADVANCED_FACE ( 'NONE', ( #6062 ), #17960, .T. ) ;
#24146 = DIRECTION ( 'NONE',  ( 0.000000000000000000, 0.000000000000000000, 1.000000000000000000 ) ) ;
#24147 = ADVANCED_FACE ( 'NONE', ( #20476 ), #15908, .T. ) ;
#24148 = DIRECTION ( 'NONE',  ( 0.000000000000000000, 0.2008964009354148594, -0.9796124928211140670 ) ) ;
#24149 = CARTESIAN_POINT ( 'NONE',  ( 57.00000000000001421, 0.000000000000000000, 0.000000000000000000 ) ) ;
#24150 = AXIS2_PLACEMENT_3D ( 'NONE', #5928, #23019, #8738 ) ;
#24152 = EDGE_CURVE ( 'NONE', #15593, #6507, #14047, .T. ) ;
#24151 = CARTESIAN_POINT ( 'NONE',  ( -71.49999999999998579, -0.4118376219176019259, 2.008205610283286813 ) ) ;
#24153 = CARTESIAN_POINT ( 'NONE',  ( 58.65815574817527533, 0.5272471384325619903, -1.799565140949186404 ) ) ;
#24154 = CIRCLE ( 'NONE', #10493, 1.975000000000001865 ) ;
#24155 =( BOUNDED_CURVE ( )  B_SPLINE_CURVE ( 2, ( #23363, #11481, #11643, #11302, #30951, #6574, #20987, #18623, #16235 ),
 .UNSPECIFIED., .F., .T. ) 
 B_SPLINE_CURVE_WITH_KNOTS ( ( 3, 2, 2, 2, 3 ),
 ( 0.1388888888888888951, 0.1481481481481481399, 0.1666666666666666574, 0.1851851851851851749, 0.1944444444444444475 ),
 .UNSPECIFIED. ) 
 CURVE ( )  GEOMETRIC_REPRESENTATION_ITEM ( )  RATIONAL_B_SPLINE_CURVE ( ( 0.9330127018922192983, 0.9330127018922194093, 1.000000000000000000, 0.8660254037844387076, 1.000000000000000000, 0.8660254037844387076, 1.000000000000000000, 0.9330127018922191873, 0.9330127018922192983 ) ) 
 REPRESENTATION_ITEM ( '' )  );
#24156 = VECTOR ( 'NONE', #18509, 1000.000000000000114 ) ;
#24157 = CARTESIAN_POINT ( 'NONE',  ( 58.75000018595671492, -0.9248597378508944811, 1.701752411746787930 ) ) ;
#24158 = CARTESIAN_POINT ( 'NONE',  ( 51.75337531998826535, -4.276948325786879224, 0.9210526687159865666 ) ) ;
#24159 = CARTESIAN_POINT ( 'NONE',  ( 58.75000000000000711, 1.039502773796331159, 1.800471618825331355 ) ) ;
#24160 = AXIS2_PLACEMENT_3D ( 'NONE', #6603, #8794, #21018 ) ;
#24161 = CARTESIAN_POINT ( 'NONE',  ( 51.97945110550971037, 4.337541896208930048, 1.549654688285104331 ) ) ;
#24162 = CIRCLE ( 'NONE', #17096, 0.01000000000000001929 ) ;
#24163 = AXIS2_PLACEMENT_3D ( 'NONE', #24716, #21906, #10015 ) ;
#24164 = VERTEX_POINT ( 'NONE', #18254 ) ;
#24165 = ORIENTED_EDGE ( 'NONE', *, *, #24706, .T. ) ;
#24166 = CARTESIAN_POINT ( 'NONE',  ( 51.88778388204188730, 0.01071552754804109761, -4.374297461196706927 ) ) ;
#24167 = ORIENTED_EDGE ( 'NONE', *, *, #5040, .F. ) ;
#24168 = CARTESIAN_POINT ( 'NONE',  ( -59.84585481156722864, -2.489203624310587504, 2.804704140674918911 ) ) ;
#24170 = DIRECTION ( 'NONE',  ( 3.491481338843133355E-15, 3.491481338843133355E-15, -1.000000000000000000 ) ) ;
#24169 = CARTESIAN_POINT ( 'NONE',  ( 58.75000000000002132, 6.153735859711025284E-13, 3.111507638930570854E-58 ) ) ;
#24171 = CIRCLE ( 'NONE', #1844, 1.899999999999999911 ) ;
#24172 = ORIENTED_EDGE ( 'NONE', *, *, #21235, .T. ) ;
#24173 = EDGE_CURVE ( 'NONE', #8534, #16069, #2263, .T. ) ;
#24174 = EDGE_LOOP ( 'NONE', ( #18410, #29025, #18685, #11694 ) ) ;
#24175 = CARTESIAN_POINT ( 'NONE',  ( -73.89999999999997726, -2.435524336289708093E-15, 4.607889071584891164E-15 ) ) ;
#24176 = ORIENTED_EDGE ( 'NONE', *, *, #8441, .T. ) ;
#24177 = CARTESIAN_POINT ( 'NONE',  ( 21.97322666366009614, 8.076925076899403422, -1.950000000000076117 ) ) ;
#24178 = CIRCLE ( 'NONE', #5961, 4.100000000000000533 ) ;
#24179 = VERTEX_POINT ( 'NONE', #22849 ) ;
#24180 = CARTESIAN_POINT ( 'NONE',  ( 50.42106458229518751, 0.9199776782966334610, 3.998258245321812510 ) ) ;
#24181 = EDGE_CURVE ( 'NONE', #5779, #29991, #26039, .T. ) ;
#24182 = ORIENTED_EDGE ( 'NONE', *, *, #25736, .T. ) ;
#24183 = CARTESIAN_POINT ( 'NONE',  ( 53.37675057098704912, 7.899674929380397614, 1.885230776086536109 ) ) ;
#24184 = DIRECTION ( 'NONE',  ( 1.000000000000000000, -0.000000000000000000, -1.047444401652940007E-14 ) ) ;
#24185 = CARTESIAN_POINT ( 'NONE',  ( 58.64999999999999858, 1.872332544501833507, -0.09997921184724666011 ) ) ;
#24186 = CARTESIAN_POINT ( 'NONE',  ( -56.26905989232412963, 2.944486372867092250, 1.699999999999811218 ) ) ;
#24188 = ADVANCED_FACE ( 'NONE', ( #3820 ), #27544, .T. ) ;
#24187 = DIRECTION ( 'NONE',  ( -0.000000000000000000, 1.000000000000000000, 3.491481338843133355E-15 ) ) ;
#24189 = B_SPLINE_CURVE_WITH_KNOTS ( 'NONE', 3,
 ( #28714, #28390, #14288, #16839 ),
 .UNSPECIFIED., .F., .F.,
 ( 4, 4 ),
 ( 4.848699518061080308E-19, 0.0003408895603972687729 ),
 .UNSPECIFIED. ) ;
#24190 = DIRECTION ( 'NONE',  ( -1.000000000000000000, -0.000000000000000000, -0.000000000000000000 ) ) ;
#24191 = CARTESIAN_POINT ( 'NONE',  ( 51.90000000000001279, -4.227689052994015206, -1.125730994152046804 ) ) ;
#24192 = AXIS2_PLACEMENT_3D ( 'NONE', #16546, #14157, #9100 ) ;
#24193 = CARTESIAN_POINT ( 'NONE',  ( 15.18459684427940104, -5.377732432866643819, -0.5657657256215741226 ) ) ;
#24194 = ORIENTED_EDGE ( 'NONE', *, *, #27077, .T. ) ;
#24195 = CARTESIAN_POINT ( 'NONE',  ( -36.79682133506354091, 0.5584590966806799450, 5.380195666604549842 ) ) ;
#24196 = B_SPLINE_CURVE_WITH_KNOTS ( 'NONE', 3,
 ( #20736, #1870, #8998, #11540, #1693, #25777 ),
 .UNSPECIFIED., .F., .F.,
 ( 4, 2, 4 ),
 ( 0.000000000000000000, 0.5000000000000000000, 1.000000000000000000 ),
 .UNSPECIFIED. ) ;
#24197 = ORIENTED_EDGE ( 'NONE', *, *, #15516, .F. ) ;
#24198 = CARTESIAN_POINT ( 'NONE',  ( 52.20711756518984004, -0.4999999999994533817, 1.807104036850122109 ) ) ;
#24199 = DIRECTION ( 'NONE',  ( -1.000000000000000000, 1.219044193948983948E-29, -3.491481338843133355E-15 ) ) ;
#24200 = CARTESIAN_POINT ( 'NONE',  ( 53.90826771765248537, 6.078164526406591328, -1.689602626210267466 ) ) ;
#24201 = VERTEX_POINT ( 'NONE', #6521 ) ;
#24202 = DIRECTION ( 'NONE',  ( -1.000000000000000000, -3.053848253006669023E-16, 2.042510438544995415E-16 ) ) ;
#24203 = VERTEX_POINT ( 'NONE', #13620 ) ;
#24204 = CARTESIAN_POINT ( 'NONE',  ( 15.67083574136730384, -0.3995010896671927214, -5.397102918580121589 ) ) ;
#24205 = CARTESIAN_POINT ( 'NONE',  ( 50.80000000000001137, -4.387164041431065975, -1.383037119376935742 ) ) ;
#24206 = EDGE_LOOP ( 'NONE', ( #23683, #16476, #5396, #31293 ) ) ;
#24207 = EDGE_CURVE ( 'NONE', #16231, #24382, #13882, .T. ) ;
#24208 = DIRECTION ( 'NONE',  ( -0.5000000000000029976, -3.023711536277451078E-15, 0.8660254037844369313 ) ) ;
#24209 = ADVANCED_FACE ( 'NONE', ( #20785 ), #16180, .F. ) ;
#24210 = DIRECTION ( 'NONE',  ( 1.000000000000000000, -0.000000000000000000, -1.047444401652940007E-14 ) ) ;
#24212 = CARTESIAN_POINT ( 'NONE',  ( -54.49983703358571319, -1.542636180423123449, -4.059406436927352146 ) ) ;
#24211 = DIRECTION ( 'NONE',  ( 1.000000000000000000, 1.047444401652940007E-14, 0.000000000000000000 ) ) ;
#24213 = EDGE_CURVE ( 'NONE', #29437, #30188, #22500, .T. ) ;
#24214 = EDGE_LOOP ( 'NONE', ( #10139, #22194, #3215, #22417 ) ) ;
#24215 = CARTESIAN_POINT ( 'NONE',  ( -58.87499999999997158, 1.184343223768590025, 3.558065644182725418 ) ) ;
#24216 = DIRECTION ( 'NONE',  ( 3.016910393003118404E-15, 0.000000000000000000, 1.000000000000000000 ) ) ;
#24217 = AXIS2_PLACEMENT_3D ( 'NONE', #2842, #14864, #7743 ) ;
#24218 = CARTESIAN_POINT ( 'NONE',  ( -55.06249999999997158, 3.400000000000007905, -1.826733775103631524E-13 ) ) ;
#24219 = CIRCLE ( 'NONE', #6004, 0.2499999999999997780 ) ;
#24220 = VECTOR ( 'NONE', #8743, 1000.000000000000000 ) ;
#24221 = FACE_OUTER_BOUND ( 'NONE', #4371, .T. ) ;
#24222 = CARTESIAN_POINT ( 'NONE',  ( 52.10742411006412311, -0.5153926522284794087, 1.803012591436477408 ) ) ;
#24223 = DIRECTION ( 'NONE',  ( 0.000000000000000000, 0.000000000000000000, -1.000000000000000000 ) ) ;
#24224 = B_SPLINE_CURVE_WITH_KNOTS ( 'NONE', 3,
 ( #4113, #6497, #9027, #21079, #20766, #15986, #16155, #13436, #18541, #25648 ),
 .UNSPECIFIED., .F., .F.,
 ( 4, 3, 3, 4 ),
 ( 0.000000000000000000, 6.454972543172422090E-05, 0.0001290994513737798294, 0.0002445102546710338021 ),
 .UNSPECIFIED. ) ;
#24225 = ORIENTED_EDGE ( 'NONE', *, *, #24349, .T. ) ;
#24226 = EDGE_CURVE ( 'NONE', #31054, #1785, #28581, .T. ) ;
#24227 = CARTESIAN_POINT ( 'NONE',  ( 58.75000000000000000, 1.394635017528132570, 1.253243060178681922 ) ) ;
#24228 = CARTESIAN_POINT ( 'NONE',  ( 51.73328143279136526, 4.175271471638091647, 1.930573136446042337 ) ) ;
#24229 = CARTESIAN_POINT ( 'NONE',  ( 50.87477060347373481, 8.633605004118187765, -2.050000000000176570 ) ) ;
#24230 = CARTESIAN_POINT ( 'NONE',  ( -62.05074114918922845, -2.687605151338700704, 0.2580611626218518584 ) ) ;
#24232 = CARTESIAN_POINT ( 'NONE',  ( 53.36557156485857689, 7.911885792138814821, -1.886359577549349797 ) ) ;
#24231 = CARTESIAN_POINT ( 'NONE',  ( 58.66107449606962376, 1.301839550768181919, 1.349793924522737054 ) ) ;
#24233 =( GEOMETRIC_REPRESENTATION_CONTEXT ( 3 ) GLOBAL_UNCERTAINTY_ASSIGNED_CONTEXT ( ( #19343 ) ) GLOBAL_UNIT_ASSIGNED_CONTEXT ( ( #24746, #15243, #7968 ) ) REPRESENTATION_CONTEXT ( 'NONE', 'WORKASPACE' ) );
#24234 = CARTESIAN_POINT ( 'NONE',  ( -62.29999999999998295, 1.106939637198029038E-15, 2.238576962872695299E-15 ) ) ;
#24236 = DIRECTION ( 'NONE',  ( -3.491481338843133355E-15, -3.491481338843133355E-15, 1.000000000000000000 ) ) ;
#24235 = CARTESIAN_POINT ( 'NONE',  ( 51.58641917109738984, -3.755449232595080122, 1.648679025009623267 ) ) ;
#24237 = ORIENTED_EDGE ( 'NONE', *, *, #13405, .F. ) ;
#24238 = CARTESIAN_POINT ( 'NONE',  ( 58.65000000000001279, 0.8799718970826592157, -1.656030381686704134 ) ) ;
#24239 = DIRECTION ( 'NONE',  ( 0.000000000000000000, 1.000000000000000000, 3.491481338843130594E-15 ) ) ;
#24241 = FACE_OUTER_BOUND ( 'NONE', #25941, .T. ) ;
#24240 = LINE ( 'NONE', #28979, #10026 ) ;
#24242 = DIRECTION ( 'NONE',  ( -1.000000000000000000, 1.219044193948983948E-29, -3.491481338843133355E-15 ) ) ;
#24243 = ORIENTED_EDGE ( 'NONE', *, *, #10323, .T. ) ;
#24244 = ORIENTED_EDGE ( 'NONE', *, *, #17773, .T. ) ;
#24245 = CARTESIAN_POINT ( 'NONE',  ( -57.47085481156722864, -3.673546848079175753, -0.7533615035078066180 ) ) ;
#24246 = EDGE_CURVE ( 'NONE', #2409, #18413, #18400, .T. ) ;
#24247 = EDGE_LOOP ( 'NONE', ( #21807, #20096, #23132, #16583, #17343 ) ) ;
#24248 = DIRECTION ( 'NONE',  ( 1.000000000000000000, 1.047444401652940007E-14, 0.000000000000000000 ) ) ;
#24249 = AXIS2_PLACEMENT_3D ( 'NONE', #2204, #10231, #27174 ) ;
#24250 = VERTEX_POINT ( 'NONE', #3666 ) ;
#24251 = CARTESIAN_POINT ( 'NONE',  ( -59.63511902941204568, -2.173259666074455865, 1.527495276501993349 ) ) ;
#24252 = ORIENTED_EDGE ( 'NONE', *, *, #16827, .T. ) ;
#24253 = ORIENTED_EDGE ( 'NONE', *, *, #25455, .F. ) ;
#24254 = CIRCLE ( 'NONE', #13110, 2.600000000000000089 ) ;
#24255 = PRESENTATION_STYLE_ASSIGNMENT (( #14593 ) ) ;
#24256 = ORIENTED_EDGE ( 'NONE', *, *, #29700, .T. ) ;
#24257 = EDGE_LOOP ( 'NONE', ( #4370, #19065, #19340, #18552, #9661 ) ) ;
#24258 =( GEOMETRIC_REPRESENTATION_CONTEXT ( 3 ) GLOBAL_UNCERTAINTY_ASSIGNED_CONTEXT ( ( #15190 ) ) GLOBAL_UNIT_ASSIGNED_CONTEXT ( ( #22823, #483, #12662 ) ) REPRESENTATION_CONTEXT ( 'NONE', 'WORKASPACE' ) );
#24259 = CIRCLE ( 'NONE', #9, 1.899999999999999911 ) ;
#24260 = EDGE_CURVE ( 'NONE', #15422, #13616, #28049, .T. ) ;
#24261 = CARTESIAN_POINT ( 'NONE',  ( -59.19702994616205416, -2.078460969082657872, 3.599999999999782041 ) ) ;
#24262 = CARTESIAN_POINT ( 'NONE',  ( 52.41206581543986687, 8.644163850305695007, -2.050000000000182343 ) ) ;
#24263 = DIRECTION ( 'NONE',  ( 0.000000000000000000, 0.000000000000000000, -1.000000000000000000 ) ) ;
#24264 = CARTESIAN_POINT ( 'NONE',  ( 21.97322666366010324, 8.076925076899300393, -1.950000000000076117 ) ) ;
#24265 = CARTESIAN_POINT ( 'NONE',  ( -71.49999999999998579, 0.3062499654112549874, -1.493338310920502066 ) ) ;
#24266 = VECTOR ( 'NONE', #4691, 1000.000000000000000 ) ;
#24268 = CARTESIAN_POINT ( 'NONE',  ( -61.39999999999998437, -2.565822298769830478, -0.8405688140393350327 ) ) ;
#24267 = DIRECTION ( 'NONE',  ( 1.000000000000000000, -0.000000000000000000, -1.047444401652940007E-14 ) ) ;
#24269 = CARTESIAN_POINT ( 'NONE',  ( 51.59739104186227365, 1.010292945603182169, 1.272765950230260401 ) ) ;
#24270 = CARTESIAN_POINT ( 'NONE',  ( 15.71019289815287934, -3.857619034241787759, 3.790808625284011857 ) ) ;
#24272 = CARTESIAN_POINT ( 'NONE',  ( 47.00000000000002132, 2.428612866367529932E-14, -1.640996229256273308E-13 ) ) ;
#24271 = CARTESIAN_POINT ( 'NONE',  ( -59.69999999999997442, 8.366749974758454467E-15, -2.120534355533670266E-13 ) ) ;
#24273 = EDGE_LOOP ( 'NONE', ( #14112, #30781, #23898, #16654, #7374 ) ) ;
#24274 = CARTESIAN_POINT ( 'NONE',  ( 58.66107449606967350, -1.301839550767874165, -1.349793924521847988 ) ) ;
#24275 = CARTESIAN_POINT ( 'NONE',  ( -36.72207054450174724, -5.313409993919712804, -1.009519134730212819 ) ) ;
#24277 = CARTESIAN_POINT ( 'NONE',  ( 51.59739104186229497, -1.010292945602101256, 1.272765950230260623 ) ) ;
#24276 = DIRECTION ( 'NONE',  ( 0.000000000000000000, 0.000000000000000000, 1.000000000000000000 ) ) ;
#24278 = CARTESIAN_POINT ( 'NONE',  ( 63.50000000000002842, 1.401298464324817071E-42, -6.651271950496169736E-13 ) ) ;
#24279 = EDGE_LOOP ( 'NONE', ( #17894, #20789, #23808, #9370 ) ) ;
#24280 = DIRECTION ( 'NONE',  ( 0.000000000000000000, 0.000000000000000000, -1.000000000000000000 ) ) ;
#24281 = AXIS2_PLACEMENT_3D ( 'NONE', #19276, #4681, #12419 ) ;
#24282 = EDGE_CURVE ( 'NONE', #25126, #107, #3217, .T. ) ;
#24283 = ORIENTED_EDGE ( 'NONE', *, *, #12895, .F. ) ;
#24284 = CARTESIAN_POINT ( 'NONE',  ( 22.54717926605044909, 7.740376438784151603, 1.424999999999921663 ) ) ;
#24285 = CARTESIAN_POINT ( 'NONE',  ( -57.63452994616205416, -3.117691453623976816, 1.799999999999783329 ) ) ;
#24286 = EDGE_CURVE ( 'NONE', #25794, #23733, #11367, .T. ) ;
#24287 = VERTEX_POINT ( 'NONE', #26148 ) ;
#24288 = VERTEX_POINT ( 'NONE', #19035 ) ;
#24289 = EDGE_LOOP ( 'NONE', ( #28485, #25897, #19543, #526 ) ) ;
#24290 = VECTOR ( 'NONE', #11475, 1000.000000000000000 ) ;
#24291 = DIRECTION ( 'NONE',  ( 9.754918421198724481E-16, -0.9601771338024399638, 0.2793919678926571892 ) ) ;
#24292 = CARTESIAN_POINT ( 'NONE',  ( -54.82202994616206126, 2.078460969082646770, 3.599999999999812683 ) ) ;
#24293 = EDGE_LOOP ( 'NONE', ( #24963, #6926, #9619, #20205 ) ) ;
#24294 = CARTESIAN_POINT ( 'NONE',  ( 54.41118797001386298, -1.084202172485505913E-16, 4.375000000000000000 ) ) ;
#24295 = CARTESIAN_POINT ( 'NONE',  ( 51.80000048712015115, 3.919471099442191520, -2.045252491637605807 ) ) ;
#24296 = CARTESIAN_POINT ( 'NONE',  ( 30.67843166873835159, 7.122989987860218974, 2.049999999999892353 ) ) ;
#24297 = VERTEX_POINT ( 'NONE', #21576 ) ;
#24298 = ADVANCED_FACE ( 'NONE', ( #12210 ), #31218, .T. ) ;
#24299 = CARTESIAN_POINT ( 'NONE',  ( 51.79427239975815667, -4.149162114478044394, -1.064915450748001646 ) ) ;
#24300 = DIRECTION ( 'NONE',  ( 1.000000000000000000, -1.805490781531623600E-17, 1.716160222047040134E-16 ) ) ;
#24301 = CARTESIAN_POINT ( 'NONE',  ( 58.65000038048066955, -1.008797009995799465, -1.580579251835824595 ) ) ;
#24302 = CARTESIAN_POINT ( 'NONE',  ( -59.69999999999996021, 1.397030005794335672, -3.099726949734703751 ) ) ;
#24303 = CARTESIAN_POINT ( 'NONE',  ( 58.65000000000001279, 0.5540123067551541158, -1.791510860174695408 ) ) ;
#24304 = APPLICATION_CONTEXT ( 'automotive_design' ) ;
#24306 = LINE ( 'NONE', #22098, #25524 ) ;
#24305 = PLANE ( 'NONE',  #15979 ) ;
#24307 = EDGE_CURVE ( 'NONE', #16732, #2659, #10352, .T. ) ;
#24308 = CIRCLE ( 'NONE', #9657, 1.625000000000000444 ) ;
#24309 = CARTESIAN_POINT ( 'NONE',  ( 51.34893360928145256, 1.002183861493406436, 1.396106892655430753 ) ) ;
#24310 = CARTESIAN_POINT ( 'NONE',  ( 52.06628335902944826, 0.5434431642986571331, -1.794517909405660694 ) ) ;
#24311 = CARTESIAN_POINT ( 'NONE',  ( 53.60047708782985865, 7.640852521089519733, 1.861455469535095331 ) ) ;
#24312 = ORIENTED_EDGE ( 'NONE', *, *, #8784, .F. ) ;
#24313 = VERTEX_POINT ( 'NONE', #19204 ) ;
#24314 = EDGE_CURVE ( 'NONE', #24734, #11521, #1758, .T. ) ;
#24315 = ORIENTED_EDGE ( 'NONE', *, *, #4581, .F. ) ;
#24316 = EDGE_CURVE ( 'NONE', #1935, #7270, #9369, .T. ) ;
#24317 = CARTESIAN_POINT ( 'NONE',  ( 52.11563210330035645, 3.836792880204552336, 2.049999999999818190 ) ) ;
#24318 = CARTESIAN_POINT ( 'NONE',  ( -54.54792740578361077, -1.073804522883516688, -3.225979517392336238 ) ) ;
#24320 = DIRECTION ( 'NONE',  ( 0.000000000000000000, 0.000000000000000000, 1.000000000000000000 ) ) ;
#24319 = CARTESIAN_POINT ( 'NONE',  ( -54.68749999999998579, -3.925981830489445379, -2.085002746943179415E-13 ) ) ;
#24321 = EDGE_CURVE ( 'NONE', #16500, #18983, #4795, .T. ) ;
#24322 = ORIENTED_EDGE ( 'NONE', *, *, #2200, .T. ) ;
#24323 = ORIENTED_EDGE ( 'NONE', *, *, #18414, .F. ) ;
#24324 = FACE_OUTER_BOUND ( 'NONE', #12004, .T. ) ;
#24325 = ORIENTED_EDGE ( 'NONE', *, *, #15982, .F. ) ;
#24326 = CARTESIAN_POINT ( 'NONE',  ( 27.27214205000343483, 5.011961650406414392, 1.949999999999904254 ) ) ;
#24327 = EDGE_LOOP ( 'NONE', ( #22768, #28292, #15209, #31033 ) ) ;
#24328 = CARTESIAN_POINT ( 'NONE',  ( 30.93618511144916994, 7.271541257249353407, -2.050000000000106848 ) ) ;
#24329 = CIRCLE ( 'NONE', #14712, 4.000000000000000000 ) ;
#24330 = B_SPLINE_CURVE_WITH_KNOTS ( 'NONE', 3,
 ( #17032, #4986, #14639, #21943, #5452, #20018, #17480, #12562, #24759, #7665, #5133, #27132, #22396, #3389, #13035, #29208 ),
 .UNSPECIFIED., .F., .F.,
 ( 4, 3, 3, 3, 3, 4 ),
 ( 0.000000000000000000, 1.625241835515689952E-05, 3.292491922809579385E-05, 5.060195339673861708E-05, 6.961003767230190245E-05, 8.476187580399473969E-05 ),
 .UNSPECIFIED. ) ;
#24331 = CARTESIAN_POINT ( 'NONE',  ( 51.12687253673781385, -0.9194130538815391551, 1.491219977510798600 ) ) ;
#24332 = CARTESIAN_POINT ( 'NONE',  ( 60.75000000000002842, -0.4999999999993638977, -1.718465885608440047 ) ) ;
#24333 = EDGE_CURVE ( 'NONE', #15675, #865, #258, .T. ) ;
#24334 = CARTESIAN_POINT ( 'NONE',  ( -55.33155989232414385, -1.962990915244731571, 3.399999999999794742 ) ) ;
#24335 = CARTESIAN_POINT ( 'NONE',  ( 53.78456803694539445, 5.661108390837276794, -1.682988280464833286 ) ) ;
#24336 = SPHERICAL_SURFACE ( 'NONE', #9930, 0.1000000000000000056 ) ;
#24337 = DIRECTION ( 'NONE',  ( 1.000000000000000000, 0.000000000000000000, 0.000000000000000000 ) ) ;
#24338 = EDGE_CURVE ( 'NONE', #2901, #28072, #6835, .T. ) ;
#24339 = DIRECTION ( 'NONE',  ( 1.000000000000000000, -1.219044193948983948E-29, 3.491481338843133355E-15 ) ) ;
#24341 = EDGE_CURVE ( 'NONE', #20831, #2488, #8824, .T. ) ;
#24340 = FACE_OUTER_BOUND ( 'NONE', #24273, .T. ) ;
#24342 = ORIENTED_EDGE ( 'NONE', *, *, #10851, .F. ) ;
#24343 = CARTESIAN_POINT ( 'NONE',  ( 57.00873807961998097, -0.7491996424029042645, -2.489992076190610248 ) ) ;
#24344 = CARTESIAN_POINT ( 'NONE',  ( -36.56390771145616725, -3.008101665203226638, -4.495550615867749400 ) ) ;
#24345 = CARTESIAN_POINT ( 'NONE',  ( 53.90734097010463444, 6.075402212724766216, 1.402257142663977607 ) ) ;
#24346 = ORIENTED_EDGE ( 'NONE', *, *, #21686, .T. ) ;
#24347 = DIRECTION ( 'NONE',  ( 1.000000000000000000, -1.219044193948983948E-29, 3.491481338843133355E-15 ) ) ;
#24348 = VERTEX_POINT ( 'NONE', #28991 ) ;
#24349 = EDGE_CURVE ( 'NONE', #30905, #18829, #9637, .T. ) ;
#24350 = CARTESIAN_POINT ( 'NONE',  ( 15.98305126557428579, 0.5375162698823215957, -5.381098085087392846 ) ) ;
#24351 = CARTESIAN_POINT ( 'NONE',  ( 58.64999999999999858, 1.671477153795419390, -0.8495817349390374362 ) ) ;
#24353 = CARTESIAN_POINT ( 'NONE',  ( 60.75000000000002842, -0.4999999999993638977, 1.546164609606623053 ) ) ;
#24352 = CARTESIAN_POINT ( 'NONE',  ( 50.80000000000002558, -4.387164041431067751, 1.383037119376580693 ) ) ;
#24354 = EDGE_CURVE ( 'NONE', #26583, #14688, #4154, .T. ) ;
#24355 = VERTEX_POINT ( 'NONE', #11590 ) ;
#24356 = DIRECTION ( 'NONE',  ( -1.000000000000000000, 0.000000000000000000, 0.000000000000000000 ) ) ;
#24357 = CARTESIAN_POINT ( 'NONE',  ( 58.45000000000001705, -0.8000000000000000444, 2.421260002560649660 ) ) ;
#24358 = AXIS2_PLACEMENT_3D ( 'NONE', #10664, #19861, #17803 ) ;
#24360 = DIRECTION ( 'NONE',  ( 1.000000000000000000, -1.219044193948983948E-29, 3.491481338843133355E-15 ) ) ;
#24359 = CARTESIAN_POINT ( 'NONE',  ( 69.23535533905932482, 3.976613875667303688E-16, -2.764644660941391052 ) ) ;
#24361 = ORIENTED_EDGE ( 'NONE', *, *, #2155, .T. ) ;
#24362 = CARTESIAN_POINT ( 'NONE',  ( -57.68749999999996447, 0.8699069336946685382, -4.241846523238428368 ) ) ;
#24363 = DIRECTION ( 'NONE',  ( 0.000000000000000000, 0.9996898646859344595, 0.02490330187381124133 ) ) ;
#24364 = CARTESIAN_POINT ( 'NONE',  ( 51.31572262954152563, 1.002608958138273554, -1.584424273060082378 ) ) ;
#24365 = CARTESIAN_POINT ( 'NONE',  ( 15.03925126672132961, -2.199885893005931070, -4.939696249117691451 ) ) ;
#24366 = AXIS2_PLACEMENT_3D ( 'NONE', #2015, #18968, #11680 ) ;
#24367 = CARTESIAN_POINT ( 'NONE',  ( -54.68749999999997868, 0.7533615035078081723, -3.673546848079177973 ) ) ;
#24368 = PLANE ( 'NONE',  #22805 ) ;
#24369 = DIRECTION ( 'NONE',  ( -2.614381936396368743E-16, 0.2008964009354147762, -0.9796124928211139560 ) ) ;
#24370 = ORIENTED_EDGE ( 'NONE', *, *, #329, .T. ) ;
#24371 = FACE_OUTER_BOUND ( 'NONE', #22476, .T. ) ;
#24372 = CARTESIAN_POINT ( 'NONE',  ( -44.59999999999999432, 1.399999999999995914, 3.959797974644454488 ) ) ;
#24373 = ADVANCED_FACE ( 'NONE', ( #21271 ), #14106, .T. ) ;
#24374 = EDGE_CURVE ( 'NONE', #24537, #5072, #5070, .T. ) ;
#24375 = CARTESIAN_POINT ( 'NONE',  ( 48.50000000000002132, 1.409787217987196861, -3.850000000000022737 ) ) ;
#24377 = EDGE_CURVE ( 'NONE', #3532, #28342, #7755, .T. ) ;
#24376 = DIRECTION ( 'NONE',  ( 0.000000000000000000, 1.000000000000000000, 3.491481338843133355E-15 ) ) ;
#24378 = AXIS2_PLACEMENT_3D ( 'NONE', #13064, #3095, #25093 ) ;
#24379 = DIRECTION ( 'NONE',  ( 0.000000000000000000, 0.9495137264943719346, -0.3137254901960807585 ) ) ;
#24381 = CARTESIAN_POINT ( 'NONE',  ( -44.59999999999995879, -1.499999999999978684, -4.029888335922158227 ) ) ;
#24380 = DIRECTION ( 'NONE',  ( 1.189524669241238948E-14, 0.000000000000000000, 1.000000000000000000 ) ) ;
#24382 = VERTEX_POINT ( 'NONE', #21888 ) ;
#24383 = CARTESIAN_POINT ( 'NONE',  ( 58.74999981404335614, -1.865327579933669710, 0.5879486190978074900 ) ) ;
#24384 = ORIENTED_EDGE ( 'NONE', *, *, #8144, .T. ) ;
#24385 = UNCERTAINTY_MEASURE_WITH_UNIT (LENGTH_MEASURE( 1.000000000000000082E-05 ), #13495, 'distance_accuracy_value', 'NONE');
#24386 = CARTESIAN_POINT ( 'NONE',  ( 58.65000000000003411, -1.022750809560713181, -1.571497941946363497 ) ) ;
#24388 = DIRECTION ( 'NONE',  ( 0.000000000000000000, -1.000000000000000000, -3.491481338843137694E-15 ) ) ;
#24387 = CARTESIAN_POINT ( 'NONE',  ( 15.68751737981894934, -2.884962146574149511, -4.577321775072947574 ) ) ;
#24389 = DIRECTION ( 'NONE',  ( 0.7313537016191670181, 0.6819983600625023623, -2.468850131082252722E-15 ) ) ;
#24390 = EDGE_LOOP ( 'NONE', ( #10789, #13808, #4147, #11217 ) ) ;
#24391 = VERTEX_POINT ( 'NONE', #10145 ) ;
#24392 = CARTESIAN_POINT ( 'NONE',  ( -57.31684846062113792, -0.2309624077929026409, -3.875409454552791733 ) ) ;
#24393 = ORIENTED_EDGE ( 'NONE', *, *, #28816, .F. ) ;
#24394 = LINE ( 'NONE', #17420, #13493 ) ;
#24395 = DIRECTION ( 'NONE',  ( -7.401486830834382195E-15, 0.000000000000000000, -1.000000000000000000 ) ) ;
#24396 = AXIS2_PLACEMENT_3D ( 'NONE', #9798, #6736, #23848 ) ;
#24397 = CARTESIAN_POINT ( 'NONE',  ( -36.30347965937280463, -4.980680447166691671, -1.498595263773966790 ) ) ;
#24398 = ORIENTED_EDGE ( 'NONE', *, *, #23059, .F. ) ;
#24399 = SURFACE_SIDE_STYLE ('',( #2232 ) ) ;
#24400 = CARTESIAN_POINT ( 'NONE',  ( 58.73379417893114152, -1.381558089341666795, -1.267842757871614490 ) ) ;
#24401 =( NAMED_UNIT ( * ) PLANE_ANGLE_UNIT ( ) SI_UNIT ( $, .RADIAN. ) );
#24402 = VERTEX_POINT ( 'NONE', #19810 ) ;
#24403 = CARTESIAN_POINT ( 'NONE',  ( -58.69702994616204705, 4.156921938165313080, -1.932741547809596393E-13 ) ) ;
#24404 = CARTESIAN_POINT ( 'NONE',  ( 50.33625478868709990, 1.419210040599422795, 3.846553521706499446 ) ) ;
#24405 = DIRECTION ( 'NONE',  ( 0.000000000000000000, -0.5333333333333335480, -0.8459051693633012903 ) ) ;
#24406 = CARTESIAN_POINT ( 'NONE',  ( -54.45495050826418293, -1.500000000000000000, 3.300094695611020867 ) ) ;
#24407 = CARTESIAN_POINT ( 'NONE',  ( 51.87921884176515164, -4.254539148539595139, -1.020319270753726526 ) ) ;
#24408 = ADVANCED_FACE ( 'NONE', ( #27391 ), #12874, .T. ) ;
#24409 = DIRECTION ( 'NONE',  ( 0.000000000000000000, 1.000000000000000000, 3.491481338843130594E-15 ) ) ;
#24412 = EDGE_CURVE ( 'NONE', #3198, #15422, #12346, .T. ) ;
#24411 = CARTESIAN_POINT ( 'NONE',  ( -36.89250464418362441, 0.3169205264057852189, -5.400007398663901448 ) ) ;
#24410 = DIRECTION ( 'NONE',  ( 1.000000000000000000, -1.219044193948983948E-29, 3.491481338843133355E-15 ) ) ;
#24413 = AXIS2_PLACEMENT_3D ( 'NONE', #3860, #20673, #11141 ) ;
#24414 = DIRECTION ( 'NONE',  ( 1.000000000000000000, -1.219044193948983948E-29, 3.491481338843133355E-15 ) ) ;
#24416 = CARTESIAN_POINT ( 'NONE',  ( 57.05000000000001847, -0.8156862745098039102, 2.468735688885368873 ) ) ;
#24415 = CARTESIAN_POINT ( 'NONE',  ( 15.41586008885035319, 4.863061488092564666, -1.860589201779632607 ) ) ;
#24417 = ORIENTED_EDGE ( 'NONE', *, *, #18229, .T. ) ;
#24418 = CARTESIAN_POINT ( 'NONE',  ( 51.80000000000001137, 4.350000000000017408, -1.495827530165608321 ) ) ;
#24419 = DIRECTION ( 'NONE',  ( -1.000000000000000000, 1.219044193948983948E-29, -3.491481338843133355E-15 ) ) ;
#24421 = DIRECTION ( 'NONE',  ( 1.000000000000000000, 4.678365685400793326E-16, -1.520093157366863638E-16 ) ) ;
#24420 = CARTESIAN_POINT ( 'NONE',  ( 48.40000000000002700, -0.6462379109120522935, 4.048750000000028493 ) ) ;
#24422 = CARTESIAN_POINT ( 'NONE',  ( 47.21160823903058912, -4.227734780419093674, 1.816236823409400847 ) ) ;
#24423 = VERTEX_POINT ( 'NONE', #176 ) ;
#24424 = CARTESIAN_POINT ( 'NONE',  ( -61.36293602036113271, -2.641650077464329005, 0.4741806564687899295 ) ) ;
#24425 = ADVANCED_FACE ( 'NONE', ( #9998 ), #20136, .T. ) ;
#24426 = ORIENTED_EDGE ( 'NONE', *, *, #4637, .F. ) ;
#24427 = CARTESIAN_POINT ( 'NONE',  ( -59.69999999999997442, 8.366749974758454467E-15, -2.120534355533670266E-13 ) ) ;
#24428 = ORIENTED_EDGE ( 'NONE', *, *, #11136, .T. ) ;
#24429 = ORIENTED_EDGE ( 'NONE', *, *, #21348, .T. ) ;
#24430 = DIRECTION ( 'NONE',  ( -0.000000000000000000, -0.000000000000000000, 1.000000000000000000 ) ) ;
#24431 = VERTEX_POINT ( 'NONE', #22343 ) ;
#24432 = CARTESIAN_POINT ( 'NONE',  ( 52.01765327766486280, 4.368296548649880151, 1.441525720016375134 ) ) ;
#24433 = CARTESIAN_POINT ( 'NONE',  ( -54.88452994616206126, 3.117691453623979481, 1.799999999999816858 ) ) ;
#24434 = VERTEX_POINT ( 'NONE', #19961 ) ;
#24435 = CARTESIAN_POINT ( 'NONE',  ( 54.46244440770933437, -0.0007103938889471558219, 4.353106894003209604 ) ) ;
#24436 = AXIS2_PLACEMENT_3D ( 'NONE', #8185, #10567, #15462 ) ;
#24437 = DIRECTION ( 'NONE',  ( -1.000000000000000000, 1.219044193948983948E-29, -3.491481338843133355E-15 ) ) ;
#24438 = CIRCLE ( 'NONE', #3703, 2.649999999999999911 ) ;
#24439 = CARTESIAN_POINT ( 'NONE',  ( 26.91641317417657220, 5.349067879198667441, 2.049999999999906564 ) ) ;
#24440 = ORIENTED_EDGE ( 'NONE', *, *, #6268, .F. ) ;
#24441 = CARTESIAN_POINT ( 'NONE',  ( -74.39999999999997726, -1.239615432210561474, -0.03088009432352123093 ) ) ;
#24442 = CARTESIAN_POINT ( 'NONE',  ( -54.49409853110120139, -1.525884777627347644, 4.047834655405393889 ) ) ;
#24443 = CARTESIAN_POINT ( 'NONE',  ( 53.81464057712624793, 5.799094425976102585, -2.050000000000187228 ) ) ;
#24444 = CARTESIAN_POINT ( 'NONE',  ( -59.51007810423286770, -3.208491484513371628, -1.128887151816144963 ) ) ;
#24445 = DIRECTION ( 'NONE',  ( 0.000000000000000000, 1.000000000000000000, 3.491481338843130594E-15 ) ) ;
#24446 = EDGE_CURVE ( 'NONE', #25040, #28523, #13362, .T. ) ;
#24448 = CARTESIAN_POINT ( 'NONE',  ( 58.65266784251146959, -0.9945725797245054123, 1.589569034372780854 ) ) ;
#24447 = CARTESIAN_POINT ( 'NONE',  ( 57.00000000000001421, 0.7500000000000000000, 3.499999999999999556 ) ) ;
#24449 = DIRECTION ( 'NONE',  ( 0.000000000000000000, -0.2008964009354147484, 0.9796124928211139560 ) ) ;
#24450 = DIRECTION ( 'NONE',  ( 0.000000000000000000, 0.9996898646859344595, 0.02490330187381105745 ) ) ;
#24451 = CARTESIAN_POINT ( 'NONE',  ( 52.82099478266074755, 4.588601447596447613, 1.578939844535152570 ) ) ;
#24452 = CIRCLE ( 'NONE', #27995, 0.1000000000000000472 ) ;
#24453 = EDGE_LOOP ( 'NONE', ( #5069, #25502, #26698, #4865, #27530, #17122, #10958, #17496, #6830, #20972, #870, #2622 ) ) ;
#24454 = EDGE_LOOP ( 'NONE', ( #15888, #19252, #14664, #4032 ) ) ;
#24455 = ADVANCED_FACE ( 'NONE', ( #9832 ), #18151, .T. ) ;
#24456 = ORIENTED_EDGE ( 'NONE', *, *, #16041, .F. ) ;
#24457 = CARTESIAN_POINT ( 'NONE',  ( -62.06710100716625789, -2.517118187348250213, 0.1993515260053453086 ) ) ;
#24458 = CARTESIAN_POINT ( 'NONE',  ( -56.36042740578360366, -0.7887156198831599685, 3.845940847736173840 ) ) ;
#24460 = FACE_OUTER_BOUND ( 'NONE', #30828, .T. ) ;
#24459 = CYLINDRICAL_SURFACE ( 'NONE', #14532, 2.000000000000000000 ) ;
#24461 = ORIENTED_EDGE ( 'NONE', *, *, #31034, .T. ) ;
#24462 = EDGE_LOOP ( 'NONE', ( #3233, #18732, #6622, #30948 ) ) ;
#24463 = CARTESIAN_POINT ( 'NONE',  ( 53.81450004168215173, 5.799141575175360330, -1.730551853729838774 ) ) ;
#24464 = VERTEX_POINT ( 'NONE', #30455 ) ;
#24465 = CARTESIAN_POINT ( 'NONE',  ( 50.25000000000002842, -0.4999999999994738653, 1.863080903344643380 ) ) ;
#24466 = EDGE_LOOP ( 'NONE', ( #16622, #4102, #31220, #19921 ) ) ;
#24467 = CARTESIAN_POINT ( 'NONE',  ( 27.54696499484732186, 5.363421040470059076, -2.050000000000028244 ) ) ;
#24468 =( BOUNDED_CURVE ( )  B_SPLINE_CURVE ( 2, ( #26886, #2816, #12471, #22162, #450, #19780, #27032, #5342, #24673 ),
 .UNSPECIFIED., .F., .T. ) 
 B_SPLINE_CURVE_WITH_KNOTS ( ( 3, 2, 2, 2, 3 ),
 ( 0.08333333333333332871, 0.09259259259259258745, 0.1111111111111111049, 0.1296296296296296224, 0.1388888888888888951 ),
 .UNSPECIFIED. ) 
 CURVE ( )  GEOMETRIC_REPRESENTATION_ITEM ( )  RATIONAL_B_SPLINE_CURVE ( ( 0.9330127018922194093, 0.9330127018922194093, 1.000000000000000000, 0.8660254037844387076, 1.000000000000000000, 0.8660254037844387076, 1.000000000000000000, 0.9330127018922191873, 0.9330127018922192983 ) ) 
 REPRESENTATION_ITEM ( '' )  );
#24469 = ORIENTED_EDGE ( 'NONE', *, *, #12019, .T. ) ;
#24470 = CARTESIAN_POINT ( 'NONE',  ( 51.12687253673779253, 0.9194130538826112975, -1.491219977510798378 ) ) ;
#24471 = DIRECTION ( 'NONE',  ( 0.000000000000000000, 0.000000000000000000, -1.000000000000000000 ) ) ;
#24472 = CARTESIAN_POINT ( 'NONE',  ( 15.87128154250934031, -5.321612844166236478, -0.9647713018064705270 ) ) ;
#24474 = CARTESIAN_POINT ( 'NONE',  ( -56.45655989232411542, 1.962990915244748891, -3.400000000000191314 ) ) ;
#24473 = AXIS2_PLACEMENT_3D ( 'NONE', #16623, #9656, #5188 ) ;
#24475 = CARTESIAN_POINT ( 'NONE',  ( 53.60227722476024326, 4.617096236911465645, -2.050000000000186784 ) ) ;
#24476 = EDGE_CURVE ( 'NONE', #26160, #8007, #19826, .T. ) ;
#24477 = CARTESIAN_POINT ( 'NONE',  ( 50.31877865969198638, 1.391940262981064214, -3.850000000000022293 ) ) ;
#24478 = ADVANCED_FACE ( 'NONE', ( #11294 ), #4027, .F. ) ;
#24479 = AXIS2_PLACEMENT_3D ( 'NONE', #11133, #3113, #1477 ) ;
#24480 = CARTESIAN_POINT ( 'NONE',  ( 16.10667815269233216, -5.098435263432253173, -1.807398698456192276 ) ) ;
#24481 = ORIENTED_EDGE ( 'NONE', *, *, #3844, .T. ) ;
#24482 = LINE ( 'NONE', #2792, #22538 ) ;
#24483 = EDGE_LOOP ( 'NONE', ( #12380, #17379, #21776, #19493 ) ) ;
#24484 = FACE_OUTER_BOUND ( 'NONE', #24648, .T. ) ;
#24485 = FACE_OUTER_BOUND ( 'NONE', #2599, .T. ) ;
#24486 = CARTESIAN_POINT ( 'NONE',  ( 54.22158129257385184, 6.014404448109268664, 2.049999999999810640 ) ) ;
#24487 = ORIENTED_EDGE ( 'NONE', *, *, #670, .F. ) ;
#24488 = EDGE_CURVE ( 'NONE', #28519, #1074, #20527, .T. ) ;
#24489 = FACE_OUTER_BOUND ( 'NONE', #7437, .T. ) ;
#24490 = ORIENTED_EDGE ( 'NONE', *, *, #30108, .F. ) ;
#24491 = DIRECTION ( 'NONE',  ( 0.000000000000000000, 1.000000000000000000, 3.491481338843130594E-15 ) ) ;
#24492 = AXIS2_PLACEMENT_3D ( 'NONE', #8504, #20863, #25907 ) ;
#24493 = CARTESIAN_POINT ( 'NONE',  ( 48.43326094847141405, 1.398826622412688403, 3.854114288381606190 ) ) ;
#24495 = SPHERICAL_SURFACE ( 'NONE', #16159, 0.05000000000000000278 ) ;
#24494 = CARTESIAN_POINT ( 'NONE',  ( 58.65000000000000568, 1.022750809560621921, 1.571497941947222587 ) ) ;
#24496 = ORIENTED_EDGE ( 'NONE', *, *, #4763, .F. ) ;
#24497 = FACE_OUTER_BOUND ( 'NONE', #11377, .T. ) ;
#24498 = DIRECTION ( 'NONE',  ( -1.000000000000000000, 1.219044193948983948E-29, -3.491481338843133355E-15 ) ) ;
#24500 = CARTESIAN_POINT ( 'NONE',  ( -54.49998548284560940, -1.548795215916124013, -4.063650232134933482 ) ) ;
#24499 = CARTESIAN_POINT ( 'NONE',  ( 53.02535680938098039, 4.241071265092343445, 2.047386379460785388 ) ) ;
#24501 = LINE ( 'NONE', #7874, #11995 ) ;
#24502 = CARTESIAN_POINT ( 'NONE',  ( -58.81249999999996447, -0.8699069336946627651, 4.241846523238428368 ) ) ;
#24503 = CARTESIAN_POINT ( 'NONE',  ( -35.85663232820584057, 0.000000000000000000, 5.200000000000000178 ) ) ;
#24504 = EDGE_CURVE ( 'NONE', #1976, #27508, #4314, .T. ) ;
#24505 = CARTESIAN_POINT ( 'NONE',  ( -55.31249999999995737, -1.962990915244704260, -3.400000000000204636 ) ) ;
#24506 = CARTESIAN_POINT ( 'NONE',  ( 48.99999999999999289, 1.401298464324817071E-42, -2.875000000000512035 ) ) ;
#24507 = FACE_OUTER_BOUND ( 'NONE', #24390, .T. ) ;
#24508 = DIRECTION ( 'NONE',  ( -3.489354422748178582E-15, 1.218509414717996338E-16, -1.000000000000000000 ) ) ;
#24509 = AXIS2_PLACEMENT_3D ( 'NONE', #17965, #27614, #5942 ) ;
#24511 = ORIENTED_EDGE ( 'NONE', *, *, #10653, .T. ) ;
#24510 = AXIS2_PLACEMENT_3D ( 'NONE', #14393, #24064, #25419 ) ;
#24512 = EDGE_CURVE ( 'NONE', #6647, #10074, #30594, .T. ) ;
#24513 = CARTESIAN_POINT ( 'NONE',  ( 15.74504787372189263, -3.350344226587724794, 4.246692235171886765 ) ) ;
#24514 = ADVANCED_FACE ( 'NONE', ( #23498 ), #18766, .F. ) ;
#24515 = CIRCLE ( 'NONE', #5302, 5.100000000000000533 ) ;
#24516 = CARTESIAN_POINT ( 'NONE',  ( 24.67796800286685510, 5.428620075164593217, -1.950000000000086109 ) ) ;
#24517 = EDGE_CURVE ( 'NONE', #7259, #30552, #9098, .T. ) ;
#24518 = DIRECTION ( 'NONE',  ( 2.775557561562891351E-14, -1.000000000000000000, 0.000000000000000000 ) ) ;
#24519 = AXIS2_PLACEMENT_3D ( 'NONE', #4923, #9692, #2399 ) ;
#24520 = DIRECTION ( 'NONE',  ( -1.000000000000000000, -0.000000000000000000, 3.491481338843133355E-15 ) ) ;
#24521 = CARTESIAN_POINT ( 'NONE',  ( 69.25000000000004263, -0.7500000000000000000, 1.988246715072632620 ) ) ;
#24523 = CARTESIAN_POINT ( 'NONE',  ( 30.21341079104190186, 6.695592610073531681, 1.424999999999893907 ) ) ;
#24522 = CARTESIAN_POINT ( 'NONE',  ( 58.72200907981798679, 0.5299537992503529082, 1.799145225589759756 ) ) ;
#24524 = ORIENTED_EDGE ( 'NONE', *, *, #15658, .F. ) ;
#24525 = FACE_OUTER_BOUND ( 'NONE', #13055, .T. ) ;
#24526 = VERTEX_POINT ( 'NONE', #27358 ) ;
#24527 = FACE_OUTER_BOUND ( 'NONE', #19115, .T. ) ;
#24529 = DIRECTION ( 'NONE',  ( 1.000000000000000000, 1.047444401652940007E-14, 0.000000000000000000 ) ) ;
#24528 = CARTESIAN_POINT ( 'NONE',  ( 15.49702763512083870, -3.100731772197800495, -4.174739983989899095 ) ) ;
#24530 = CARTESIAN_POINT ( 'NONE',  ( -62.09999999999997300, -2.625757682666624238, -0.2804666419185134485 ) ) ;
#24531 = VERTEX_POINT ( 'NONE', #929 ) ;
#24532 = AXIS2_PLACEMENT_3D ( 'NONE', #3391, #22722, #13184 ) ;
#24533 = VERTEX_POINT ( 'NONE', #21153 ) ;
#24534 = DIRECTION ( 'NONE',  ( 0.000000000000000000, 0.000000000000000000, 1.000000000000000000 ) ) ;
#24535 = AXIS2_PLACEMENT_3D ( 'NONE', #816, #15072, #13154 ) ;
#24536 = CARTESIAN_POINT ( 'NONE',  ( 52.20711756518982583, 0.6500000000005481393, 1.489337100860647523 ) ) ;
#24537 = VERTEX_POINT ( 'NONE', #15481 ) ;
#24538 = DIRECTION ( 'NONE',  ( 0.000000000000000000, -0.9996898646859343485, -0.02490330187381124133 ) ) ;
#24539 = CARTESIAN_POINT ( 'NONE',  ( -55.48542740578360366, -3.725040285533364859, 1.239922660687674760 ) ) ;
#24540 = ADVANCED_FACE ( 'NONE', ( #12935 ), #17457, .T. ) ;
#24541 = CARTESIAN_POINT ( 'NONE',  ( -59.61316801158443468, -2.161784001863006566, 1.533130796914948801 ) ) ;
#24542 = VERTEX_POINT ( 'NONE', #1793 ) ;
#24543 = CARTESIAN_POINT ( 'NONE',  ( 0.000000000000000000, 0.000000000000000000, 0.000000000000000000 ) ) ;
#24544 = VECTOR ( 'NONE', #30954, 1000.000000000000000 ) ;
#24545 = CARTESIAN_POINT ( 'NONE',  ( 48.50000000000002132, -1.391941090707485396, -3.850000000000022737 ) ) ;
#24546 = AXIS2_PLACEMENT_3D ( 'NONE', #27539, #25331, #15525 ) ;
#24547 = EDGE_CURVE ( 'NONE', #29149, #4586, #17131, .T. ) ;
#24548 = EDGE_LOOP ( 'NONE', ( #30811, #1062, #13478, #26457 ) ) ;
#24549 = CARTESIAN_POINT ( 'NONE',  ( -59.44702994616203995, 4.156921938165313080, -1.958927657850919798E-13 ) ) ;
#24550 = DIRECTION ( 'NONE',  ( 1.000000000000000000, -1.219044193948983948E-29, 3.491481338843133355E-15 ) ) ;
#24551 = CARTESIAN_POINT ( 'NONE',  ( 48.34352038844360777, -1.212999249975891258, -3.917061424767716016 ) ) ;
#24552 = DIRECTION ( 'NONE',  ( -1.000000000000000000, -3.054025858079668409E-16, 2.042474015755241579E-16 ) ) ;
#24553 = DIRECTION ( 'NONE',  ( -1.000000000000000000, -3.054025858079668409E-16, 2.042474015755241579E-16 ) ) ;
#24554 = AXIS2_PLACEMENT_3D ( 'NONE', #13909, #20767, #18380 ) ;
#24555 = DIRECTION ( 'NONE',  ( 3.002035892788117952E-16, -0.9996898646859344595, -0.02490330187381124480 ) ) ;
#24557 = CARTESIAN_POINT ( 'NONE',  ( -61.36066246949631875, -2.556345655048151144, -0.8088090313980157431 ) ) ;
#24556 = CARTESIAN_POINT ( 'NONE',  ( -67.99999999999997158, 0.3264566515200485464, -1.591870300834308471 ) ) ;
#24558 = FACE_OUTER_BOUND ( 'NONE', #14278, .T. ) ;
#24559 = CARTESIAN_POINT ( 'NONE',  ( 15.03925126672132961, -2.199885893005945725, 4.939696249117685234 ) ) ;
#24560 = AXIS2_PLACEMENT_3D ( 'NONE', #12862, #25523, #23180 ) ;
#24562 = CARTESIAN_POINT ( 'NONE',  ( 56.95000043478394502, -0.7674401070440159955, 2.484784916619714679 ) ) ;
#24561 = DIRECTION ( 'NONE',  ( 1.000000000000000000, 3.054025858079668409E-16, -2.042474015755241579E-16 ) ) ;
#24563 = VERTEX_POINT ( 'NONE', #6407 ) ;
#24564 = DIRECTION ( 'NONE',  ( 0.9993908270191184107, -0.03489949670185085034, -3.491481338843133355E-15 ) ) ;
#24565 = AXIS2_PLACEMENT_3D ( 'NONE', #7589, #17248, #12473 ) ;
#24566 = DIRECTION ( 'NONE',  ( 0.000000000000000000, 0.000000000000000000, 1.000000000000000000 ) ) ;
#24568 = CARTESIAN_POINT ( 'NONE',  ( 52.79462163297414889, 4.045128697758171299, -0.6895311692810858206 ) ) ;
#24567 = CARTESIAN_POINT ( 'NONE',  ( 15.57907767661750498, 3.590618801409606320, -4.051716037497242517 ) ) ;
#24569 = CARTESIAN_POINT ( 'NONE',  ( -58.40400635094607651, -3.399999999999988365, -0.9110272542660473594 ) ) ;
#24570 = ORIENTED_EDGE ( 'NONE', *, *, #5168, .F. ) ;
#24571 = CARTESIAN_POINT ( 'NONE',  ( 61.25000000000002842, -0.8716090598184202953, 1.626546686965557820 ) ) ;
#24572 = CIRCLE ( 'NONE', #10919, 0.1000000000000002554 ) ;
#24573 = ORIENTED_EDGE ( 'NONE', *, *, #12718, .T. ) ;
#24574 = CARTESIAN_POINT ( 'NONE',  ( 15.03925126672133139, -4.683225679163343536, 2.703237727951232294 ) ) ;
#24575 = EDGE_LOOP ( 'NONE', ( #172, #9652, #6182, #18639, #31174, #13235 ) ) ;
#24576 = EDGE_LOOP ( 'NONE', ( #11669, #30980, #12467, #7903 ) ) ;
#24577 = ADVANCED_FACE ( 'NONE', ( #28256 ), #10889, .T. ) ;
#24578 = AXIS2_PLACEMENT_3D ( 'NONE', #14981, #30011, #7849 ) ;
#24579 = CARTESIAN_POINT ( 'NONE',  ( 15.67083574136752055, 5.256402525809845905, 1.287848407636934089 ) ) ;
#24580 = VERTEX_POINT ( 'NONE', #8199 ) ;
#24581 = EDGE_CURVE ( 'NONE', #6667, #15786, #11470, .T. ) ;
#24582 = DIRECTION ( 'NONE',  ( 1.000000000000000000, -0.000000000000000000, -0.000000000000000000 ) ) ;
#24583 = CARTESIAN_POINT ( 'NONE',  ( -55.39405989232414385, -3.920666489018348300E-15, 3.399999999999801847 ) ) ;
#24584 = VERTEX_POINT ( 'NONE', #28411 ) ;
#24585 = AXIS2_PLACEMENT_3D ( 'NONE', #25386, #6382, #1471 ) ;
#24586 = CARTESIAN_POINT ( 'NONE',  ( 54.44364453144186911, -0.0003028757503198298978, 4.365665911209477557 ) ) ;
#24587 = ADVANCED_FACE ( 'NONE', ( #4332 ), #22388, .T. ) ;
#24588 = CARTESIAN_POINT ( 'NONE',  ( -71.44999999999998863, -0.4218824419643722456, 2.057186234924342383 ) ) ;
#24589 = VECTOR ( 'NONE', #11311, 1000.000000000000000 ) ;
#24590 = CARTESIAN_POINT ( 'NONE',  ( 58.99999999999998579, 1.401298464324817071E-42, -4.000000000000617284 ) ) ;
#24591 = EDGE_LOOP ( 'NONE', ( #7819, #27212, #28916, #13676 ) ) ;
#24592 = CIRCLE ( 'NONE', #20070, 0.04999999999999991257 ) ;
#24593 = VECTOR ( 'NONE', #22836, 1000.000000000000000 ) ;
#24594 =( BOUNDED_CURVE ( )  B_SPLINE_CURVE ( 2, ( #24367, #19933, #3296, #26888, #29115, #7432, #3140, #22001, #27207 ),
 .UNSPECIFIED., .F., .T. ) 
 B_SPLINE_CURVE_WITH_KNOTS ( ( 3, 2, 2, 2, 3 ),
 ( 0.02777777777777778317, 0.03703703703703703498, 0.05555555555555555247, 0.07407407407407406996, 0.08333333333333332871 ),
 .UNSPECIFIED. ) 
 CURVE ( )  GEOMETRIC_REPRESENTATION_ITEM ( )  RATIONAL_B_SPLINE_CURVE ( ( 0.9330127018922194093, 0.9330127018922194093, 1.000000000000000000, 0.8660254037844387076, 1.000000000000000000, 0.8660254037844387076, 1.000000000000000000, 0.9330127018922194093, 0.9330127018922194093 ) ) 
 REPRESENTATION_ITEM ( '' )  );
#24595 = CARTESIAN_POINT ( 'NONE',  ( 52.20711756518982583, 0.6500000000005479173, -1.489337100860647745 ) ) ;
#24596 = CIRCLE ( 'NONE', #12949, 0.05000000000000012768 ) ;
#24597 = DIRECTION ( 'NONE',  ( 1.000000000000000000, -0.000000000000000000, -1.047444401652940007E-14 ) ) ;
#24598 = CARTESIAN_POINT ( 'NONE',  ( -54.49999999999997868, -1.549999999999999600, -4.064480286580312907 ) ) ;
#24599 = FACE_OUTER_BOUND ( 'NONE', #26524, .T. ) ;
#24600 = CARTESIAN_POINT ( 'NONE',  ( 47.05963571244990362, 8.266527678078146479, -1.950000000000163380 ) ) ;
#24601 = EDGE_CURVE ( 'NONE', #22982, #13311, #12405, .T. ) ;
#24602 = AXIS2_PLACEMENT_3D ( 'NONE', #12882, #8300, #10831 ) ;
#24604 = DIRECTION ( 'NONE',  ( 1.156482317317871449E-14, 0.000000000000000000, 1.000000000000000000 ) ) ;
#24603 =( LENGTH_UNIT ( ) NAMED_UNIT ( * ) SI_UNIT ( .MILLI., .METRE. ) );
#24605 = VECTOR ( 'NONE', #4277, 1000.000000000000000 ) ;
#24606 = CARTESIAN_POINT ( 'NONE',  ( 58.65000000000001279, 0.8495817349399592544, 1.671477153794648673 ) ) ;
#24607 = CARTESIAN_POINT ( 'NONE',  ( 60.75000000000002842, -0.6499999999993638644, -1.489337100860647967 ) ) ;
#24608 = CARTESIAN_POINT ( 'NONE',  ( 58.75000000000000711, 1.320164791810142679, -1.457351493772217843 ) ) ;
#24610 = CARTESIAN_POINT ( 'NONE',  ( 53.78456803694540866, 5.661108390837275905, 1.682988280464426722 ) ) ;
#24609 = VECTOR ( 'NONE', #8248, 1000.000000000000000 ) ;
#24611 = ORIENTED_EDGE ( 'NONE', *, *, #20695, .F. ) ;
#24612 = AXIS2_PLACEMENT_3D ( 'NONE', #27553, #10631, #25018 ) ;
#24613 = AXIS2_PLACEMENT_3D ( 'NONE', #24682, #609, #17254 ) ;
#24614 = ORIENTED_EDGE ( 'NONE', *, *, #2294, .T. ) ;
#24615 = VERTEX_POINT ( 'NONE', #28697 ) ;
#24616 = VECTOR ( 'NONE', #7130, 1000.000000000000000 ) ;
#24617 = DIRECTION ( 'NONE',  ( 0.000000000000000000, 0.000000000000000000, -1.000000000000000000 ) ) ;
#24618 = CARTESIAN_POINT ( 'NONE',  ( -60.48542740578360366, 0.7887156198831658527, -3.845940847736173840 ) ) ;
#24620 = CYLINDRICAL_SURFACE ( 'NONE', #20580, 0.1000000000000000472 ) ;
#24619 = CARTESIAN_POINT ( 'NONE',  ( 58.75000000000002132, 6.153735859711025284E-13, 3.111507638930570854E-58 ) ) ;
#24621 = ORIENTED_EDGE ( 'NONE', *, *, #19945, .F. ) ;
#24622 = ORIENTED_EDGE ( 'NONE', *, *, #20393, .F. ) ;
#24623 = CARTESIAN_POINT ( 'NONE',  ( 51.06423821941617547, -4.410640387330812651, -1.311048612305549144 ) ) ;
#24624 = ORIENTED_EDGE ( 'NONE', *, *, #23568, .T. ) ;
#24625 = EDGE_CURVE ( 'NONE', #1785, #31054, #3304, .T. ) ;
#24626 = CARTESIAN_POINT ( 'NONE',  ( 58.64999999999999858, 1.834410884276226117, 0.3880228184671293268 ) ) ;
#24627 = ORIENTED_EDGE ( 'NONE', *, *, #19611, .T. ) ;
#24628 = CARTESIAN_POINT ( 'NONE',  ( 32.54904120526650502, 8.004085848662747082, -2.050000000000113065 ) ) ;
#24629 = ORIENTED_EDGE ( 'NONE', *, *, #8812, .T. ) ;
#24630 = CARTESIAN_POINT ( 'NONE',  ( -58.18749999999997158, 3.238593381231836155, 2.874284765127033126 ) ) ;
#24631 = AXIS2_PLACEMENT_3D ( 'NONE', #27617, #15747, #5945 ) ;
#24632 = CARTESIAN_POINT ( 'NONE',  ( 57.00000000000001421, -0.6999999999999999556, -2.489477856900920383 ) ) ;
#24633 = ORIENTED_EDGE ( 'NONE', *, *, #22286, .F. ) ;
#24634 = AXIS2_PLACEMENT_3D ( 'NONE', #25786, #13262, #4094 ) ;
#24635 = AXIS2_PLACEMENT_3D ( 'NONE', #13403, #26092, #18353 ) ;
#24636 = DIRECTION ( 'NONE',  ( -1.000000000000000000, -0.000000000000000000, 3.491481338843133355E-15 ) ) ;
#24637 = CARTESIAN_POINT ( 'NONE',  ( -60.57202994616203995, -4.156921938165296204, -2.298664652687300067E-13 ) ) ;
#24638 = CARTESIAN_POINT ( 'NONE',  ( 53.29207122288457299, 4.934008984266801789, -1.614082030464848438 ) ) ;
#24639 = AXIS2_PLACEMENT_3D ( 'NONE', #444, #14999, #10106 ) ;
#24640 = ADVANCED_FACE ( 'NONE', ( #12069 ), #14274, .T. ) ;
#24641 = CARTESIAN_POINT ( 'NONE',  ( 69.20000000000003126, 1.401298464324817071E-42, -7.248315259438346108E-13 ) ) ;
#24642 = AXIS2_PLACEMENT_3D ( 'NONE', #3108, #14397, #17528 ) ;
#24644 = VECTOR ( 'NONE', #26931, 1000.000000000000000 ) ;
#24643 = CARTESIAN_POINT ( 'NONE',  ( -54.49999999999996447, -1.499999999999978906, -3.959797974644881258 ) ) ;
#24645 = CARTESIAN_POINT ( 'NONE',  ( 50.37749466183669256, 1.328329461116619425, -3.879000873601229138 ) ) ;
#24646 = LINE ( 'NONE', #2959, #8867 ) ;
#24647 = CARTESIAN_POINT ( 'NONE',  ( 51.31943556899496173, -1.088761256243092612, 1.206353010735627729 ) ) ;
#24648 = EDGE_LOOP ( 'NONE', ( #27924, #26463, #8147, #19653 ) ) ;
#24649 = AXIS2_PLACEMENT_3D ( 'NONE', #20254, #12932, #15791 ) ;
#24650 = DIRECTION ( 'NONE',  ( 1.000000000000000000, 1.047444401652940007E-14, 0.000000000000000000 ) ) ;
#24651 = CARTESIAN_POINT ( 'NONE',  ( 51.45655683570191741, -0.9591657938390837357, -1.468576096419531574 ) ) ;
#24652 = CARTESIAN_POINT ( 'NONE',  ( 54.31977788970097265, 6.362876281374246545, 2.049999999999810196 ) ) ;
#24653 = ORIENTED_EDGE ( 'NONE', *, *, #10977, .T. ) ;
#24654 = CARTESIAN_POINT ( 'NONE',  ( 50.30000000000001847, 1.426739617975221641, -3.843750000000023093 ) ) ;
#24655 = AXIS2_PLACEMENT_3D ( 'NONE', #9773, #2955, #27330 ) ;
#24656 = ORIENTED_EDGE ( 'NONE', *, *, #10626, .F. ) ;
#24657 =( BOUNDED_SURFACE ( )  B_SPLINE_SURFACE ( 3, 2, ( 
 ( #23089, #6928, #18966 ),
 ( #1384, #6289, #11675 ),
 ( #1537, #21355, #30354 ),
 ( #8660, #18811, #11198 ),
 ( #28455, #6457, #18340 ),
 ( #30982, #1849, #14033 ),
 ( #4221, #20871, #13860 ),
 ( #30498, #8980, #9301 ),
 ( #6759, #23550, #4073 ),
 ( #21200, #6609, #16419 ) ),
 .UNSPECIFIED., .F., .F., .F. ) 
 B_SPLINE_SURFACE_WITH_KNOTS ( ( 4, 2, 2, 2, 4 ),
 ( 3, 3 ),
 ( 0.0001706658715691471151, 0.0002229276920778181924, 0.0002751895125864892697, 0.0003274513330951603742, 0.0003797131536038314244 ),
 ( 0.000000000000000000, 1.000000000000000000 ),
 .UNSPECIFIED. ) 
 GEOMETRIC_REPRESENTATION_ITEM ( )  RATIONAL_B_SPLINE_SURFACE ( (
 ( 1.000000000000000000, 0.7071067811865189290, 1.000000000000000000),
 ( 1.000000000000000000, 0.7375607040702090167, 1.000000000000000000),
 ( 1.000000000000000000, 0.7730431127430185123, 1.000000000000000000),
 ( 1.000000000000000000, 0.8321012486991855583, 1.000000000000000000),
 ( 1.000000000000000000, 0.8541932017417042111, 1.000000000000000000),
 ( 1.000000000000000000, 0.8545723906069231379, 1.000000000000000000),
 ( 1.000000000000000000, 0.8327032135054186490, 1.000000000000000000),
 ( 1.000000000000000000, 0.7734559727066918633, 1.000000000000000000),
 ( 1.000000000000000000, 0.7377766653996046253, 1.000000000000000000),
 ( 1.000000000000000000, 0.7071067811865201502, 1.000000000000000000) ) ) 
 REPRESENTATION_ITEM ( '' )  SURFACE ( )  );
#24658 = CARTESIAN_POINT ( 'NONE',  ( 51.73499623029054106, 4.165486553371512635, 1.939055223349886781 ) ) ;
#24659 = DIRECTION ( 'NONE',  ( 0.000000000000000000, 0.000000000000000000, 1.000000000000000000 ) ) ;
#24660 = DIRECTION ( 'NONE',  ( 1.000000000000000000, 1.047444401652940007E-14, 0.000000000000000000 ) ) ;
#24661 = VERTEX_POINT ( 'NONE', #31225 ) ;
#24662 = B_SPLINE_CURVE_WITH_KNOTS ( 'NONE', 3,
 ( #4241, #3939, #9171, #13580, #18833, #1552 ),
 .UNSPECIFIED., .F., .F.,
 ( 4, 2, 4 ),
 ( 0.000000000000000000, 0.5000000000000000000, 1.000000000000000000 ),
 .UNSPECIFIED. ) ;
#24663 = DIRECTION ( 'NONE',  ( -1.000000000000000000, -0.000000000000000000, -0.000000000000000000 ) ) ;
#24664 = AXIS2_PLACEMENT_3D ( 'NONE', #22416, #559, #18149 ) ;
#24665 = EDGE_CURVE ( 'NONE', #25954, #26805, #19437, .T. ) ;
#24666 = SPHERICAL_SURFACE ( 'NONE', #16056, 0.05000000000000000278 ) ;
#24667 = ORIENTED_EDGE ( 'NONE', *, *, #23870, .F. ) ;
#24669 = CARTESIAN_POINT ( 'NONE',  ( 69.25000000000004263, 0.7500000000000000000, 1.988246715072633064 ) ) ;
#24668 = CARTESIAN_POINT ( 'NONE',  ( -57.86505354137801049, 3.400000000000013678, -0.9110272542659997308 ) ) ;
#24670 = EDGE_LOOP ( 'NONE', ( #24461, #7885, #21962, #23668, #1922, #19703 ) ) ;
#24671 = CARTESIAN_POINT ( 'NONE',  ( -57.31249999999996447, -0.8699069336946624320, 4.241846523238428368 ) ) ;
#24672 = CARTESIAN_POINT ( 'NONE',  ( 56.99280487254718253, -0.7628505807388673565, 1.740142286037820618 ) ) ;
#24673 = CARTESIAN_POINT ( 'NONE',  ( -55.43749999999997868, 0.7533615035078096156, -3.673546848079177529 ) ) ;
#24674 = CARTESIAN_POINT ( 'NONE',  ( 34.50000000000001421, 0.000000000000000000, -3.200000000000000178 ) ) ;
#24675 = DIRECTION ( 'NONE',  ( -1.000000000000000000, -0.000000000000000000, -0.000000000000000000 ) ) ;
#24676 = DIRECTION ( 'NONE',  ( 0.000000000000000000, 0.000000000000000000, -1.000000000000000000 ) ) ;
#24677 = CARTESIAN_POINT ( 'NONE',  ( 52.20711756518984714, -0.6499999999994519051, -1.489337100860648633 ) ) ;
#24678 = VERTEX_POINT ( 'NONE', #14591 ) ;
#24679 = CIRCLE ( 'NONE', #5473, 0.2500000000000002220 ) ;
#24680 = ADVANCED_FACE ( 'NONE', ( #9221 ), #22524, .T. ) ;
#24681 = CARTESIAN_POINT ( 'NONE',  ( 15.48609859788820131, 2.964363692626647673, 4.273817190665822885 ) ) ;
#24682 = CARTESIAN_POINT ( 'NONE',  ( 50.80000000000002558, -4.003661535119149129, 1.269131321891740383 ) ) ;
#24683 = CARTESIAN_POINT ( 'NONE',  ( 52.20711756518982583, 0.7500000000005468959, 1.718465885608440047 ) ) ;
#24684 = EDGE_CURVE ( 'NONE', #27461, #2740, #16462, .T. ) ;
#24685 = CARTESIAN_POINT ( 'NONE',  ( -56.75952994616203995, -3.117691453623960829, -1.800000000000218314 ) ) ;
#24686 = CARTESIAN_POINT ( 'NONE',  ( -56.93749999999996447, 0.7533615035078061739, -3.673546848079177973 ) ) ;
#24688 = FACE_OUTER_BOUND ( 'NONE', #17465, .T. ) ;
#24687 = DIRECTION ( 'NONE',  ( 1.000000000000000000, 1.047444401652940007E-14, 0.000000000000000000 ) ) ;
#24689 = VERTEX_POINT ( 'NONE', #9696 ) ;
#24690 = CARTESIAN_POINT ( 'NONE',  ( 49.05000000000005400, 1.401298464324817071E-42, 2.824999999999485034 ) ) ;
#24691 = ORIENTED_EDGE ( 'NONE', *, *, #5748, .F. ) ;
#24692 = UNCERTAINTY_MEASURE_WITH_UNIT (LENGTH_MEASURE( 1.000000000000000082E-05 ), #5866, 'distance_accuracy_value', 'NONE');
#24693 = PLANE ( 'NONE',  #6002 ) ;
#24695 = CARTESIAN_POINT ( 'NONE',  ( 58.73868664959883290, -0.4999999999993850475, -1.844330893389452219 ) ) ;
#24694 = CARTESIAN_POINT ( 'NONE',  ( 15.03925126672133139, -3.779372838781759558, -3.883777296072569385 ) ) ;
#24696 = EDGE_LOOP ( 'NONE', ( #24922, #21411, #4132, #2030 ) ) ;
#24697 = EDGE_LOOP ( 'NONE', ( #5215, #28808, #10068 ) ) ;
#24698 = FACE_BOUND ( 'NONE', #16587, .T. ) ;
#24699 = MECHANICAL_DESIGN_GEOMETRIC_PRESENTATION_REPRESENTATION (  '', ( #22192 ), #13569 ) ;
#24700 = ADVANCED_FACE ( 'NONE', ( #28996 ), #20188, .F. ) ;
#24701 = LINE ( 'NONE', #30934, #17187 ) ;
#24702 = ORIENTED_EDGE ( 'NONE', *, *, #13274, .T. ) ;
#24703 = CARTESIAN_POINT ( 'NONE',  ( -54.39999999999997726, 1.400000000000009681, -1.886605105831180521E-13 ) ) ;
#24704 = EDGE_CURVE ( 'NONE', #27277, #18051, #2801, .T. ) ;
#24705 = CARTESIAN_POINT ( 'NONE',  ( -54.54999999999998295, 3.780972210569126836E-15, -5.448124817252668230E-16 ) ) ;
#24706 = EDGE_CURVE ( 'NONE', #24164, #26416, #14488, .T. ) ;
#24707 = CARTESIAN_POINT ( 'NONE',  ( 58.75000000000002132, 6.153735859711025284E-13, 3.111507638930570854E-58 ) ) ;
#24708 = DIRECTION ( 'NONE',  ( 0.000000000000000000, 0.000000000000000000, 1.000000000000000000 ) ) ;
#24709 = CARTESIAN_POINT ( 'NONE',  ( 58.74999999305997989, -1.382203543030976034, -1.345908541130527381 ) ) ;
#24710 = ORIENTED_EDGE ( 'NONE', *, *, #4237, .F. ) ;
#24711 = EDGE_CURVE ( 'NONE', #14148, #3532, #1284, .T. ) ;
#24712 = CARTESIAN_POINT ( 'NONE',  ( -57.69702994616206126, -2.078460969082657872, 3.599999999999786926 ) ) ;
#24713 = CARTESIAN_POINT ( 'NONE',  ( 52.41226287506259496, 8.644902628253648302, -2.050000000000182343 ) ) ;
#24714 = CARTESIAN_POINT ( 'NONE',  ( 48.50000000000002132, -1.426739617975179897, -3.843750000000022649 ) ) ;
#24715 = CARTESIAN_POINT ( 'NONE',  ( -54.49998431799114940, -1.548747819918199209, 3.331336553795240185 ) ) ;
#24716 = CARTESIAN_POINT ( 'NONE',  ( 52.13000000000001677, 0.5000000000005460077, -1.996089927833914146 ) ) ;
#24717 = CARTESIAN_POINT ( 'NONE',  ( -58.76905989232410832, 2.523434546734629592E-14, -3.400000000000208189 ) ) ;
#24718 = VECTOR ( 'NONE', #1546, 1000.000000000000000 ) ;
#24720 = CARTESIAN_POINT ( 'NONE',  ( -61.35074562499247008, -2.538044284739583656, -0.7956845220112261918 ) ) ;
#24719 = CARTESIAN_POINT ( 'NONE',  ( 28.63101374161907842, 6.274379892050022001, -1.425000000000099742 ) ) ;
#24721 = EDGE_CURVE ( 'NONE', #9227, #19802, #13738, .T. ) ;
#24722 = PLANE ( 'NONE',  #18547 ) ;
#24723 = LINE ( 'NONE', #504, #14473 ) ;
#24725 = CARTESIAN_POINT ( 'NONE',  ( 57.00000000000001421, -0.7263196003080392149, 2.437012689524181486 ) ) ;
#24724 = CARTESIAN_POINT ( 'NONE',  ( 54.49070678691090563, -0.001831363507897020146, -4.318560329337371329 ) ) ;
#24726 = EDGE_LOOP ( 'NONE', ( #7216, #21240, #20035, #20861 ) ) ;
#24727 = CARTESIAN_POINT ( 'NONE',  ( -62.09999999999997300, 1.168016602258162478E-15, 2.197726754101795588E-15 ) ) ;
#24728 = EDGE_CURVE ( 'NONE', #23987, #12273, #5306, .T. ) ;
#24729 = CARTESIAN_POINT ( 'NONE',  ( 51.76681525450422328, 3.850182003052834201, 1.478406873915413922 ) ) ;
#24730 = VECTOR ( 'NONE', #4730, 1000.000000000000000 ) ;
#24732 = FACE_OUTER_BOUND ( 'NONE', #583, .T. ) ;
#24731 = CARTESIAN_POINT ( 'NONE',  ( 15.49702763512083514, 3.012234853004126300, -4.239036759381555441 ) ) ;
#24733 = CARTESIAN_POINT ( 'NONE',  ( 57.00000000000001421, 0.7000000000000006217, 2.452039967047844993 ) ) ;
#24734 = VERTEX_POINT ( 'NONE', #12350 ) ;
#24735 = DIRECTION ( 'NONE',  ( 3.491481338843133355E-15, 0.000000000000000000, 1.000000000000000000 ) ) ;
#24736 = CARTESIAN_POINT ( 'NONE',  ( 47.08898448364825384, -4.179189514726507682, 0.9999999999999997780 ) ) ;
#24737 = ORIENTED_EDGE ( 'NONE', *, *, #1434, .F. ) ;
#24738 = EDGE_CURVE ( 'NONE', #26017, #11119, #29098, .T. ) ;
#24739 = CYLINDRICAL_SURFACE ( 'NONE', #20994, 3.399999999999999911 ) ;
#24740 = ORIENTED_EDGE ( 'NONE', *, *, #27012, .F. ) ;
#24741 = VERTEX_POINT ( 'NONE', #24545 ) ;
#24742 = ADVANCED_FACE ( 'NONE', ( #2862 ), #12515, .F. ) ;
#24743 = CARTESIAN_POINT ( 'NONE',  ( 15.17256654081411327, 5.086913989685035276, 1.171642050077737585 ) ) ;
#24744 = STYLED_ITEM ( 'NONE', ( #25514 ), #12322 ) ;
#24745 = ORIENTED_EDGE ( 'NONE', *, *, #10790, .F. ) ;
#24746 =( LENGTH_UNIT ( ) NAMED_UNIT ( * ) SI_UNIT ( .MILLI., .METRE. ) );
#24747 = CARTESIAN_POINT ( 'NONE',  ( 31.44149084649588133, 7.421688627196123100, 1.949999999999888933 ) ) ;
#24748 = AXIS2_PLACEMENT_3D ( 'NONE', #1407, #13263, #8370 ) ;
#24749 = CARTESIAN_POINT ( 'NONE',  ( -58.69702994616204705, 4.156921938165313080, -1.932741547809596393E-13 ) ) ;
#24750 = EDGE_LOOP ( 'NONE', ( #10579, #2435, #11944, #11339 ) ) ;
#24751 = CARTESIAN_POINT ( 'NONE',  ( 54.42253022455169997, -6.265509904175804647E-05, 4.373069084971676013 ) ) ;
#24752 = ORIENTED_EDGE ( 'NONE', *, *, #14924, .T. ) ;
#24753 = CARTESIAN_POINT ( 'NONE',  ( 22.07280086217094350, 8.086143481909239483, 2.049999999999922551 ) ) ;
#24754 = ORIENTED_EDGE ( 'NONE', *, *, #11976, .T. ) ;
#24755 = CARTESIAN_POINT ( 'NONE',  ( 51.70000000000001705, -4.179189514726506793, -1.000000000000000000 ) ) ;
#24756 = CARTESIAN_POINT ( 'NONE',  ( 53.82754651211526919, 4.897847608402549291, -2.050000000000188560 ) ) ;
#24757 = DIRECTION ( 'NONE',  ( 1.000000000000000000, 0.000000000000000000, 0.000000000000000000 ) ) ;
#24758 = DIRECTION ( 'NONE',  ( -1.000000000000000000, -0.000000000000000000, -0.000000000000000000 ) ) ;
#24759 = CARTESIAN_POINT ( 'NONE',  ( 57.01173390802158991, -0.7326096616897963543, 2.432492958759772783 ) ) ;
#24761 = CARTESIAN_POINT ( 'NONE',  ( 54.50000000000002132, 1.734723475976807094E-15, 0.000000000000000000 ) ) ;
#24760 = DIRECTION ( 'NONE',  ( 0.000000000000000000, -0.000000000000000000, 1.000000000000000000 ) ) ;
#24762 = ADVANCED_FACE ( 'NONE', ( #20759 ), #277, .T. ) ;
#24763 = CARTESIAN_POINT ( 'NONE',  ( 50.37722501620131510, -1.384253668070385856, -3.859284659399054185 ) ) ;
#24764 = EDGE_CURVE ( 'NONE', #27693, #30654, #19046, .T. ) ;
#24765 = CIRCLE ( 'NONE', #11112, 3.075000000000000622 ) ;
#24766 = DIRECTION ( 'NONE',  ( 1.000000000000000000, 0.000000000000000000, 0.000000000000000000 ) ) ;
#24767 = CARTESIAN_POINT ( 'NONE',  ( 48.42277498379876022, -1.384253668070385856, 3.859284659399054185 ) ) ;
#24768 = ADVANCED_FACE ( 'NONE', ( #1111 ), #8385, .T. ) ;
#24769 = ORIENTED_EDGE ( 'NONE', *, *, #26592, .F. ) ;
#24770 = CARTESIAN_POINT ( 'NONE',  ( -54.48833221701376317, 1.517896399908648108, 3.311598511235000153 ) ) ;
#24771 = AXIS2_PLACEMENT_3D ( 'NONE', #17975, #29994, #20521 ) ;
#24772 = ORIENTED_EDGE ( 'NONE', *, *, #9703, .F. ) ;
#24773 = ORIENTED_EDGE ( 'NONE', *, *, #27077, .F. ) ;
#24774 = CARTESIAN_POINT ( 'NONE',  ( -62.08896444478691024, -2.506042826205294283, -0.3088273841889361271 ) ) ;
#24775 = CARTESIAN_POINT ( 'NONE',  ( -57.04792740578359656, -2.256877952708263635, 2.542931754211924300 ) ) ;
#24777 = CARTESIAN_POINT ( 'NONE',  ( -60.59999999999997300, -2.458552378503722657, 0.9390651652154902163 ) ) ;
#24776 = CYLINDRICAL_SURFACE ( 'NONE', #11009, 1.000000000000000000 ) ;
#24778 = ORIENTED_EDGE ( 'NONE', *, *, #27819, .F. ) ;
#24779 = ORIENTED_EDGE ( 'NONE', *, *, #21039, .F. ) ;
#24780 = CARTESIAN_POINT ( 'NONE',  ( 54.10834201130843013, 6.369203044738526387, -2.033313965204277540 ) ) ;
#24781 = ORIENTED_EDGE ( 'NONE', *, *, #10298, .T. ) ;
#24782 = CARTESIAN_POINT ( 'NONE',  ( 51.49777277048503521, 1.059151787769027298, -1.232523824083105346 ) ) ;
#24783 =( BOUNDED_CURVE ( )  B_SPLINE_CURVE ( 3, ( #3872, #10839, #11472, #11636 ),
 .UNSPECIFIED., .F., .T. ) 
 B_SPLINE_CURVE_WITH_KNOTS ( ( 4, 4 ),
 ( 1.079950260862541311, 1.195659917899331459 ),
 .UNSPECIFIED. ) 
 CURVE ( )  GEOMETRIC_REPRESENTATION_ITEM ( )  RATIONAL_B_SPLINE_CURVE ( ( 1.000000000000000000, 0.9988845841160336469, 0.9988845841160336469, 1.000000000000000000 ) ) 
 REPRESENTATION_ITEM ( '' )  );
#24784 = AXIS2_PLACEMENT_3D ( 'NONE', #5785, #22584, #24931 ) ;
#24785 = VERTEX_POINT ( 'NONE', #1254 ) ;
#24786 = CARTESIAN_POINT ( 'NONE',  ( 33.98208436309533198, 8.188484713946708737, -2.050000000000247624 ) ) ;
#24787 = B_SPLINE_CURVE_WITH_KNOTS ( 'NONE', 3,
 ( #22534, #15092, #2604, #12703 ),
 .UNSPECIFIED., .F., .F.,
 ( 4, 4 ),
 ( 0.000000000000000000, 0.0003111614939242397359 ),
 .UNSPECIFIED. ) ;
#24788 = CARTESIAN_POINT ( 'NONE',  ( 50.25000000000002132, 5.263408118306026973E-13, 0.8749999999999990008 ) ) ;
#24789 = CARTESIAN_POINT ( 'NONE',  ( -45.15971931043468146, 5.755839955992559655E-16, -4.700000000000000178 ) ) ;
#24790 = DIRECTION ( 'NONE',  ( -1.000000000000000000, -1.047444401652940007E-14, -0.000000000000000000 ) ) ;
#24791 = CARTESIAN_POINT ( 'NONE',  ( -57.45655989232412963, -3.925981830489445379, -2.181683956345066863E-13 ) ) ;
#24792 = CARTESIAN_POINT ( 'NONE',  ( 53.31680359303814498, 8.198234760421843959, -2.050000000000185452 ) ) ;
#24793 = CARTESIAN_POINT ( 'NONE',  ( 47.88156667651360010, -3.908336253171002639, -1.238913932502745618 ) ) ;
#24794 = AXIS2_PLACEMENT_3D ( 'NONE', #23981, #14467, #1796 ) ;
#24795 = CARTESIAN_POINT ( 'NONE',  ( 47.10000000000002274, 6.982261990806648555E-14, -1.632474749424821370E-13 ) ) ;
#24796 = CARTESIAN_POINT ( 'NONE',  ( 50.25000000000002842, -0.4999999999994738653, -1.863080903343643069 ) ) ;
#24797 = LINE ( 'NONE', #27177, #26712 ) ;
#24798 =( NAMED_UNIT ( * ) SI_UNIT ( $, .STERADIAN. ) SOLID_ANGLE_UNIT ( ) );
#24799 = EDGE_CURVE ( 'NONE', #21818, #1995, #16976, .T. ) ;
#24800 = CARTESIAN_POINT ( 'NONE',  ( 58.75000000000003553, -1.996089927834303168, -0.1249999999999982098 ) ) ;
#24801 = CARTESIAN_POINT ( 'NONE',  ( -41.12388279035661753, -5.147405183146891439, 6.303753281455314391E-16 ) ) ;
#24802 = VERTEX_POINT ( 'NONE', #11079 ) ;
#24803 = CARTESIAN_POINT ( 'NONE',  ( 53.94314916079858335, 6.379172879799750007, -1.774223561664970861 ) ) ;
#24804 = CARTESIAN_POINT ( 'NONE',  ( -36.80043232705833844, -3.597789892641473752, -4.037455662930106826 ) ) ;
#24805 = CARTESIAN_POINT ( 'NONE',  ( 54.44724579918531049, 6.358489010972262712, -1.963089969304977700 ) ) ;
#24806 = ORIENTED_EDGE ( 'NONE', *, *, #13244, .T. ) ;
#24807 = CYLINDRICAL_SURFACE ( 'NONE', #20430, 3.499999999999999556 ) ;
#24808 = EDGE_LOOP ( 'NONE', ( #6437, #13562, #5087, #29603, #10353, #17161 ) ) ;
#24809 = CARTESIAN_POINT ( 'NONE',  ( 53.94136487687685388, 6.599443998687462454, 1.761196874214440378 ) ) ;
#24811 = FACE_OUTER_BOUND ( 'NONE', #15781, .T. ) ;
#24810 = CARTESIAN_POINT ( 'NONE',  ( 68.00000000000002842, 1.401298464324817071E-42, -7.122621931239993559E-13 ) ) ;
#24812 = VERTEX_POINT ( 'NONE', #18230 ) ;
#24813 = DIRECTION ( 'NONE',  ( -1.000000000000000000, -0.000000000000000000, -0.000000000000000000 ) ) ;
#24814 = AXIS2_PLACEMENT_3D ( 'NONE', #1715, #28493, #25047 ) ;
#24815 = EDGE_CURVE ( 'NONE', #12697, #26529, #10376, .T. ) ;
#24816 = DIRECTION ( 'NONE',  ( 1.000000000000000000, 3.054025858079668409E-16, -2.042474015755241579E-16 ) ) ;
#24817 = VERTEX_POINT ( 'NONE', #18371 ) ;
#24819 = CARTESIAN_POINT ( 'NONE',  ( -59.69577712845196515, 2.424301977118770157, -1.236100533437267890 ) ) ;
#24818 = CARTESIAN_POINT ( 'NONE',  ( 52.23459832779079903, 3.957147914211791573, 2.045484236922850307 ) ) ;
#24820 = VERTEX_POINT ( 'NONE', #10762 ) ;
#24821 = EDGE_LOOP ( 'NONE', ( #21573, #2236, #17446, #436 ) ) ;
#24822 = CARTESIAN_POINT ( 'NONE',  ( -58.37499999999997158, 2.489203624310591056, -2.804704140674917578 ) ) ;
#24823 = DIRECTION ( 'NONE',  ( 0.000000000000000000, -0.9996898646859344595, -0.02490330187381124827 ) ) ;
#24824 = DIRECTION ( 'NONE',  ( -1.000000000000000000, -3.053848253006669023E-16, 2.042510438544995415E-16 ) ) ;
#24825 = CARTESIAN_POINT ( 'NONE',  ( -61.83175433005612120, -2.659179716902812629, -0.4747749904632609375 ) ) ;
#24826 = CARTESIAN_POINT ( 'NONE',  ( -61.34999999999997300, -2.574153985709302539, -0.5872647410103332133 ) ) ;
#24827 = CARTESIAN_POINT ( 'NONE',  ( -54.88452994616206126, 3.117691453623979481, 1.799999999999816858 ) ) ;
#24828 = CARTESIAN_POINT ( 'NONE',  ( 15.18459684427940104, 1.123735532908289425, 5.289358697221545391 ) ) ;
#24829 = ORIENTED_EDGE ( 'NONE', *, *, #329, .F. ) ;
#24830 =( GEOMETRIC_REPRESENTATION_CONTEXT ( 3 ) GLOBAL_UNCERTAINTY_ASSIGNED_CONTEXT ( ( #26905 ) ) GLOBAL_UNIT_ASSIGNED_CONTEXT ( ( #437, #19768, #14365 ) ) REPRESENTATION_CONTEXT ( 'NONE', 'WORKASPACE' ) );
#24831 = CARTESIAN_POINT ( 'NONE',  ( 15.87128154250955170, 3.738196885377689238, 3.908481927057728456 ) ) ;
#24832 = CARTESIAN_POINT ( 'NONE',  ( -60.60352959746391122, -2.493729372996688731, 0.9514323440252360209 ) ) ;
#24833 = EDGE_CURVE ( 'NONE', #27318, #15189, #8359, .T. ) ;
#24834 = CYLINDRICAL_SURFACE ( 'NONE', #21033, 0.1000000000000000472 ) ;
#24835 = FACE_OUTER_BOUND ( 'NONE', #16674, .T. ) ;
#24836 = CARTESIAN_POINT ( 'NONE',  ( 36.50000000000002132, 0.000000000000000000, -0.7500000000000001110 ) ) ;
#24837 = CARTESIAN_POINT ( 'NONE',  ( 48.48092587705050960, 1.391939743175939048, -3.849999999996903899 ) ) ;
#24838 = ORIENTED_EDGE ( 'NONE', *, *, #28785, .F. ) ;
#24839 = CARTESIAN_POINT ( 'NONE',  ( 58.75000000000000711, 1.760622601996782999, 0.8948927608044728865 ) ) ;
#24840 = ORIENTED_EDGE ( 'NONE', *, *, #19292, .T. ) ;
#24841 = DIRECTION ( 'NONE',  ( -1.163827112947710461E-15, 0.9428090415820623571, 0.3333333333333364235 ) ) ;
#24842 = CARTESIAN_POINT ( 'NONE',  ( 15.30042582489635272, -4.018128186975086891, -3.618665893506916031 ) ) ;
#24843 = ORIENTED_EDGE ( 'NONE', *, *, #23921, .F. ) ;
#24844 = EDGE_LOOP ( 'NONE', ( #11063, #3246, #6124, #31254 ) ) ;
#24845 = LINE ( 'NONE', #10608, #7310 ) ;
#24846 = CIRCLE ( 'NONE', #18818, 4.050000000000000711 ) ;
#24847 = CARTESIAN_POINT ( 'NONE',  ( 47.00000000000002842, -3.637377585518695611, 2.099877210782872261 ) ) ;
#24848 = VERTEX_POINT ( 'NONE', #11382 ) ;
#24850 = CARTESIAN_POINT ( 'NONE',  ( 57.00000000000001421, -0.6999999999999997335, -1.820027472320129514 ) ) ;
#24849 = CARTESIAN_POINT ( 'NONE',  ( -57.25952994616203995, 3.117691453623994580, -1.800000000000189671 ) ) ;
#24851 = DIRECTION ( 'NONE',  ( 0.000000000000000000, -1.000000000000000000, 0.000000000000000000 ) ) ;
#24852 = FACE_OUTER_BOUND ( 'NONE', #25286, .T. ) ;
#24853 = APPLICATION_PROTOCOL_DEFINITION ( 'draft international standard', 'automotive_design', 1998, #26971 ) ;
#24854 = DIRECTION ( 'NONE',  ( 0.000000000000000000, -7.228014483236697541E-16, -1.000000000000000000 ) ) ;
#24855 = EDGE_CURVE ( 'NONE', #12841, #11041, #30356, .T. ) ;
#24856 = ORIENTED_EDGE ( 'NONE', *, *, #5706, .T. ) ;
#24857 = CARTESIAN_POINT ( 'NONE',  ( -56.25952994616206126, -4.643455692769913008E-15, 3.599999999999798916 ) ) ;
#24858 = CARTESIAN_POINT ( 'NONE',  ( 53.81176349924869129, 5.730864617276226980, -1.682988280464833286 ) ) ;
#24859 = CARTESIAN_POINT ( 'NONE',  ( -71.44999999999998863, -1.380331489585512972E-15, 2.906968604901091669E-15 ) ) ;
#24860 = CARTESIAN_POINT ( 'NONE',  ( 15.22842924604220016, 0.7747498452697078042, 5.363501451416292198 ) ) ;
#24861 = FACE_OUTER_BOUND ( 'NONE', #16133, .T. ) ;
#24862 = CIRCLE ( 'NONE', #15268, 159.7997717543496776 ) ;
#24863 = VECTOR ( 'NONE', #16867, 1000.000000000000000 ) ;
#24864 = EDGE_CURVE ( 'NONE', #24250, #22580, #4670, .T. ) ;
#24866 = DIRECTION ( 'NONE',  ( 0.000000000000000000, 0.000000000000000000, 1.000000000000000000 ) ) ;
#24865 = CARTESIAN_POINT ( 'NONE',  ( -62.04999999999998295, -2.687391533643777919, 0.2606275981160458555 ) ) ;
#24867 = EDGE_CURVE ( 'NONE', #10792, #11068, #7838, .T. ) ;
#24868 = EDGE_CURVE ( 'NONE', #20184, #9901, #14933, .T. ) ;
#24869 = DIRECTION ( 'NONE',  ( 1.000000000000000000, 1.047444401652940007E-14, 0.000000000000000000 ) ) ;
#24870 = CARTESIAN_POINT ( 'NONE',  ( 48.40000000000001990, 0.6304760106459513791, -3.950000000000022826 ) ) ;
#24872 = CARTESIAN_POINT ( 'NONE',  ( 57.00872446408695993, -0.7491456045391122753, 2.490007504536590588 ) ) ;
#24871 = FACE_OUTER_BOUND ( 'NONE', #15648, .T. ) ;
#24873 = ORIENTED_EDGE ( 'NONE', *, *, #16478, .T. ) ;
#24874 = CARTESIAN_POINT ( 'NONE',  ( 50.50000002815836098, -0.7900353715960748424, -4.025797886239748991 ) ) ;
#24875 = DIRECTION ( 'NONE',  ( 0.000000000000000000, -0.2008964009354147762, 0.9796124928211140670 ) ) ;
#24877 = FACE_OUTER_BOUND ( 'NONE', #20267, .T. ) ;
#24876 = CARTESIAN_POINT ( 'NONE',  ( 15.61033468494287213, 3.560621078037196519, -4.077054076718805042 ) ) ;
#24878 = CARTESIAN_POINT ( 'NONE',  ( 47.19807692573832725, -4.191416138886288500, 1.624134901684293419 ) ) ;
#24879 = ORIENTED_EDGE ( 'NONE', *, *, #3449, .T. ) ;
#24880 = LINE ( 'NONE', #823, #13452 ) ;
#24881 = LINE ( 'NONE', #5731, #25464 ) ;
#24882 = EDGE_CURVE ( 'NONE', #13995, #27463, #14423, .T. ) ;
#24883 = ORIENTED_EDGE ( 'NONE', *, *, #7742, .F. ) ;
#24884 = CARTESIAN_POINT ( 'NONE',  ( 51.24373197084326392, 0.9939375204961439225, -1.410940055059475062 ) ) ;
#24885 = EDGE_LOOP ( 'NONE', ( #4782, #17007, #17508, #9650 ) ) ;
#24886 = EDGE_LOOP ( 'NONE', ( #18487, #9956, #11538, #7224, #881 ) ) ;
#24887 = DIRECTION ( 'NONE',  ( 0.000000000000000000, 0.000000000000000000, -1.000000000000000000 ) ) ;
#24888 = ORIENTED_EDGE ( 'NONE', *, *, #17242, .F. ) ;
#24889 = SURFACE_STYLE_FILL_AREA ( #20296 ) ;
#24890 = CARTESIAN_POINT ( 'NONE',  ( 27.44806845810027340, 5.340582161072727985, 1.949999999999904476 ) ) ;
#24891 = CARTESIAN_POINT ( 'NONE',  ( -55.64405989232412253, 2.944486372867106461, -1.700000000000184919 ) ) ;
#24892 = VERTEX_POINT ( 'NONE', #26276 ) ;
#24893 = CARTESIAN_POINT ( 'NONE',  ( 69.25000000000000000, 0.6441176470588245717, -1.707553061181374732 ) ) ;
#24894 = DIRECTION ( 'NONE',  ( 1.000000000000000000, 1.047444401652940007E-14, 0.000000000000000000 ) ) ;
#24895 = EDGE_CURVE ( 'NONE', #13972, #21339, #20177, .T. ) ;
#24896 = CARTESIAN_POINT ( 'NONE',  ( 21.97322666366011035, 8.076925076899389211, 2.049999999999926104 ) ) ;
#24897 = ORIENTED_EDGE ( 'NONE', *, *, #21273, .T. ) ;
#24898 = CARTESIAN_POINT ( 'NONE',  ( 51.64281244548096339, 0.8321733326271696374, -1.569379851958313754 ) ) ;
#24899 = CARTESIAN_POINT ( 'NONE',  ( 58.72200959573668655, 0.5298027519224196569, -1.799185603788116872 ) ) ;
#24900 = DIRECTION ( 'NONE',  ( -8.165490522235077225E-15, 0.5454670984324081484, -0.8381322357049213467 ) ) ;
#24901 = CIRCLE ( 'NONE', #22955, 4.100000000000022737 ) ;
#24902 = CARTESIAN_POINT ( 'NONE',  ( 56.95442145253466038, -0.7107037530308675244, -1.762072693003282398 ) ) ;
#24903 = CARTESIAN_POINT ( 'NONE',  ( -56.72499999999997300, 0.9643027244899941008, -4.702139965541347166 ) ) ;
#24904 = EDGE_CURVE ( 'NONE', #18790, #31281, #23403, .T. ) ;
#24906 = LINE ( 'NONE', #29662, #18975 ) ;
#24905 = DIRECTION ( 'NONE',  ( 3.083952846180964840E-15, -1.776356839400251254E-15, 1.000000000000000000 ) ) ;
#24907 = EDGE_CURVE ( 'NONE', #21439, #29156, #18490, .T. ) ;
#24908 = EDGE_CURVE ( 'NONE', #10216, #15120, #27044, .T. ) ;
#24909 = CARTESIAN_POINT ( 'NONE',  ( -61.09488783161975078, -2.409829088982875511, 0.7600985921382209520 ) ) ;
#24910 = DIRECTION ( 'NONE',  ( 0.000000000000000000, 0.02490330187381123092, -0.9996898646859343485 ) ) ;
#24911 = CARTESIAN_POINT ( 'NONE',  ( 58.73371041428899275, 1.381461519774649149, -1.267950628960770487 ) ) ;
#24912 = DIRECTION ( 'NONE',  ( -1.000000000000000000, -3.054025858079668409E-16, 2.042474015755241579E-16 ) ) ;
#24913 = ORIENTED_EDGE ( 'NONE', *, *, #10059, .T. ) ;
#24914 = LINE ( 'NONE', #12727, #30785 ) ;
#24915 = VERTEX_POINT ( 'NONE', #30868 ) ;
#24916 = ORIENTED_EDGE ( 'NONE', *, *, #5579, .T. ) ;
#24917 = DIRECTION ( 'NONE',  ( 1.000000000000000000, 1.047444401652940007E-14, 0.000000000000000000 ) ) ;
#24918 = AXIS2_PLACEMENT_3D ( 'NONE', #7672, #26977, #29054 ) ;
#24919 = CARTESIAN_POINT ( 'NONE',  ( -56.92292740578359656, -3.330682475591783209, -0.6830477631804109384 ) ) ;
#24921 = CARTESIAN_POINT ( 'NONE',  ( -61.39719200130745236, -2.604935742679383548, 0.7098721203061703067 ) ) ;
#24920 = CARTESIAN_POINT ( 'NONE',  ( 50.80000000000001847, 0.2793919678926817807, -0.9601771338026184877 ) ) ;
#24922 = ORIENTED_EDGE ( 'NONE', *, *, #12289, .T. ) ;
#24923 = EDGE_LOOP ( 'NONE', ( #19038, #16927, #23245, #23237 ) ) ;
#24924 = FACE_OUTER_BOUND ( 'NONE', #13387, .T. ) ;
#24925 = ORIENTED_EDGE ( 'NONE', *, *, #10250, .T. ) ;
#24926 = CARTESIAN_POINT ( 'NONE',  ( 57.05000000000001847, -0.8000000000000002665, 2.421260002560650104 ) ) ;
#24927 = ORIENTED_EDGE ( 'NONE', *, *, #3473, .T. ) ;
#24928 = CARTESIAN_POINT ( 'NONE',  ( 30.98482657347591029, 7.184130539199417242, -1.950000000000108091 ) ) ;
#24929 = CARTESIAN_POINT ( 'NONE',  ( 50.59602332238209499, 0.1408342061609074158, -1.212874140286673841 ) ) ;
#24930 = EDGE_CURVE ( 'NONE', #3048, #19414, #29575, .T. ) ;
#24931 = DIRECTION ( 'NONE',  ( 0.000000000000000000, 0.000000000000000000, 1.000000000000000000 ) ) ;
#24932 = ADVANCED_FACE ( 'NONE', ( #24221 ), #16308, .T. ) ;
#24933 = CARTESIAN_POINT ( 'NONE',  ( 15.29384114148407825, -4.822476035523829196, -1.985498375066542476 ) ) ;
#24934 = ADVANCED_FACE ( 'NONE', ( #21237 ), #6330, .T. ) ;
#24935 = CARTESIAN_POINT ( 'NONE',  ( -58.83155989232410832, -1.962990915244706924, -3.400000000000215294 ) ) ;
#24936 = CARTESIAN_POINT ( 'NONE',  ( 47.54395435973425066, -3.873096995916273766, 1.345769568645033942 ) ) ;
#24937 = CARTESIAN_POINT ( 'NONE',  ( -54.44999999999997442, 2.818925648462311528E-15, 9.856100559121352825E-17 ) ) ;
#24938 = CARTESIAN_POINT ( 'NONE',  ( 69.05000000000002558, 4.557543281186736018E-17, -7.232603593413552923E-13 ) ) ;
#24939 = CARTESIAN_POINT ( 'NONE',  ( 58.72202590012995671, -0.4851648829343623293, 1.811143295643880213 ) ) ;
#24940 = AXIS2_PLACEMENT_3D ( 'NONE', #14862, #3004, #2838 ) ;
#24941 = CIRCLE ( 'NONE', #20415, 0.04999999999999994033 ) ;
#24942 =( LENGTH_UNIT ( ) NAMED_UNIT ( * ) SI_UNIT ( .MILLI., .METRE. ) );
#24943 = CARTESIAN_POINT ( 'NONE',  ( -59.28448904087081672, 2.425384292835127464, -1.073600088316289947 ) ) ;
#24944 = CARTESIAN_POINT ( 'NONE',  ( 50.34192419032897448, 8.193354243125561709, -2.050000000000174794 ) ) ;
#24945 = ORIENTED_EDGE ( 'NONE', *, *, #23258, .T. ) ;
#24946 = CARTESIAN_POINT ( 'NONE',  ( -59.29999999999994742, 1.055797642268307301, 3.459130888392116354 ) ) ;
#24947 = CARTESIAN_POINT ( 'NONE',  ( 51.13585994975462512, -0.9262448312163767961, -1.518514878530177192 ) ) ;
#24948 = CARTESIAN_POINT ( 'NONE',  ( 54.22606526463520993, 5.661062737973960424, 2.046523307115193369 ) ) ;
#24949 = ORIENTED_EDGE ( 'NONE', *, *, #11316, .F. ) ;
#24950 = B_SPLINE_CURVE_WITH_KNOTS ( 'NONE', 3,
 ( #17607, #6044, #1263, #647, #10475, #10306, #25189, #24719, #17764, #1122, #29781, #27405, #15365, #10770, #19975 ),
 .UNSPECIFIED., .F., .F.,
 ( 4, 1, 1, 1, 1, 1, 1, 1, 1, 1, 1, 1, 4 ),
 ( 0.03200690811994900270, 0.06212998257909596589, 0.1242599651581919318, 0.2485199303163838636, 0.3727798954745757953, 0.4970398606327676716, 0.6212998257909596589, 0.6834298083700556248, 0.7455597909491513686, 0.8076897735282473345, 0.8387547648177954285, 0.8698197561073433004, 0.8953196949773711832 ),
 .UNSPECIFIED. ) ;
#24951 = CARTESIAN_POINT ( 'NONE',  ( -59.29999999999997584, 2.330309927981285032E-15, 4.253626757584724400E-16 ) ) ;
#24952 =( BOUNDED_CURVE ( )  B_SPLINE_CURVE ( 3, ( #762, #10885, #10427, #940 ),
 .UNSPECIFIED., .F., .F. ) 
 B_SPLINE_CURVE_WITH_KNOTS ( ( 4, 4 ),
 ( 1.362166255977964147, 1.466857099139255105 ),
 .UNSPECIFIED. ) 
 CURVE ( )  GEOMETRIC_REPRESENTATION_ITEM ( )  RATIONAL_B_SPLINE_CURVE ( ( 1.000000000000000000, 0.9990868608118155247, 0.9990868608118155247, 1.000000000000000000 ) ) 
 REPRESENTATION_ITEM ( '' )  );
#24953 = ORIENTED_EDGE ( 'NONE', *, *, #25138, .F. ) ;
#24954 = CARTESIAN_POINT ( 'NONE',  ( 51.79118766240952709, 4.088244304910976012, 1.991034353352840958 ) ) ;
#24955 = CARTESIAN_POINT ( 'NONE',  ( -36.38139716712352367, -5.370189181195086370, 0.6649548426257814171 ) ) ;
#24956 = CARTESIAN_POINT ( 'NONE',  ( 51.60286920921249987, -3.901416201057245292, -1.541017813822733062 ) ) ;
#24957 = ORIENTED_EDGE ( 'NONE', *, *, #23598, .F. ) ;
#24958 = CARTESIAN_POINT ( 'NONE',  ( 60.99000702708185884, -0.5469907030321375929, -1.538545889480080309 ) ) ;
#24959 = CARTESIAN_POINT ( 'NONE',  ( 60.75000000000001421, 0.5000000000006363798, 1.863080903344385808 ) ) ;
#24960 = ORIENTED_EDGE ( 'NONE', *, *, #8715, .T. ) ;
#24962 = CARTESIAN_POINT ( 'NONE',  ( 51.80000048712015115, 3.919471099442191520, -2.045252491637605807 ) ) ;
#24961 = CARTESIAN_POINT ( 'NONE',  ( 52.99773473688004088, 4.225724694811284543, 2.047297911660232117 ) ) ;
#24963 = ORIENTED_EDGE ( 'NONE', *, *, #24517, .F. ) ;
#24964 = ORIENTED_EDGE ( 'NONE', *, *, #26456, .T. ) ;
#24965 = DIRECTION ( 'NONE',  ( 0.000000000000000000, 0.000000000000000000, 1.000000000000000000 ) ) ;
#24966 = CIRCLE ( 'NONE', #9797, 0.05000000000000008604 ) ;
#24967 = EDGE_CURVE ( 'NONE', #15457, #4799, #5039, .T. ) ;
#24968 = CARTESIAN_POINT ( 'NONE',  ( 58.75000000000000000, 1.671477153795420501, -0.8495817349390359929 ) ) ;
#24969 = EDGE_CURVE ( 'NONE', #26664, #26160, #9338, .T. ) ;
#24970 = DIRECTION ( 'NONE',  ( 0.000000000000000000, 1.000000000000000000, 3.491481338843130594E-15 ) ) ;
#24971 = CARTESIAN_POINT ( 'NONE',  ( -59.69999999999996021, -1.369200569148549373, -3.341326691469316490 ) ) ;
#24972 = ADVANCED_FACE ( 'NONE', ( #12180 ), #9665, .T. ) ;
#24973 = DIRECTION ( 'NONE',  ( 1.000000000000000000, 1.047444401652940007E-14, 0.000000000000000000 ) ) ;
#24975 = ORIENTED_EDGE ( 'NONE', *, *, #6013, .F. ) ;
#24974 = AXIS2_PLACEMENT_3D ( 'NONE', #14983, #24650, #28068 ) ;
#24976 = CARTESIAN_POINT ( 'NONE',  ( 15.45522337368514521, 2.900433254920969706, 4.320265374240213951 ) ) ;
#24977 = AXIS2_PLACEMENT_3D ( 'NONE', #19173, #292, #9800 ) ;
#24978 = EDGE_CURVE ( 'NONE', #24250, #2594, #3146, .T. ) ;
#24979 = CARTESIAN_POINT ( 'NONE',  ( 54.50000000000002132, 0.000000000000000000, 0.000000000000000000 ) ) ;
#24980 = CIRCLE ( 'NONE', #1214, 0.04999999999999991257 ) ;
#24981 = CARTESIAN_POINT ( 'NONE',  ( -59.07202994616203995, -4.156921938165296204, -2.528906867826594094E-13 ) ) ;
#24982 = CARTESIAN_POINT ( 'NONE',  ( 58.75000000000004974, -1.872332544500606044, -0.09997921184723379540 ) ) ;
#24983 = CARTESIAN_POINT ( 'NONE',  ( 48.39081772275598325, 1.198378070452247091, -3.921585382223974570 ) ) ;
#24984 = VERTEX_POINT ( 'NONE', #7726 ) ;
#24985 = CARTESIAN_POINT ( 'NONE',  ( -54.56249999999997158, -1.962990915244707146, -3.400000000000200640 ) ) ;
#24986 = ORIENTED_EDGE ( 'NONE', *, *, #7209, .T. ) ;
#24987 = CARTESIAN_POINT ( 'NONE',  ( -67.97846802697301882, -3.201166483080443511E-16, 2.197917219923980763E-15 ) ) ;
#24988 = AXIS2_PLACEMENT_3D ( 'NONE', #14848, #5055, #24369 ) ;
#24990 = DIRECTION ( 'NONE',  ( 0.000000000000000000, -0.2008964009354147484, 0.9796124928211139560 ) ) ;
#24989 = CARTESIAN_POINT ( 'NONE',  ( -54.49979136068852625, -2.172130796128893149, -2.794980562871907548 ) ) ;
#24991 = ORIENTED_EDGE ( 'NONE', *, *, #20299, .F. ) ;
#24992 = ORIENTED_EDGE ( 'NONE', *, *, #27322, .F. ) ;
#24993 = CARTESIAN_POINT ( 'NONE',  ( 51.80000000000001137, 3.850000000000016520, -1.950000000000180256 ) ) ;
#24994 = FACE_OUTER_BOUND ( 'NONE', #18356, .T. ) ;
#24995 = EDGE_LOOP ( 'NONE', ( #4061, #4210, #12884, #20671, #29060, #5584, #16188 ) ) ;
#24997 = CARTESIAN_POINT ( 'NONE',  ( 68.00000000000001421, 1.401298464324817071E-42, -7.122621931239992550E-13 ) ) ;
#24996 = CARTESIAN_POINT ( 'NONE',  ( -58.88452994616202574, 2.093608279459372350E-14, -3.600000000000208811 ) ) ;
#24998 = CARTESIAN_POINT ( 'NONE',  ( 50.36640492253749102, 1.250162886418204389, 3.874884102585954171 ) ) ;
#24999 = AXIS2_PLACEMENT_3D ( 'NONE', #31119, #23855, #9452 ) ;
#25000 = AXIS2_PLACEMENT_3D ( 'NONE', #1016, #23015, #25526 ) ;
#25001 = CARTESIAN_POINT ( 'NONE',  ( 68.05000000000002558, 1.401298464324817071E-42, -7.127859153248258291E-13 ) ) ;
#25002 = SHAPE_DEFINITION_REPRESENTATION ( #26044, #18201 ) ;
#25003 = EDGE_CURVE ( 'NONE', #3817, #5818, #5672, .T. ) ;
#25004 = CARTESIAN_POINT ( 'NONE',  ( -59.29999999999998295, -2.594510663346734969, 2.255216637833513893 ) ) ;
#25005 = EDGE_CURVE ( 'NONE', #21960, #21439, #2826, .T. ) ;
#25006 = AXIS2_PLACEMENT_3D ( 'NONE', #8966, #6749, #8792 ) ;
#25007 = EDGE_LOOP ( 'NONE', ( #8650, #12391, #28998 ) ) ;
#25008 = B_SPLINE_CURVE_WITH_KNOTS ( 'NONE', 3,
 ( #11925, #21612, #26656, #28725, #9576, #11619, #16696, #24126 ),
 .UNSPECIFIED., .F., .F.,
 ( 4, 2, 2, 4 ),
 ( 0.000000000000000000, 0.0007042195513453415210, 0.001056329327018012227, 0.001408439102690683042 ),
 .UNSPECIFIED. ) ;
#25009 = CARTESIAN_POINT ( 'NONE',  ( -60.75952994616205416, -4.643455692769856999E-15, 3.599999999999783373 ) ) ;
#25010 = AXIS2_PLACEMENT_3D ( 'NONE', #1749, #11419, #30099 ) ;
#25011 = CARTESIAN_POINT ( 'NONE',  ( 48.44664364291948999, -1.310522848978938670, -3.864668279552719632 ) ) ;
#25012 = CARTESIAN_POINT ( 'NONE',  ( 15.17214319754858387, -0.4576450703117617702, 5.200000005133924574 ) ) ;
#25013 = CARTESIAN_POINT ( 'NONE',  ( -54.74999999999997868, -2.944486372867089141, 1.699999999999794342 ) ) ;
#25014 = EDGE_CURVE ( 'NONE', #18443, #15338, #24594, .T. ) ;
#25016 = CARTESIAN_POINT ( 'NONE',  ( 58.65838214097819048, -1.819565423306627627, -0.4528606663874174543 ) ) ;
#25015 = DIRECTION ( 'NONE',  ( 9.297243531610763781E-15, 0.000000000000000000, 1.000000000000000000 ) ) ;
#25017 = CIRCLE ( 'NONE', #23036, 5.147405183146873675 ) ;
#25018 = DIRECTION ( 'NONE',  ( 0.000000000000000000, 0.000000000000000000, 1.000000000000000000 ) ) ;
#25019 = CARTESIAN_POINT ( 'NONE',  ( 52.23456635604563303, 3.957142910676406888, -2.045484142945491524 ) ) ;
#25021 = CARTESIAN_POINT ( 'NONE',  ( -59.67875522479140926, 2.062422519532147280, 1.724463576965509670 ) ) ;
#25020 = DIRECTION ( 'NONE',  ( 9.408669700213139918E-15, -1.000000000000000000, 0.000000000000000000 ) ) ;
#25022 = ORIENTED_EDGE ( 'NONE', *, *, #12321, .F. ) ;
#25023 = DIRECTION ( 'NONE',  ( 1.000000000000000000, 1.047444401652940007E-14, 0.000000000000000000 ) ) ;
#25024 = AXIS2_PLACEMENT_3D ( 'NONE', #12846, #19704, #22528 ) ;
#25025 = CARTESIAN_POINT ( 'NONE',  ( -36.92405921417682890, 3.062358472872086956, -4.459001320275544522 ) ) ;
#25027 = FACE_OUTER_BOUND ( 'NONE', #924, .T. ) ;
#25026 = CARTESIAN_POINT ( 'NONE',  ( 15.22780280894146543, 3.779372851356984864, -3.883777284340693026 ) ) ;
#25028 = CARTESIAN_POINT ( 'NONE',  ( -60.49999999999995737, 1.963826825011730345E-15, 6.704595576490977020E-16 ) ) ;
#25029 = ORIENTED_EDGE ( 'NONE', *, *, #30716, .F. ) ;
#25030 = CARTESIAN_POINT ( 'NONE',  ( 54.13139471328951657, 5.522381836601891081, 2.049999999999811084 ) ) ;
#25031 = CARTESIAN_POINT ( 'NONE',  ( 51.79999999999820659, 1.279603193924745863, -4.104441627167203066 ) ) ;
#25032 = VECTOR ( 'NONE', #13681, 1000.000000000000000 ) ;
#25033 = EDGE_LOOP ( 'NONE', ( #15420, #14796, #30732 ) ) ;
#25034 = AXIS2_PLACEMENT_3D ( 'NONE', #4614, #21894, #4930 ) ;
#25035 = CARTESIAN_POINT ( 'NONE',  ( -62.14999999999998437, 1.152747360993128871E-15, 2.207939306294521009E-15 ) ) ;
#25036 = ORIENTED_EDGE ( 'NONE', *, *, #4640, .F. ) ;
#25037 = EDGE_LOOP ( 'NONE', ( #12696, #26912, #27789, #4458 ) ) ;
#25038 = DIRECTION ( 'NONE',  ( -1.000000000000000000, -3.053848253006669023E-16, 2.042510438544995415E-16 ) ) ;
#25039 = DIRECTION ( 'NONE',  ( -1.000000000000000000, 0.000000000000000000, 0.000000000000000000 ) ) ;
#25040 = VERTEX_POINT ( 'NONE', #12631 ) ;
#25041 =( NAMED_UNIT ( * ) PLANE_ANGLE_UNIT ( ) SI_UNIT ( $, .RADIAN. ) );
#25042 = CARTESIAN_POINT ( 'NONE',  ( 51.31572262954149011, 1.002608958138273554, -1.395204572094392637 ) ) ;
#25043 = EDGE_CURVE ( 'NONE', #7544, #19375, #29417, .T. ) ;
#25044 = CARTESIAN_POINT ( 'NONE',  ( -59.75952994616203284, -3.117691453623963938, -1.800000000000223199 ) ) ;
#25045 = ORIENTED_EDGE ( 'NONE', *, *, #515, .F. ) ;
#25046 = CARTESIAN_POINT ( 'NONE',  ( -54.39999999999999147, 1.514093959731539263, 3.183260039818149867 ) ) ;
#25047 = DIRECTION ( 'NONE',  ( 1.047444401652940007E-14, 0.000000000000000000, 1.000000000000000000 ) ) ;
#25048 = ADVANCED_FACE ( 'NONE', ( #294 ), #24061, .T. ) ;
#25049 = CIRCLE ( 'NONE', #3315, 0.09999999999999997780 ) ;
#25050 = AXIS2_PLACEMENT_3D ( 'NONE', #28145, #1866, #23407 ) ;
#25051 = CARTESIAN_POINT ( 'NONE',  ( 22.68548117337035563, 6.704541182151904977, 2.049999999999919886 ) ) ;
#25052 = ORIENTED_EDGE ( 'NONE', *, *, #19873, .T. ) ;
#25053 = VECTOR ( 'NONE', #27560, 1000.000000000000000 ) ;
#25054 = CARTESIAN_POINT ( 'NONE',  ( -58.31249999999995026, -1.962990915244707368, -3.400000000000213518 ) ) ;
#25055 = CARTESIAN_POINT ( 'NONE',  ( 61.25000000000001421, 0.8666666666673038533, 1.374595900215357824 ) ) ;
#25056 = CARTESIAN_POINT ( 'NONE',  ( 60.88043801789655163, 0.5128233974954672370, -1.858165151416652394 ) ) ;
#25057 = DIRECTION ( 'NONE',  ( 1.000000000000000000, -1.219044193948983948E-29, 3.491481338843133355E-15 ) ) ;
#25058 = CIRCLE ( 'NONE', #28093, 1.000000000000000000 ) ;
#25059 = EDGE_CURVE ( 'NONE', #2603, #2931, #19469, .T. ) ;
#25061 = FACE_OUTER_BOUND ( 'NONE', #16298, .T. ) ;
#25060 = CARTESIAN_POINT ( 'NONE',  ( 58.65000000000001990, 6.143261415694495821E-13, 3.111507638930570854E-58 ) ) ;
#25062 = CARTESIAN_POINT ( 'NONE',  ( 50.45717930666027229, -1.210123066480733200, -3.917958458743180827 ) ) ;
#25063 = CARTESIAN_POINT ( 'NONE',  ( -54.49999999999997868, 8.366749974758391359E-15, -1.938977325913827332E-13 ) ) ;
#25064 = CARTESIAN_POINT ( 'NONE',  ( -55.43749999999997868, 0.7533615035078096156, -3.673546848079177529 ) ) ;
#25065 = CARTESIAN_POINT ( 'NONE',  ( 36.50000000000002132, 2.296212748401286986E-16, 1.850000000000000089 ) ) ;
#25066 = CARTESIAN_POINT ( 'NONE',  ( 21.97322666366011745, 8.076925076899298617, 1.949999999999923128 ) ) ;
#25067 = EDGE_LOOP ( 'NONE', ( #31317, #30012, #22482 ) ) ;
#25068 = CARTESIAN_POINT ( 'NONE',  ( 58.64999999999992752, -1.655311165517189931, 1.077297519403137116 ) ) ;
#25069 = EDGE_CURVE ( 'NONE', #20313, #5081, #3560, .T. ) ;
#25070 = AXIS2_PLACEMENT_3D ( 'NONE', #1824, #8780, #30330 ) ;
#25071 = AXIS2_PLACEMENT_3D ( 'NONE', #23439, #28346, #6498 ) ;
#25072 = VERTEX_POINT ( 'NONE', #24674 ) ;
#25073 = AXIS2_PLACEMENT_3D ( 'NONE', #23020, #25530, #20350 ) ;
#25074 = ORIENTED_EDGE ( 'NONE', *, *, #19533, .T. ) ;
#25075 = CARTESIAN_POINT ( 'NONE',  ( 47.10000000000002274, 2.428612866367529932E-14, -1.644487710595116631E-13 ) ) ;
#25076 = CARTESIAN_POINT ( 'NONE',  ( -59.67292740578360366, 2.256877952708268964, -2.542931754211924744 ) ) ;
#25078 = CARTESIAN_POINT ( 'NONE',  ( -61.39798924013852854, -2.604827329856813645, 0.7104159706129550278 ) ) ;
#25077 = CARTESIAN_POINT ( 'NONE',  ( -56.68749999999996447, 1.962990915244749557, -3.400000000000192646 ) ) ;
#25079 = ORIENTED_EDGE ( 'NONE', *, *, #27636, .T. ) ;
#25080 = PRESENTATION_LAYER_ASSIGNMENT (  '', '', ( #7396 ) ) ;
#25081 = ORIENTED_EDGE ( 'NONE', *, *, #6765, .T. ) ;
#25082 = FACE_OUTER_BOUND ( 'NONE', #17407, .T. ) ;
#25083 = VERTEX_POINT ( 'NONE', #12315 ) ;
#25085 = CARTESIAN_POINT ( 'NONE',  ( -62.06710100716625789, -2.624587610216423172, -0.3274367013645053115 ) ) ;
#25084 = CIRCLE ( 'NONE', #5381, 0.2999999999999999334 ) ;
#25086 = EDGE_CURVE ( 'NONE', #6272, #3316, #22315, .T. ) ;
#25087 = ORIENTED_EDGE ( 'NONE', *, *, #6897, .T. ) ;
#25088 = CARTESIAN_POINT ( 'NONE',  ( 23.33428888328930739, 6.022557148079468625, -2.050000000000081979 ) ) ;
#25089 = PRESENTATION_LAYER_ASSIGNMENT (  '', '', ( #7402 ) ) ;
#25090 = EDGE_CURVE ( 'NONE', #15786, #28571, #2988, .T. ) ;
#25091 = DIRECTION ( 'NONE',  ( -1.000000000000000000, 0.000000000000000000, 1.047444401652940007E-14 ) ) ;
#25092 = EDGE_CURVE ( 'NONE', #29220, #22240, #26586, .T. ) ;
#25093 = DIRECTION ( 'NONE',  ( 0.000000000000000000, -1.224646799147353947E-16, 1.000000000000000000 ) ) ;
#25094 = CARTESIAN_POINT ( 'NONE',  ( 15.56401610563846383, -5.370189181195031303, -0.6649548426260208922 ) ) ;
#25095 = AXIS2_PLACEMENT_3D ( 'NONE', #25063, #11274, #3846 ) ;
#25096 = CARTESIAN_POINT ( 'NONE',  ( -58.08155989232410832, -1.962990915244706924, -3.400000000000212630 ) ) ;
#25097 = DIRECTION ( 'NONE',  ( 0.000000000000000000, 0.000000000000000000, 1.000000000000000000 ) ) ;
#25098 = CIRCLE ( 'NONE', #23105, 0.1000000000000000749 ) ;
#25099 = DIRECTION ( 'NONE',  ( -1.282749433769087582E-30, 1.000000000000000000, -1.224646799147353207E-16 ) ) ;
#25100 = AXIS2_PLACEMENT_3D ( 'NONE', #3271, #25115, #1621 ) ;
#25101 = CARTESIAN_POINT ( 'NONE',  ( -59.19810431338756018, -2.425676737179530917, 1.249042049956554656 ) ) ;
#25102 = CIRCLE ( 'NONE', #22623, 2.000000000000000000 ) ;
#25103 = CARTESIAN_POINT ( 'NONE',  ( 50.25000000000004263, -2.008165151418721983, 0.5380862305909606125 ) ) ;
#25105 = CARTESIAN_POINT ( 'NONE',  ( 51.35632695591942820, -4.328087698693943608, 1.560456010858371378 ) ) ;
#25104 = DIRECTION ( 'NONE',  ( 0.000000000000000000, 0.000000000000000000, 1.000000000000000000 ) ) ;
#25106 = AXIS2_PLACEMENT_3D ( 'NONE', #29617, #24869, #5881 ) ;
#25107 = AXIS2_PLACEMENT_3D ( 'NONE', #19758, #7844, #29387 ) ;
#25108 = CARTESIAN_POINT ( 'NONE',  ( 41.48619405471883681, -151.3359592902622239, -2.050000000000163691 ) ) ;
#25109 = CIRCLE ( 'NONE', #20618, 0.04999999999999989175 ) ;
#25110 = CARTESIAN_POINT ( 'NONE',  ( 51.49777277048506363, -1.059151787767940389, 1.232523824083111563 ) ) ;
#25111 = AXIS2_PLACEMENT_3D ( 'NONE', #17949, #13645, #8894 ) ;
#25112 =( BOUNDED_SURFACE ( )  B_SPLINE_SURFACE ( 3, 2, ( 
 ( #27849, #20273, #29903 ),
 ( #23108, #3622, #6011 ),
 ( #20423, #8213, #8363 ),
 ( #27691, #25157, #15809 ),
 ( #15665, #3475, #1399 ),
 ( #10894, #13115, #30365 ),
 ( #11059, #27516, #18352 ),
 ( #5841, #20584, #22804 ),
 ( #25312, #15184, #30218 ),
 ( #13255, #24982, #8525 ) ),
 .UNSPECIFIED., .F., .F., .T. ) 
 B_SPLINE_SURFACE_WITH_KNOTS ( ( 4, 2, 2, 2, 4 ),
 ( 3, 3 ),
 ( 0.0001706658715700577907, 0.0002229276920781165106, 0.0002751895125861752306, 0.0003274513330942339234, 0.0003797131536022926705 ),
 ( 0.000000000000000000, 1.000000000000000000 ),
 .UNSPECIFIED. ) 
 GEOMETRIC_REPRESENTATION_ITEM ( )  RATIONAL_B_SPLINE_SURFACE ( (
 ( 1.000000000000000000, 0.7071067811873469333, 1.000000000000000000),
 ( 1.000000000000000000, 0.7375607040709394324, 1.000000000000000000),
 ( 1.000000000000000000, 0.7730431127427472848, 1.000000000000000000),
 ( 1.000000000000000000, 0.8321012486975403188, 1.000000000000000000),
 ( 1.000000000000000000, 0.8541932017388174092, 1.000000000000000000),
 ( 1.000000000000000000, 0.8545723906033031447, 1.000000000000000000),
 ( 1.000000000000000000, 0.8327032135027588877, 1.000000000000000000),
 ( 1.000000000000000000, 0.7734559727054394207, 1.000000000000000000),
 ( 1.000000000000000000, 0.7377766653992711143, 1.000000000000000000),
 ( 1.000000000000000000, 0.7071067811865520136, 1.000000000000000000) ) ) 
 REPRESENTATION_ITEM ( '' )  SURFACE ( )  );
#25113 = ORIENTED_EDGE ( 'NONE', *, *, #22040, .F. ) ;
#25114 = EDGE_CURVE ( 'NONE', #13929, #14583, #18026, .T. ) ;
#25115 = DIRECTION ( 'NONE',  ( -1.000000000000000000, -0.000000000000000000, 3.491481338843133355E-15 ) ) ;
#25116 = CARTESIAN_POINT ( 'NONE',  ( 54.44772159691260072, 6.353385547808748868, -1.625000000000181188 ) ) ;
#25117 = VERTEX_POINT ( 'NONE', #1539 ) ;
#25118 = CARTESIAN_POINT ( 'NONE',  ( -59.19834903927997516, -2.558621439192811930, -0.9489102922513534821 ) ) ;
#25119 = ORIENTED_EDGE ( 'NONE', *, *, #1905, .F. ) ;
#25120 = ADVANCED_FACE ( 'NONE', ( #15653 ), #5867, .T. ) ;
#25121 = CARTESIAN_POINT ( 'NONE',  ( 51.98855675296393031, -0.7791495708602246273, 1.432971607104406075 ) ) ;
#25122 = DIRECTION ( 'NONE',  ( 0.000000000000000000, -1.000000000000000000, 0.000000000000000000 ) ) ;
#25124 = CARTESIAN_POINT ( 'NONE',  ( 51.69999998495889315, -3.608564799421289493, -1.949774616186548570 ) ) ;
#25123 = CYLINDRICAL_SURFACE ( 'NONE', #26657, 2.649999999999999911 ) ;
#25125 = CIRCLE ( 'NONE', #9971, 4.284222560975607053 ) ;
#25126 = VERTEX_POINT ( 'NONE', #25446 ) ;
#25127 = CARTESIAN_POINT ( 'NONE',  ( 61.22059884411349628, -0.7794434480077455651, -1.429589005548589142 ) ) ;
#25128 = AXIS2_PLACEMENT_3D ( 'NONE', #6915, #4368, #14017 ) ;
#25129 = CARTESIAN_POINT ( 'NONE',  ( -60.48535533905928219, 0.8667965836981847971, -4.226679811941398413 ) ) ;
#25130 = AXIS2_PLACEMENT_3D ( 'NONE', #27737, #3811, #6347 ) ;
#25131 = ORIENTED_EDGE ( 'NONE', *, *, #22571, .F. ) ;
#25133 = DIRECTION ( 'NONE',  ( 1.000000000000000000, 2.586136946169074517E-16, -0.000000000000000000 ) ) ;
#25132 = DIRECTION ( 'NONE',  ( -1.054009200593503061E-14, 0.000000000000000000, -1.000000000000000000 ) ) ;
#25134 = FACE_OUTER_BOUND ( 'NONE', #26824, .T. ) ;
#25135 = ORIENTED_EDGE ( 'NONE', *, *, #16330, .T. ) ;
#25136 = DIRECTION ( 'NONE',  ( 3.489354422748178582E-15, -1.218509414717996338E-16, 1.000000000000000000 ) ) ;
#25137 = DIRECTION ( 'NONE',  ( 0.000000000000000000, 0.000000000000000000, 1.000000000000000000 ) ) ;
#25138 = EDGE_CURVE ( 'NONE', #11503, #18794, #11920, .T. ) ;
#25139 = DIRECTION ( 'NONE',  ( -1.000000000000000000, 0.000000000000000000, 1.047444401652940007E-14 ) ) ;
#25140 = CLOSED_SHELL ( 'NONE', ( #1556, #1055, #9161, #22597, #14720, #22618, #9748, #11125, #11113, #19949, #12388, #2451, #14939, #3259, #19236, #1009, #9141, #22789, #8612, #2019, #21072, #1184, #13953, #30247, #31309, #13373, #14590, #9982, #3483, #7597, #13253, #27402, #24577, #4000, #23102, #20147, #18701, #4233, #24455, #23730, #4005, #15054, #27037, #26098, #17979, #1661, #3071, #564, #15336, #25914, #8996, #1167, #13297, #1628, #30538, #3042, #8607, #15400, #27846, #24408, #4966, #30311, #16933, #19220, #14640, #19359, #4557, #12037 ) ) ;
#25141 = AXIS2_PLACEMENT_3D ( 'NONE', #20090, #27828, #6136 ) ;
#25142 = CARTESIAN_POINT ( 'NONE',  ( -54.49999999999999289, -1.600000000000004530, 3.363870538531237298 ) ) ;
#25143 = CARTESIAN_POINT ( 'NONE',  ( -73.89999999999997726, -0.2499224661714860851, -0.006225825468448203774 ) ) ;
#25144 = AXIS2_PLACEMENT_3D ( 'NONE', #20770, #23295, #1578 ) ;
#25145 = AXIS2_PLACEMENT_3D ( 'NONE', #14553, #18845, #31177 ) ;
#25146 = CARTESIAN_POINT ( 'NONE',  ( 52.06628335902946247, -0.5434431642975651178, 1.718465885608441379 ) ) ;
#25147 = VERTEX_POINT ( 'NONE', #27678 ) ;
#25148 = CARTESIAN_POINT ( 'NONE',  ( -44.59999999999997300, -6.102218906431391608E-14, -1.870876429524648473E-13 ) ) ;
#25149 = AXIS2_PLACEMENT_3D ( 'NONE', #11822, #4068, #23866 ) ;
#25150 = AXIS2_PLACEMENT_3D ( 'NONE', #7117, #16625, #11702 ) ;
#25151 = PLANE ( 'NONE',  #29616 ) ;
#25152 =( BOUNDED_CURVE ( )  B_SPLINE_CURVE ( 2, ( #1227, #22645, #17876, #30041, #8522, #18202, #27844, #15806, #25454, #10431, #3759, #23101, #20112, #27368, #5678, #15330, #3303, #12951, #28312, #9158, #16280, #30992, #2022, #6942, #13869, #8815, #23563, #1865, #30842, #16605, #18663, #6768, #18821, #25609, #1689, #16428, #23880, #21042, #11533, #18503, #6619, #21211, #25926, #28624, #30679, #28465, #11205, #4229, #14046, #26085, #4396, #30361, #23729, #11055, #20733, #8992, #11685, #28144, #21364, #6468, #8666, #26249, #9311, #18976, #20879, #4556, #14205, #18347, #27984, #6298, #15949, #3929, #30505, #13572, #23257, #1543, #16125, #25774, #4081, #13722, #23406 ),
 .UNSPECIFIED., .F., .T. ) 
 B_SPLINE_CURVE_WITH_KNOTS ( ( 3, 2, 2, 2, 2, 2, 2, 2, 2, 2, 2, 2, 2, 2, 2, 2, 2, 2, 2, 2, 2, 2, 2, 2, 2, 2, 2, 2, 2, 2, 2, 2, 2, 2, 2, 2, 2, 2, 2, 2, 3 ),
 ( 0.02979895253302125568, 0.03703703703703703498, 0.05555555555555555247, 0.07407407407407406996, 0.09259259259259258745, 0.1111111111111111049, 0.1296296296296295947, 0.1481481481481481399, 0.1666666666666666574, 0.1851851851851851749, 0.2037037037037036924, 0.2222222222222222099, 0.2407407407407407274, 0.2592592592592592449, 0.2777777777777777901, 0.2962962962962962798, 0.3148148148148147696, 0.3333333333333332593, 0.3518518518518518601, 0.3703703703703703498, 0.3888888888888889506, 0.4074074074074073293, 0.4259259259259259300, 0.4444444444444445308, 0.4629629629629629095, 0.4814814814814813992, 0.5000000000000001110, 0.5185185185185184897, 0.5370370370370370905, 0.5555555555555555802, 0.5740740740740740700, 0.5925925925925925597, 0.6111111111111111605, 0.6296296296296296502, 0.6481481481481481399, 0.6666666666666666297, 0.6851851851851852304, 0.7037037037037037202, 0.7222222222222222099, 0.7407407407407405886, 0.7410924888692722590 ),
 .UNSPECIFIED. ) 
 CURVE ( )  GEOMETRIC_REPRESENTATION_ITEM ( )  RATIONAL_B_SPLINE_CURVE ( ( 0.9362045903222155907, 0.9476351497648202171, 1.000000000000000000, 0.8660254037844387076, 1.000000000000000000, 0.8660254037844387076, 1.000000000000000000, 0.8660254037844387076, 1.000000000000000000, 0.8660254037844387076, 1.000000000000000000, 0.8660254037844387076, 1.000000000000000000, 0.8660254037844387076, 1.000000000000000000, 0.8660254037844387076, 1.000000000000000000, 0.8660254037844387076, 1.000000000000000000, 0.8660254037844387076, 1.000000000000000000, 0.8660254037844387076, 1.000000000000000000, 0.8660254037844387076, 1.000000000000000000, 0.8660254037844387076, 1.000000000000000000, 0.8660254037844387076, 1.000000000000000000, 0.8660254037844387076, 1.000000000000000000, 0.8660254037844387076, 1.000000000000000000, 0.8660254037844387076, 1.000000000000000000, 0.8660254037844387076, 1.000000000000000000, 0.8660254037844387076, 1.000000000000000000, 0.8660254037844387076, 1.000000000000000000, 0.8660254037844387076, 1.000000000000000000, 0.8660254037844387076, 1.000000000000000000, 0.8660254037844387076, 1.000000000000000000, 0.8660254037844387076, 1.000000000000000000, 0.8660254037844387076, 1.000000000000000000, 0.8660254037844387076, 1.000000000000000000, 0.8660254037844387076, 1.000000000000000000, 0.8660254037844387076, 1.000000000000000000, 0.8660254037844387076, 1.000000000000000000, 0.8660254037844387076, 1.000000000000000000, 0.8660254037844387076, 1.000000000000000000, 0.8660254037844387076, 1.000000000000000000, 0.8660254037844387076, 1.000000000000000000, 0.8660254037844387076, 1.000000000000000000, 0.8660254037844387076, 1.000000000000000000, 0.8660254037844387076, 1.000000000000000000, 0.8660254037844387076, 1.000000000000000000, 0.8660254037844387076, 1.000000000000000000, 0.8660254037844387076, 1.000000000000000000, 0.9974552330715619197, 0.9950071387796235456 ) ) 
 REPRESENTATION_ITEM ( '' )  );
#25153 = VECTOR ( 'NONE', #26605, 1000.000000000000000 ) ;
#25154 = CARTESIAN_POINT ( 'NONE',  ( -44.49999999999997868, 6.542789527549899840E-15, -1.397091617737396343E-15 ) ) ;
#25155 = ADVANCED_FACE ( 'NONE', ( #20262 ), #8515, .F. ) ;
#25156 = CARTESIAN_POINT ( 'NONE',  ( -57.19702994616204705, 4.156921938165313968, -1.775982993694543137E-13 ) ) ;
#25157 = CARTESIAN_POINT ( 'NONE',  ( 58.72427158855739293, -1.874564523101702740, 0.04519892032188633363 ) ) ;
#25158 = CARTESIAN_POINT ( 'NONE',  ( 25.99326321321243327, 5.312800855510418252, 2.049999999999909228 ) ) ;
#25159 = ADVANCED_FACE ( 'NONE', ( #15797 ), #8805, .F. ) ;
#25160 = EDGE_LOOP ( 'NONE', ( #30897, #7546, #8674, #25726, #27939 ) ) ;
#25161 = CIRCLE ( 'NONE', #10009, 4.099999999999999645 ) ;
#25162 = CARTESIAN_POINT ( 'NONE',  ( -54.68749999999998579, -3.399999999999991029, -2.060885718922576431E-13 ) ) ;
#25163 = AXIS2_PLACEMENT_3D ( 'NONE', #6735, #4824, #2296 ) ;
#25164 = ORIENTED_EDGE ( 'NONE', *, *, #26720, .F. ) ;
#25165 = EDGE_CURVE ( 'NONE', #1336, #23034, #17484, .T. ) ;
#25166 = CARTESIAN_POINT ( 'NONE',  ( -59.18122760499140611, 2.520598018727130629, -0.9442920350713964739 ) ) ;
#25168 = LINE ( 'NONE', #1098, #28824 ) ;
#25167 = CARTESIAN_POINT ( 'NONE',  ( 57.05000000000001847, 0.7500000000000000000, -2.421260002560649660 ) ) ;
#25169 = VERTEX_POINT ( 'NONE', #6460 ) ;
#25170 = EDGE_LOOP ( 'NONE', ( #12704, #26499, #5261, #30903 ) ) ;
#25171 = DIRECTION ( 'NONE',  ( 1.000000000000000000, 1.047444401652940007E-14, 0.000000000000000000 ) ) ;
#25172 = CARTESIAN_POINT ( 'NONE',  ( 61.25000000000002132, 6.415596960124259844E-13, 3.111507638930570854E-58 ) ) ;
#25173 = VERTEX_POINT ( 'NONE', #18196 ) ;
#25174 = CARTESIAN_POINT ( 'NONE',  ( -57.69702994616206126, -2.078460969082657872, 3.599999999999786926 ) ) ;
#25175 = CARTESIAN_POINT ( 'NONE',  ( -55.67292740578360366, 1.073804522883522239, 3.225979517392336238 ) ) ;
#25176 = AXIS2_PLACEMENT_3D ( 'NONE', #30360, #28310, #8988 ) ;
#25177 = CARTESIAN_POINT ( 'NONE',  ( -73.89999999999997726, -2.435524336289708093E-15, 4.607889071584891164E-15 ) ) ;
#25178 = AXIS2_PLACEMENT_3D ( 'NONE', #25553, #23679, #31090 ) ;
#25179 = EDGE_CURVE ( 'NONE', #13619, #13291, #1235, .T. ) ;
#25180 = CARTESIAN_POINT ( 'NONE',  ( 53.44675344197725053, 5.128499738955621723, -1.627484327855545532 ) ) ;
#25181 = CIRCLE ( 'NONE', #338, 2.100000000000000089 ) ;
#25182 =( NAMED_UNIT ( * ) SI_UNIT ( $, .STERADIAN. ) SOLID_ANGLE_UNIT ( ) );
#25183 = MANIFOLD_SOLID_BREP ( 'Stock-MAS-683-1', #25140 ) ;
#25184 = EDGE_LOOP ( 'NONE', ( #2318, #15096, #30576, #1494, #14770, #19163 ) ) ;
#25185 = PLANE ( 'NONE',  #27906 ) ;
#25186 = CARTESIAN_POINT ( 'NONE',  ( 51.74555621289471929, 3.825902093565871631, -2.050000000000180123 ) ) ;
#25187 = CARTESIAN_POINT ( 'NONE',  ( 48.30261087823118515, -0.9335627837657933803, -3.994936164801341061 ) ) ;
#25188 = CARTESIAN_POINT ( 'NONE',  ( -54.99999999999997868, 2.944486372867092250, 1.699999999999816103 ) ) ;
#25190 = CARTESIAN_POINT ( 'NONE',  ( -35.85663232820584767, 4.683225679163309785, 2.703237727951257607 ) ) ;
#25189 = CARTESIAN_POINT ( 'NONE',  ( 27.62808879389201522, 5.849836810644521989, -1.425000000000096412 ) ) ;
#25191 = AXIS2_PLACEMENT_3D ( 'NONE', #30555, #13612, #6344 ) ;
#25192 = AXIS2_PLACEMENT_3D ( 'NONE', #16026, #27580, #15570 ) ;
#25193 = CARTESIAN_POINT ( 'NONE',  ( 60.75000000000001421, 1.000000000000636380, -1.996089927833914146 ) ) ;
#25194 = FACE_OUTER_BOUND ( 'NONE', #23456, .T. ) ;
#25196 = CARTESIAN_POINT ( 'NONE',  ( -54.49999999999997868, 3.206366378120874661, -1.671797828319853574 ) ) ;
#25195 = CARTESIAN_POINT ( 'NONE',  ( 58.64999999999999858, 1.793224408422687377, -0.5487562170608069056 ) ) ;
#25197 = EDGE_CURVE ( 'NONE', #18572, #28342, #20501, .T. ) ;
#25198 = VERTEX_POINT ( 'NONE', #23551 ) ;
#25199 = CARTESIAN_POINT ( 'NONE',  ( 50.37798322691364916, -1.327156576403582644, -3.879406274192440218 ) ) ;
#25200 = CARTESIAN_POINT ( 'NONE',  ( -36.40878371307407946, 2.334862116275031596, -4.877703086529530552 ) ) ;
#25202 = CARTESIAN_POINT ( 'NONE',  ( 47.49392074102413375, -3.992076856964202669, -1.294425493481064393 ) ) ;
#25201 = CARTESIAN_POINT ( 'NONE',  ( 58.65000000000004121, -1.872332544500605822, -0.09997921184723339294 ) ) ;
#25203 = CARTESIAN_POINT ( 'NONE',  ( 50.25000000000000000, 1.960427193528716305, -0.3958853607737420899 ) ) ;
#25204 = ORIENTED_EDGE ( 'NONE', *, *, #2865, .F. ) ;
#25205 = CARTESIAN_POINT ( 'NONE',  ( 54.13382992866386445, 5.521407779354434275, 2.049999999999811084 ) ) ;
#25206 = CARTESIAN_POINT ( 'NONE',  ( 46.99999999999168665, -4.135416958146860722, 1.091811499727122658 ) ) ;
#25207 = ORIENTED_EDGE ( 'NONE', *, *, #3944, .T. ) ;
#25208 = CYLINDRICAL_SURFACE ( 'NONE', #9350, 0.1500000000000003830 ) ;
#25209 = ORIENTED_EDGE ( 'NONE', *, *, #27628, .F. ) ;
#25210 = CARTESIAN_POINT ( 'NONE',  ( 15.32766723174653478, 3.997758138077601942, -3.641634024966042826 ) ) ;
#25211 = CARTESIAN_POINT ( 'NONE',  ( 47.20943027200282671, -4.226153977860457545, -1.819915812912896502 ) ) ;
#25212 = ORIENTED_EDGE ( 'NONE', *, *, #28131, .F. ) ;
#25213 = CARTESIAN_POINT ( 'NONE',  ( 48.40000000000001990, -0.6304760106459033064, 3.950000000000022826 ) ) ;
#25214 = EDGE_CURVE ( 'NONE', #1641, #30026, #14347, .T. ) ;
#25215 = CARTESIAN_POINT ( 'NONE',  ( -59.07202994616203995, -4.156921938165296204, -2.246292432604653256E-13 ) ) ;
#25216 = ORIENTED_EDGE ( 'NONE', *, *, #22226, .F. ) ;
#25217 = DIRECTION ( 'NONE',  ( -1.499696682456171775E-15, -0.9030524935654885565, 0.4295302013422961362 ) ) ;
#25218 = EDGE_LOOP ( 'NONE', ( #5781, #18361, #844, #5631, #20573 ) ) ;
#25219 = CARTESIAN_POINT ( 'NONE',  ( 50.80000000000001847, -4.003661535119149129, -1.269131321892095654 ) ) ;
#25220 = ORIENTED_EDGE ( 'NONE', *, *, #19355, .T. ) ;
#25221 =( GEOMETRIC_REPRESENTATION_CONTEXT ( 3 ) GLOBAL_UNCERTAINTY_ASSIGNED_CONTEXT ( ( #24692 ) ) GLOBAL_UNIT_ASSIGNED_CONTEXT ( ( #5866, #15526, #18072 ) ) REPRESENTATION_CONTEXT ( 'NONE', 'WORKASPACE' ) );
#25222 = AXIS2_PLACEMENT_3D ( 'NONE', #30442, #6552, #20356 ) ;
#25223 = CARTESIAN_POINT ( 'NONE',  ( -57.49999999999995737, 2.023778652682507790E-14, -3.400000000000204636 ) ) ;
#25224 = CARTESIAN_POINT ( 'NONE',  ( 61.25000000000001421, 0.8825412585414260658, 1.623100356595665206 ) ) ;
#25225 = FACE_OUTER_BOUND ( 'NONE', #12736, .T. ) ;
#25226 = FACE_BOUND ( 'NONE', #30261, .T. ) ;
#25227 = CYLINDRICAL_SURFACE ( 'NONE', #19608, 4.100000000000022737 ) ;
#25228 = CARTESIAN_POINT ( 'NONE',  ( 50.30000000000001847, -1.391941090707485396, -3.750000000000022649 ) ) ;
#25229 = B_SPLINE_CURVE_WITH_KNOTS ( 'NONE', 3,
 ( #7252, #17374, #14993, #19309, #28944, #137, #16921, #9788, #19456, #17091 ),
 .UNSPECIFIED., .F., .F.,
 ( 4, 2, 2, 2, 4 ),
 ( 0.000000000000000000, 0.0003520942986628443545, 0.0007041885973256887090, 0.001056282895988533118, 0.001408377194651377418 ),
 .UNSPECIFIED. ) ;
#25230 = CARTESIAN_POINT ( 'NONE',  ( 51.31572262954149721, 1.002608958138273554, 1.395204572094392192 ) ) ;
#25231 = CARTESIAN_POINT ( 'NONE',  ( 51.50000000000002132, 1.163569835200988601E-28, -1.798112889504214751E-13 ) ) ;
#25232 = CARTESIAN_POINT ( 'NONE',  ( -35.85663232820584057, -3.056483311920867862, 4.206888370749728878 ) ) ;
#25233 = EDGE_CURVE ( 'NONE', #2157, #24201, #1804, .T. ) ;
#25234 = CARTESIAN_POINT ( 'NONE',  ( -54.45996984137642727, 1.500763111530253990, -3.300586169551324556 ) ) ;
#25235 = DIRECTION ( 'NONE',  ( 0.000000000000000000, 0.2008964009354148039, -0.9796124928211139560 ) ) ;
#25236 = VERTEX_POINT ( 'NONE', #28615 ) ;
#25237 = CARTESIAN_POINT ( 'NONE',  ( 50.41422517315185559, -1.132063507975291650, 3.941224428058361706 ) ) ;
#25238 = CARTESIAN_POINT ( 'NONE',  ( -36.52679053911622020, 0.8934212604923185141, -5.334164326942875789 ) ) ;
#25239 = ORIENTED_EDGE ( 'NONE', *, *, #31034, .F. ) ;
#25240 = TOROIDAL_SURFACE ( 'NONE', #14623, 4.650000000000000355, 0.05000000000000000278 ) ;
#25241 = EDGE_LOOP ( 'NONE', ( #3010, #17932, #30057, #27569 ) ) ;
#25242 = CARTESIAN_POINT ( 'NONE',  ( 58.64999999999999858, 1.782657835994909901, 0.5811678240991515754 ) ) ;
#25243 = CARTESIAN_POINT ( 'NONE',  ( -59.17292740578360366, -3.330682475591783653, -0.6830477631804104943 ) ) ;
#25245 = CARTESIAN_POINT ( 'NONE',  ( 51.70000000000001705, -3.826179070414207573, -1.000000000000000000 ) ) ;
#25244 = CARTESIAN_POINT ( 'NONE',  ( -54.99999999999997868, 2.944486372867092250, 1.699999999999816103 ) ) ;
#25246 = VERTEX_POINT ( 'NONE', #21502 ) ;
#25247 = ORIENTED_EDGE ( 'NONE', *, *, #7884, .T. ) ;
#25248 = DIRECTION ( 'NONE',  ( 0.000000000000000000, -1.000000000000000000, -3.491481338843137694E-15 ) ) ;
#25249 = ORIENTED_EDGE ( 'NONE', *, *, #27783, .T. ) ;
#25250 = DIRECTION ( 'NONE',  ( 0.000000000000000000, 0.000000000000000000, 1.000000000000000000 ) ) ;
#25251 = ADVANCED_FACE ( 'NONE', ( #1682 ), #31139, .F. ) ;
#25252 = ORIENTED_EDGE ( 'NONE', *, *, #7127, .F. ) ;
#25253 = DIRECTION ( 'NONE',  ( 1.000000000000000000, 1.047444401652940007E-14, 0.000000000000000000 ) ) ;
#25254 = DIRECTION ( 'NONE',  ( 0.000000000000000000, 0.000000000000000000, 1.000000000000000000 ) ) ;
#25255 = DIRECTION ( 'NONE',  ( -1.000000000000000000, -3.054027077731387480E-16, 2.042479963029832083E-16 ) ) ;
#25256 = AXIS2_PLACEMENT_3D ( 'NONE', #5855, #20599, #3776 ) ;
#25257 = DIRECTION ( 'NONE',  ( 1.000000000000000000, -0.000000000000000000, -1.047444401652940007E-14 ) ) ;
#25258 = CARTESIAN_POINT ( 'NONE',  ( -58.01905989232410832, 2.023778652682508421E-14, -3.400000000000205969 ) ) ;
#25259 = EDGE_CURVE ( 'NONE', #11630, #6668, #21548, .T. ) ;
#25260 = PLANE ( 'NONE',  #21041 ) ;
#25261 = CARTESIAN_POINT ( 'NONE',  ( 54.40000000000001990, 0.000000000000000000, 0.000000000000000000 ) ) ;
#25262 = FACE_OUTER_BOUND ( 'NONE', #6248, .T. ) ;
#25263 = AXIS2_PLACEMENT_3D ( 'NONE', #21524, #4712, #30695 ) ;
#25264 = CARTESIAN_POINT ( 'NONE',  ( 48.43364830228694018, 1.250438735127648027, 3.874838289045730910 ) ) ;
#25265 = AXIS2_PLACEMENT_3D ( 'NONE', #19051, #14597, #29004 ) ;
#25266 = CARTESIAN_POINT ( 'NONE',  ( 64.99999999999998579, 1.401298464324817071E-42, -3.950000000000681410 ) ) ;
#25268 = CARTESIAN_POINT ( 'NONE',  ( 51.70000000000003126, -4.020776289669855785, 2.234582293948397691 ) ) ;
#25267 = CARTESIAN_POINT ( 'NONE',  ( -59.46010231732345375, 3.229909594785855376, 1.334621550118761490 ) ) ;
#25269 = AXIS2_PLACEMENT_3D ( 'NONE', #10654, #524, #12848 ) ;
#25270 = CYLINDRICAL_SURFACE ( 'NONE', #5860, 2.000000000000000000 ) ;
#25271 = DIRECTION ( 'NONE',  ( 0.000000000000000000, 0.000000000000000000, 1.000000000000000000 ) ) ;
#25272 = EDGE_CURVE ( 'NONE', #11223, #10532, #461, .T. ) ;
#25273 = CARTESIAN_POINT ( 'NONE',  ( 51.43355796162965987, -0.9748468443428969232, 1.443681521171313653 ) ) ;
#25274 = EDGE_CURVE ( 'NONE', #12883, #6647, #5012, .T. ) ;
#25275 = VERTEX_POINT ( 'NONE', #4548 ) ;
#25276 = EDGE_CURVE ( 'NONE', #3572, #20361, #22401, .T. ) ;
#25277 = CARTESIAN_POINT ( 'NONE',  ( 54.40373534908291475, 5.983016908836285452, 1.963089969304594895 ) ) ;
#25278 = VERTEX_POINT ( 'NONE', #20812 ) ;
#25279 = CARTESIAN_POINT ( 'NONE',  ( 50.80000000000002558, -3.937842575352406005, 1.145831896685643558 ) ) ;
#25280 = EDGE_LOOP ( 'NONE', ( #1525, #24916, #3906, #5213, #11823 ) ) ;
#25281 = CARTESIAN_POINT ( 'NONE',  ( 15.87128154250933321, -0.7269167730139459715, -5.359285300587695033 ) ) ;
#25282 = CARTESIAN_POINT ( 'NONE',  ( -36.68866260399369850, -5.321612844166216938, 0.9647713018066813584 ) ) ;
#25284 = CARTESIAN_POINT ( 'NONE',  ( -35.85663232820584057, -1.854603232583471356E-14, -5.200000000000000178 ) ) ;
#25283 = DIRECTION ( 'NONE',  ( 1.000000000000000000, 0.000000000000000000, 4.738179285253040686E-16 ) ) ;
#25285 = ORIENTED_EDGE ( 'NONE', *, *, #9701, .T. ) ;
#25286 = EDGE_LOOP ( 'NONE', ( #21895, #2308, #31048, #27957 ) ) ;
#25287 = CARTESIAN_POINT ( 'NONE',  ( 50.25000000000000000, 1.895722432253085898, -0.6373668173460090847 ) ) ;
#25288 = CARTESIAN_POINT ( 'NONE',  ( 57.02942257420237837, -0.7458803891215903814, -1.782029179052657009 ) ) ;
#25289 = ADVANCED_FACE ( 'NONE', ( #18435 ), #5354, .T. ) ;
#25290 = ORIENTED_EDGE ( 'NONE', *, *, #1798, .F. ) ;
#25292 = FACE_OUTER_BOUND ( 'NONE', #15469, .T. ) ;
#25291 = DIRECTION ( 'NONE',  ( 0.000000000000000000, 0.000000000000000000, 1.000000000000000000 ) ) ;
#25293 = CARTESIAN_POINT ( 'NONE',  ( 69.20000000000001705, 0.5000000000000000000, -1.988246715074081017 ) ) ;
#25294 = ORIENTED_EDGE ( 'NONE', *, *, #25782, .F. ) ;
#25295 = DIRECTION ( 'NONE',  ( 1.000000000000000000, -0.000000000000000000, 0.000000000000000000 ) ) ;
#25296 = CARTESIAN_POINT ( 'NONE',  ( 58.72427158855702345, 1.600821037878942033, -0.9764256747740378550 ) ) ;
#25297 = CIRCLE ( 'NONE', #15185, 0.2500000000000003331 ) ;
#25298 = CARTESIAN_POINT ( 'NONE',  ( -54.49999999999997868, 0.000000000000000000, 0.000000000000000000 ) ) ;
#25299 = DIRECTION ( 'NONE',  ( 0.000000000000000000, 0.000000000000000000, -1.000000000000000000 ) ) ;
#25300 = CARTESIAN_POINT ( 'NONE',  ( -54.57202994616205416, -4.156921938165296204, -2.089175772356712570E-13 ) ) ;
#25301 = ADVANCED_FACE ( 'NONE', ( #13332 ), #1779, .T. ) ;
#25302 = ORIENTED_EDGE ( 'NONE', *, *, #17782, .F. ) ;
#25303 = B_SPLINE_CURVE_WITH_KNOTS ( 'NONE', 3,
 ( #14007, #21176, #9439, #23698, #26369, #11655 ),
 .UNSPECIFIED., .F., .F.,
 ( 4, 2, 4 ),
 ( 0.000000000000000000, 0.0001614717865051788824, 0.0003229435730103577648 ),
 .UNSPECIFIED. ) ;
#25304 = EDGE_CURVE ( 'NONE', #15307, #4089, #23915, .T. ) ;
#25305 =( BOUNDED_CURVE ( )  B_SPLINE_CURVE ( 3, ( #12680, #14897, #12229, #22360 ),
 .UNSPECIFIED., .F., .T. ) 
 B_SPLINE_CURVE_WITH_KNOTS ( ( 4, 4 ),
 ( 5.006444828673937586, 5.249382619234884473 ),
 .UNSPECIFIED. ) 
 CURVE ( )  GEOMETRIC_REPRESENTATION_ITEM ( )  RATIONAL_B_SPLINE_CURVE ( ( 1.000000000000000000, 0.9950878134350367166, 0.9950878134350367166, 1.000000000000000000 ) ) 
 REPRESENTATION_ITEM ( '' )  );
#25306 = CARTESIAN_POINT ( 'NONE',  ( -44.49999999999997868, -1.499999999999999556, 4.029888335921975262 ) ) ;
#25307 =( REPRESENTATION_RELATIONSHIP ('NONE','NONE', #7047, #1561 ) REPRESENTATION_RELATIONSHIP_WITH_TRANSFORMATION ( #25475 )SHAPE_REPRESENTATION_RELATIONSHIP( ) );
#25308 = CARTESIAN_POINT ( 'NONE',  ( -58.54806624327022746, 3.400000000000001688, 0.9110272542656313588 ) ) ;
#25309 = ADVANCED_FACE ( 'NONE', ( #1320 ), #5936, .F. ) ;
#25310 = ADVANCED_FACE ( 'NONE', ( #8294 ), #16998, .T. ) ;
#25311 = CARTESIAN_POINT ( 'NONE',  ( -56.44702994616205416, 4.156921938165313968, -1.759978405944979146E-13 ) ) ;
#25313 = AXIS2_PLACEMENT_3D ( 'NONE', #380, #12705, #3212 ) ;
#25312 = CARTESIAN_POINT ( 'NONE',  ( 58.75000000000004263, -1.963941025092382109, -0.09694516907979738862 ) ) ;
#25314 = CARTESIAN_POINT ( 'NONE',  ( 24.20708092330206185, 5.694650688851918829, 2.049999999999915001 ) ) ;
#25315 = ORIENTED_EDGE ( 'NONE', *, *, #29706, .F. ) ;
#25316 = FACE_OUTER_BOUND ( 'NONE', #11780, .T. ) ;
#25317 = ORIENTED_EDGE ( 'NONE', *, *, #11149, .F. ) ;
#25318 = UNCERTAINTY_MEASURE_WITH_UNIT (LENGTH_MEASURE( 1.000000000000000082E-05 ), #9836, 'distance_accuracy_value', 'NONE');
#25319 = CARTESIAN_POINT ( 'NONE',  ( -44.59999999999996589, 1.400000000000023670, -3.959797974644836405 ) ) ;
#25321 = DIRECTION ( 'NONE',  ( 0.000000000000000000, 0.000000000000000000, 1.000000000000000000 ) ) ;
#25320 = CARTESIAN_POINT ( 'NONE',  ( 48.45124641917420405, 1.383300983803913198, 3.859740869727656953 ) ) ;
#25322 = ORIENTED_EDGE ( 'NONE', *, *, #1726, .F. ) ;
#25323 = ORIENTED_EDGE ( 'NONE', *, *, #24246, .T. ) ;
#25324 = DIRECTION ( 'NONE',  ( 0.000000000000000000, 0.000000000000000000, -1.000000000000000000 ) ) ;
#25325 = DIRECTION ( 'NONE',  ( 3.002035892788116966E-16, -0.9996898646859343485, -0.02490330187381123786 ) ) ;
#25327 = DIRECTION ( 'NONE',  ( 0.000000000000000000, 8.881784197001252323E-16, -1.000000000000000000 ) ) ;
#25326 = CARTESIAN_POINT ( 'NONE',  ( -60.50952994616203284, -3.117691453623963938, -1.800000000000225864 ) ) ;
#25328 = CARTESIAN_POINT ( 'NONE',  ( -59.54792740578360366, 3.330682475591789427, 0.6830477631804111605 ) ) ;
#25329 = DIRECTION ( 'NONE',  ( 0.000000000000000000, -0.9996898646859343485, -0.02490330187381124133 ) ) ;
#25330 = APPLICATION_PROTOCOL_DEFINITION ( 'draft international standard', 'automotive_design', 1998, #27985 ) ;
#25331 = DIRECTION ( 'NONE',  ( 1.000000000000000000, 1.047444401652940007E-14, 0.000000000000000000 ) ) ;
#25332 = FILL_AREA_STYLE_COLOUR ( '', #12573 ) ;
#25333 = MANIFOLD_SOLID_BREP ( 'Stock-MAS-683-1', #18576 ) ;
#25334 = ADVANCED_FACE ( 'NONE', ( #16214 ), #9395, .T. ) ;
#25335 = VERTEX_POINT ( 'NONE', #4165 ) ;
#25336 = ADVANCED_FACE ( 'NONE', ( #29982 ), #19234, .T. ) ;
#25337 = DIRECTION ( 'NONE',  ( -1.000000000000000000, -1.293068473084537258E-16, -0.000000000000000000 ) ) ;
#25338 = EDGE_CURVE ( 'NONE', #20361, #28557, #12095, .T. ) ;
#25339 = CARTESIAN_POINT ( 'NONE',  ( 52.38400031671233137, 8.538946093000230775, -1.943109374214847973 ) ) ;
#25340 = CARTESIAN_POINT ( 'NONE',  ( 51.18880157753719828, 1.010242313721750662, -1.292695951881195571 ) ) ;
#25341 = CARTESIAN_POINT ( 'NONE',  ( 15.39414421509789932, -0.2904410314644361724, 5.200000000384604526 ) ) ;
#25342 = DIRECTION ( 'NONE',  ( 0.000000000000000000, -0.2008964009354147484, 0.9796124928211139560 ) ) ;
#25344 = FACE_OUTER_BOUND ( 'NONE', #21464, .T. ) ;
#25343 = CARTESIAN_POINT ( 'NONE',  ( -44.49999999999999289, 1.499999999999999556, -3.300094695611021312 ) ) ;
#25345 = CARTESIAN_POINT ( 'NONE',  ( 65.05000000000001137, -1.025519176787267142E-28, -6.813625832752373386E-13 ) ) ;
#25346 = CARTESIAN_POINT ( 'NONE',  ( 47.06312566212015724, 8.366466760780054912, -2.050000000000163691 ) ) ;
#25348 = CARTESIAN_POINT ( 'NONE',  ( -62.09999999999997300, -2.720545749060828022, -0.4014110452728629763 ) ) ;
#25347 = CARTESIAN_POINT ( 'NONE',  ( -59.51024032614731851, 3.088598804228899652, 1.421463128792039843 ) ) ;
#25349 = EDGE_LOOP ( 'NONE', ( #5692, #6629 ) ) ;
#25350 = AXIS2_PLACEMENT_3D ( 'NONE', #19138, #28777, #7090 ) ;
#25351 = CARTESIAN_POINT ( 'NONE',  ( 58.65000000000001990, 6.143261415694495821E-13, 3.111507638930570854E-58 ) ) ;
#25352 = CARTESIAN_POINT ( 'NONE',  ( -36.72207054450174013, 2.602043737612699470, -4.741394629686777051 ) ) ;
#25354 = CARTESIAN_POINT ( 'NONE',  ( -44.49999999999997868, 0.7497673985144572839, 0.01867747640536023684 ) ) ;
#25353 = CARTESIAN_POINT ( 'NONE',  ( 58.64999999999999147, 1.834410884276226117, 0.3880228184671297154 ) ) ;
#25355 = DIRECTION ( 'NONE',  ( 1.000000000000000000, 3.054025858079668409E-16, -2.042474015755241579E-16 ) ) ;
#25356 = ORIENTED_EDGE ( 'NONE', *, *, #9268, .F. ) ;
#25357 = CARTESIAN_POINT ( 'NONE',  ( 53.60445531103938777, 4.614871059762980288, 2.049999999999812861 ) ) ;
#25358 = DIRECTION ( 'NONE',  ( 0.000000000000000000, -0.9996898646859343485, -0.02490330187381124133 ) ) ;
#25359 = ORIENTED_EDGE ( 'NONE', *, *, #12856, .F. ) ;
#25361 = B_SPLINE_CURVE_WITH_KNOTS ( 'NONE', 3,
 ( #3997, #20948, #8890, #21427 ),
 .UNSPECIFIED., .F., .F.,
 ( 4, 4 ),
 ( 0.000000000000000000, 1.000000000000000000 ),
 .UNSPECIFIED. ) ;
#25360 = DIRECTION ( 'NONE',  ( 9.188425696205898615E-15, 0.000000000000000000, 1.000000000000000000 ) ) ;
#25362 = ORIENTED_EDGE ( 'NONE', *, *, #17004, .F. ) ;
#25363 = DIRECTION ( 'NONE',  ( 0.000000000000000000, 0.000000000000000000, -1.000000000000000000 ) ) ;
#25364 = DIRECTION ( 'NONE',  ( -1.000000000000000000, -1.018631342913014973E-14, -0.000000000000000000 ) ) ;
#25365 = ORIENTED_EDGE ( 'NONE', *, *, #22250, .T. ) ;
#25366 = CARTESIAN_POINT ( 'NONE',  ( 24.69162372611912204, 5.424666981099267815, 1.949999999999913580 ) ) ;
#25367 = CIRCLE ( 'NONE', #10699, 4.299999999999998046 ) ;
#25368 = CARTESIAN_POINT ( 'NONE',  ( -58.01905989232410832, 2.023778652682508421E-14, -3.400000000000205969 ) ) ;
#25369 = VERTEX_POINT ( 'NONE', #16529 ) ;
#25370 = DIRECTION ( 'NONE',  ( 1.047444401652940007E-14, 0.000000000000000000, 1.000000000000000000 ) ) ;
#25371 = ORIENTED_EDGE ( 'NONE', *, *, #25165, .F. ) ;
#25372 = ORIENTED_EDGE ( 'NONE', *, *, #4359, .T. ) ;
#25373 = ADVANCED_FACE ( 'NONE', ( #29023 ), #26338, .T. ) ;
#25374 = TOROIDAL_SURFACE ( 'NONE', #14253, 2.750000000000000000, 0.1000000000000000056 ) ;
#25375 = CARTESIAN_POINT ( 'NONE',  ( -57.37499999999996447, 2.944486372867106905, -1.700000000000191136 ) ) ;
#25376 = EDGE_CURVE ( 'NONE', #28844, #16661, #22061, .T. ) ;
#25377 = CARTESIAN_POINT ( 'NONE',  ( 58.72202590012963697, 0.4851648829358031767, -1.811143295643827811 ) ) ;
#25378 = CARTESIAN_POINT ( 'NONE',  ( 26.18134456910377850, 5.211034382732834480, -1.425000000000091083 ) ) ;
#25379 = DIRECTION ( 'NONE',  ( 1.000000000000000000, -0.000000000000000000, -0.000000000000000000 ) ) ;
#25380 = B_SPLINE_CURVE_WITH_KNOTS ( 'NONE', 3,
 ( #1576, #7595, #22009, #16794, #26438, #4899, #9972, #17253, #26893, #24516, #9523, #29283, #28968, #12323, #19182, #7276, #17113, #11871, #26759, #2828, #20231, #26285, #19331, #19477, #2685, #21716, #12482, #5060, #29122, #16945, #7440, #29861 ),
 .UNSPECIFIED., .F., .F.,
 ( 4, 2, 2, 2, 2, 2, 2, 2, 2, 2, 2, 2, 2, 2, 2, 4 ),
 ( 1.010318202610065295E-16, 0.0009241660915624322521, 0.001848332183124763457, 0.002772498274687094661, 0.003696664366249425866, 0.004620830457811756636, 0.005544996549374087841, 0.006469162640936418178, 0.006931245686717583780, 0.007393328732498750250, 0.009241660915623431741, 0.01016582700718577509, 0.01108999309874812017, 0.01201415919031047566, 0.01293832528187282768, 0.01478665746499753693 ),
 .UNSPECIFIED. ) ;
#25381 = CARTESIAN_POINT ( 'NONE',  ( 69.04999999999999716, 4.155057991226904698E-16, -3.020710678119369330 ) ) ;
#25383 = DIRECTION ( 'NONE',  ( 3.491481338843133750E-15, 0.000000000000000000, 1.000000000000000000 ) ) ;
#25382 = CARTESIAN_POINT ( 'NONE',  ( 58.65000000000001990, 6.143261415694495821E-13, 3.111507638930570854E-58 ) ) ;
#25384 = FACE_OUTER_BOUND ( 'NONE', #5000, .T. ) ;
#25385 = CYLINDRICAL_SURFACE ( 'NONE', #26118, 4.000000000000000000 ) ;
#25386 = CARTESIAN_POINT ( 'NONE',  ( -57.22499999999997300, 2.964020293532818446E-15, 1.549317489258324336E-18 ) ) ;
#25387 = ADVANCED_FACE ( 'NONE', ( #14140 ), #18758, .T. ) ;
#25388 = CARTESIAN_POINT ( 'NONE',  ( 56.96003682719288008, 0.7597908294545935304, 2.486534234876009553 ) ) ;
#25389 = CARTESIAN_POINT ( 'NONE',  ( 48.50000000000002132, -1.426739617975173013, 3.843750000000023093 ) ) ;
#25390 = ORIENTED_EDGE ( 'NONE', *, *, #10338, .T. ) ;
#25391 = DIRECTION ( 'NONE',  ( 0.000000000000000000, 0.000000000000000000, -1.000000000000000000 ) ) ;
#25392 = DIRECTION ( 'NONE',  ( -1.000000000000000000, 0.000000000000000000, 1.047444401652940007E-14 ) ) ;
#25393 = VERTEX_POINT ( 'NONE', #18908 ) ;
#25394 = DIRECTION ( 'NONE',  ( 0.000000000000000000, 0.000000000000000000, 1.000000000000000000 ) ) ;
#25395 = CARTESIAN_POINT ( 'NONE',  ( 60.99999997330885293, 0.8151934526821700278, -1.407049160682770861 ) ) ;
#25397 = FACE_OUTER_BOUND ( 'NONE', #30953, .T. ) ;
#25396 = CARTESIAN_POINT ( 'NONE',  ( -56.56249999999997158, 3.925981830489463142, -1.866702293926226148E-13 ) ) ;
#25398 = VERTEX_POINT ( 'NONE', #23967 ) ;
#25399 = ORIENTED_EDGE ( 'NONE', *, *, #9839, .T. ) ;
#25400 = CARTESIAN_POINT ( 'NONE',  ( 51.80000000000000426, -4.020776289669849568, -2.234582293948755183 ) ) ;
#25401 = EDGE_LOOP ( 'NONE', ( #10163, #13799, #17631, #6595 ) ) ;
#25402 = EDGE_LOOP ( 'NONE', ( #15017, #21670, #4339, #25131 ) ) ;
#25403 = CARTESIAN_POINT ( 'NONE',  ( 22.72181155690797638, 6.520914527883283185, -2.050000000000079758 ) ) ;
#25404 = CIRCLE ( 'NONE', #15299, 2.000000000000000000 ) ;
#25405 = DIRECTION ( 'NONE',  ( 3.002035892788117459E-16, -0.9996898646859344595, -0.02490330187381124133 ) ) ;
#25406 = CARTESIAN_POINT ( 'NONE',  ( 58.75000000000003553, -1.932246131436417436, 0.4087173687851147208 ) ) ;
#25407 = VERTEX_POINT ( 'NONE', #19068 ) ;
#25408 = ADVANCED_FACE ( 'NONE', ( #1958 ), #14451, .F. ) ;
#25409 = CARTESIAN_POINT ( 'NONE',  ( -58.47099364905386665, -0.2309624077928895125, -3.875409454552786848 ) ) ;
#25410 = ADVANCED_FACE ( 'NONE', ( #6862 ), #31184, .F. ) ;
#25411 = CARTESIAN_POINT ( 'NONE',  ( 15.70940947763170925, 0.8934212604923389422, 5.334164326942875789 ) ) ;
#25412 = CARTESIAN_POINT ( 'NONE',  ( -60.58155989232412253, -1.962990915244731571, 3.399999999999776534 ) ) ;
#25413 = EDGE_CURVE ( 'NONE', #11413, #7802, #2260, .T. ) ;
#25414 = CARTESIAN_POINT ( 'NONE',  ( 47.49584747294277065, -3.900546889229666636, 1.266936454265243039 ) ) ;
#25415 = CARTESIAN_POINT ( 'NONE',  ( 69.20000000000001705, -0.7500000000000000000, -1.988246715074081017 ) ) ;
#25416 = CARTESIAN_POINT ( 'NONE',  ( -57.22499999999997300, 2.964020293532818446E-15, 1.549317489258312010E-18 ) ) ;
#25417 = CARTESIAN_POINT ( 'NONE',  ( 53.81457038983117513, 5.799118250651475570, -1.689328355159275041 ) ) ;
#25419 = DIRECTION ( 'NONE',  ( 0.000000000000000000, -3.469446951953614189E-15, 1.000000000000000000 ) ) ;
#25418 = DIRECTION ( 'NONE',  ( 0.000000000000000000, -1.000000000000000000, 0.000000000000000000 ) ) ;
#25420 = DIRECTION ( 'NONE',  ( -1.000000000000000000, -0.000000000000000000, -0.000000000000000000 ) ) ;
#25421 = DIRECTION ( 'NONE',  ( 1.156482317317871449E-14, 0.000000000000000000, 1.000000000000000000 ) ) ;
#25422 = EDGE_CURVE ( 'NONE', #30944, #9458, #28399, .T. ) ;
#25423 = CARTESIAN_POINT ( 'NONE',  ( -73.90999999999998238, -2.438578184542714499E-15, 4.609931582023435380E-15 ) ) ;
#25424 = AXIS2_PLACEMENT_3D ( 'NONE', #1626, #8749, #23490 ) ;
#25425 = EDGE_LOOP ( 'NONE', ( #27495, #22340, #14776, #2481 ) ) ;
#25426 = CARTESIAN_POINT ( 'NONE',  ( 54.29903447189319365, 6.002870899074444822, -2.050000000000188116 ) ) ;
#25427 = ORIENTED_EDGE ( 'NONE', *, *, #8479, .T. ) ;
#25428 = VERTEX_POINT ( 'NONE', #31076 ) ;
#25429 = CARTESIAN_POINT ( 'NONE',  ( 51.77457724156050034, -3.759243154119239261, 1.865745259404142598 ) ) ;
#25430 = ORIENTED_EDGE ( 'NONE', *, *, #7926, .F. ) ;
#25431 = CARTESIAN_POINT ( 'NONE',  ( 53.71202192472757275, 7.447163568589272309, 1.837855077339518362 ) ) ;
#25432 = CARTESIAN_POINT ( 'NONE',  ( -58.40835481156723574, -0.8699069336946632092, 4.241846523238430144 ) ) ;
#25434 = DIRECTION ( 'NONE',  ( 0.000000000000000000, -0.8660422822663634834, 0.4999707644721521627 ) ) ;
#25433 = CARTESIAN_POINT ( 'NONE',  ( -77.29999999999998295, -3.473832742311974792E-15, 5.302342620690189014E-15 ) ) ;
#25435 = ORIENTED_EDGE ( 'NONE', *, *, #27443, .T. ) ;
#25436 = CARTESIAN_POINT ( 'NONE',  ( 31.86627779902472568, 7.736385160319314558, -2.050000000000110845 ) ) ;
#25437 = CARTESIAN_POINT ( 'NONE',  ( 58.75000000000000711, 1.791164585743217685, -0.8897917884432153812 ) ) ;
#25438 = ORIENTED_EDGE ( 'NONE', *, *, #8258, .T. ) ;
#25440 = LINE ( 'NONE', #22626, #3927 ) ;
#25439 = CARTESIAN_POINT ( 'NONE',  ( -74.39999999999997726, -2.588216748940040213E-15, 4.710014593512140639E-15 ) ) ;
#25441 = CYLINDRICAL_SURFACE ( 'NONE', #8891, 1.000000000000000000 ) ;
#25442 = VERTEX_POINT ( 'NONE', #30931 ) ;
#25443 = CARTESIAN_POINT ( 'NONE',  ( -35.85663232820583346, 3.817150320979498357, 2.203324261493436520 ) ) ;
#25444 = CARTESIAN_POINT ( 'NONE',  ( 58.73379417893117704, 1.582215608939472773, -1.006340787082015131 ) ) ;
#25445 = EDGE_CURVE ( 'NONE', #9698, #30783, #25008, .T. ) ;
#25446 = CARTESIAN_POINT ( 'NONE',  ( 51.80000048712027905, 3.919471135816211316, 2.045252759501752227 ) ) ;
#25447 = CARTESIAN_POINT ( 'NONE',  ( -73.89999999999997726, -2.435524336289708093E-15, 4.607889071584891164E-15 ) ) ;
#25449 = FACE_OUTER_BOUND ( 'NONE', #5599, .T. ) ;
#25448 = AXIS2_PLACEMENT_3D ( 'NONE', #23922, #9681, #26768 ) ;
#25450 = ADVANCED_FACE ( 'NONE', ( #4961 ), #4793, .T. ) ;
#25451 = AXIS2_PLACEMENT_3D ( 'NONE', #1916, #18554, #26138 ) ;
#25452 = ORIENTED_EDGE ( 'NONE', *, *, #29897, .T. ) ;
#25453 = LINE ( 'NONE', #4080, #5883 ) ;
#25454 = CARTESIAN_POINT ( 'NONE',  ( -54.92292740578361077, 1.073804522883522239, 3.225979517392335794 ) ) ;
#25455 = EDGE_CURVE ( 'NONE', #26012, #29967, #11456, .T. ) ;
#25456 = CARTESIAN_POINT ( 'NONE',  ( 51.80693638829369974, -4.271975761602690547, 0.9446694106403946689 ) ) ;
#25457 = CARTESIAN_POINT ( 'NONE',  ( 60.75000000000002842, -0.6499999999993638644, -1.489337100860647967 ) ) ;
#25458 = DIRECTION ( 'NONE',  ( 3.489354422748178582E-15, -1.218509414717996338E-16, 1.000000000000000000 ) ) ;
#25459 = CARTESIAN_POINT ( 'NONE',  ( 22.49281023664668311, 6.945812178203861542, 2.049999999999921663 ) ) ;
#25460 = ORIENTED_EDGE ( 'NONE', *, *, #16689, .T. ) ;
#25461 = DIRECTION ( 'NONE',  ( -3.491481338843133355E-15, 0.000000000000000000, -1.000000000000000000 ) ) ;
#25462 = EDGE_LOOP ( 'NONE', ( #26891, #1675, #10172, #16813 ) ) ;
#25463 = CARTESIAN_POINT ( 'NONE',  ( 50.33710128586455568, -1.426739617975172569, 3.843750000000022649 ) ) ;
#25464 = VECTOR ( 'NONE', #27740, 1000.000000000000000 ) ;
#25466 = FACE_OUTER_BOUND ( 'NONE', #5047, .T. ) ;
#25465 = CARTESIAN_POINT ( 'NONE',  ( 58.74160516400048238, 0.8556415768453904391, -1.668397168088362026 ) ) ;
#25467 = EDGE_CURVE ( 'NONE', #24423, #11687, #30774, .T. ) ;
#25468 = ORIENTED_EDGE ( 'NONE', *, *, #7486, .T. ) ;
#25469 = VERTEX_POINT ( 'NONE', #23667 ) ;
#25470 = DIRECTION ( 'NONE',  ( -1.000000000000000000, 0.000000000000000000, 1.047444401652940007E-14 ) ) ;
#25471 = CARTESIAN_POINT ( 'NONE',  ( -44.49999999999997868, 6.542789527549899840E-15, -1.397091617737396343E-15 ) ) ;
#25472 = DIRECTION ( 'NONE',  ( 1.000000000000000000, 0.000000000000000000, 0.000000000000000000 ) ) ;
#25473 = CARTESIAN_POINT ( 'NONE',  ( -56.23542740578360366, -3.725040285533364859, 1.239922660687674982 ) ) ;
#25474 = CARTESIAN_POINT ( 'NONE',  ( 50.30000000000001847, -1.391941090707485396, 3.750000000000022649 ) ) ;
#25475 = ITEM_DEFINED_TRANSFORMATION ( 'NONE', 'NONE', #8552,  #9018 ) ;
#25476 = EDGE_CURVE ( 'NONE', #24164, #18442, #26540, .T. ) ;
#25477 = CARTESIAN_POINT ( 'NONE',  ( -59.37758717751765403, 2.334345179268707771, 1.271211832739848280 ) ) ;
#25478 = ADVANCED_FACE ( 'NONE', ( #27268 ), #7888, .T. ) ;
#25479 =( BOUNDED_CURVE ( )  B_SPLINE_CURVE ( 2, ( #13389, #18194, #10729, #15650, #20567, #17556, #17869, #12780, #22460 ),
 .UNSPECIFIED., .F., .T. ) 
 B_SPLINE_CURVE_WITH_KNOTS ( ( 3, 2, 2, 2, 3 ),
 ( 0.03397538932574487025, 0.03703703703703703498, 0.05555555555555555247, 0.07407407407407406996, 0.08333333333333334259 ),
 .UNSPECIFIED. ) 
 CURVE ( )  GEOMETRIC_REPRESENTATION_ITEM ( )  RATIONAL_B_SPLINE_CURVE ( ( 0.9630242692063013532, 0.9778501171427680383, 1.000000000000000000, 0.8660254037844387076, 1.000000000000000000, 0.8660254037844387076, 1.000000000000000000, 0.9330127018922191873, 0.9330127018922192983 ) ) 
 REPRESENTATION_ITEM ( '' )  );
#25480 = ADVANCED_FACE ( 'NONE', ( #19990 ), #17779, .T. ) ;
#25481 = EDGE_LOOP ( 'NONE', ( #2739, #27934, #3980, #22954, #4169, #24182, #25372, #4618, #26344, #16577, #19111, #7532 ) ) ;
#25482 = CARTESIAN_POINT ( 'NONE',  ( -60.94702994616203995, 4.156921938165313080, -2.011299877933566609E-13 ) ) ;
#25483 = CARTESIAN_POINT ( 'NONE',  ( 53.94136487687669046, 6.599443998687474000, -2.050000000000187228 ) ) ;
#25484 = DIRECTION ( 'NONE',  ( 1.000000000000000000, 2.586136946169074517E-16, -0.000000000000000000 ) ) ;
#25485 = AXIS2_PLACEMENT_3D ( 'NONE', #9951, #26878, #14543 ) ;
#25486 = CARTESIAN_POINT ( 'NONE',  ( -59.59999999999997300, 2.337126060168390307, -1.249136413240100607 ) ) ;
#25487 = DIRECTION ( 'NONE',  ( 3.491481338843133355E-15, -0.000000000000000000, 1.000000000000000000 ) ) ;
#25489 = CARTESIAN_POINT ( 'NONE',  ( -36.11187263677868486, 0.3981319440505239893, -5.199999999410233720 ) ) ;
#25488 = FACE_OUTER_BOUND ( 'NONE', #29873, .T. ) ;
#25490 = AXIS2_PLACEMENT_3D ( 'NONE', #19324, #21864, #28961 ) ;
#25491 = DIRECTION ( 'NONE',  ( 3.002035892788117459E-16, -0.9996898646859343485, -0.02490330187381123786 ) ) ;
#25493 = DIRECTION ( 'NONE',  ( 0.000000000000000000, -0.9996898646859343485, -0.02490330187381124133 ) ) ;
#25492 = CARTESIAN_POINT ( 'NONE',  ( 15.03925126672132961, 0.9159215771349694668, -4.311190327366004382 ) ) ;
#25494 = ORIENTED_EDGE ( 'NONE', *, *, #18892, .T. ) ;
#25495 = CARTESIAN_POINT ( 'NONE',  ( 52.06628335902944826, 0.5434431642986583544, 1.718465885608440491 ) ) ;
#25496 = CARTESIAN_POINT ( 'NONE',  ( -36.00201293083839715, 2.199885893005534054, -4.939696249117942806 ) ) ;
#25498 = DIRECTION ( 'NONE',  ( 0.000000000000000000, 0.2008964009354147762, -0.9796124928211140670 ) ) ;
#25497 = CARTESIAN_POINT ( 'NONE',  ( 58.74999999999999289, 1.782657835994903461, 0.5811678240991487998 ) ) ;
#25499 = CARTESIAN_POINT ( 'NONE',  ( 15.29954477411491887, -5.377732435184348070, 0.5657657035912492249 ) ) ;
#25500 = AXIS2_PLACEMENT_3D ( 'NONE', #28909, #21658, #14654 ) ;
#25501 = EDGE_CURVE ( 'NONE', #30038, #6036, #9450, .T. ) ;
#25502 = ORIENTED_EDGE ( 'NONE', *, *, #28147, .T. ) ;
#25503 = CARTESIAN_POINT ( 'NONE',  ( 52.98236138753810565, 8.264679131573773319, 2.049999999999815525 ) ) ;
#25504 = PLANE ( 'NONE',  #19929 ) ;
#25505 = B_SPLINE_CURVE_WITH_KNOTS ( 'NONE', 3,
 ( #26275, #11708, #11380, #6321, #9184, #21066, #30708, #23280, #21537, #6487, #16305, #25950, #18687, #19003, #4580, #14229 ),
 .UNSPECIFIED., .F., .F.,
 ( 4, 2, 2, 2, 2, 2, 2, 4 ),
 ( 0.000000000000000000, 0.0004351083927046410721, 0.0008702167854092821443, 0.001740433570818564289, 0.002175541963523204819, 0.002610650356227845349, 0.003045758748932484578, 0.003480867141637123807 ),
 .UNSPECIFIED. ) ;
#25506 = ORIENTED_EDGE ( 'NONE', *, *, #8474, .T. ) ;
#25507 = EDGE_CURVE ( 'NONE', #17544, #8932, #17454, .T. ) ;
#25508 = AXIS2_PLACEMENT_3D ( 'NONE', #5948, #13517, #30607 ) ;
#25509 = CARTESIAN_POINT ( 'NONE',  ( -44.59999999999998721, -1.400000000000006795, 3.959797974644484242 ) ) ;
#25510 = VERTEX_POINT ( 'NONE', #12379 ) ;
#25511 = FACE_OUTER_BOUND ( 'NONE', #24454, .T. ) ;
#25512 = CARTESIAN_POINT ( 'NONE',  ( -54.44999999999997442, -1.549999999999999600, 4.029888335921975262 ) ) ;
#25513 = ORIENTED_EDGE ( 'NONE', *, *, #4106, .F. ) ;
#25514 = PRESENTATION_STYLE_ASSIGNMENT (( #1452 ) ) ;
#25515 = CARTESIAN_POINT ( 'NONE',  ( -54.50952994616204705, -3.117691453623963938, -1.800000000000204770 ) ) ;
#25516 = CARTESIAN_POINT ( 'NONE',  ( -56.76905989232412963, -2.944486372867088697, 1.699999999999787015 ) ) ;
#25517 = EDGE_LOOP ( 'NONE', ( #3088, #23867, #29469, #5464 ) ) ;
#25518 = DIRECTION ( 'NONE',  ( 0.000000000000000000, 0.4295302013422958032, 0.9030524935654886676 ) ) ;
#25519 = EDGE_LOOP ( 'NONE', ( #14982, #13928, #14408, #24925 ) ) ;
#25520 = CARTESIAN_POINT ( 'NONE',  ( -57.56249999999995737, -1.962990915244707368, -3.400000000000210854 ) ) ;
#25521 = CARTESIAN_POINT ( 'NONE',  ( 58.75000000000001421, 0.4991259882264960646, -1.863313159664827134 ) ) ;
#25522 = PLANE ( 'NONE',  #18304 ) ;
#25523 = DIRECTION ( 'NONE',  ( 1.000000000000000000, 0.000000000000000000, 0.000000000000000000 ) ) ;
#25524 = VECTOR ( 'NONE', #7526, 1000.000000000000000 ) ;
#25525 = DIRECTION ( 'NONE',  ( 1.000000000000000000, 3.054025858079668409E-16, -2.042474015755241579E-16 ) ) ;
#25526 = DIRECTION ( 'NONE',  ( 0.000000000000000000, 0.000000000000000000, 1.000000000000000000 ) ) ;
#25527 = B_SPLINE_CURVE_WITH_KNOTS ( 'NONE', 3,
 ( #6841, #30580, #31232, #18417, #23798, #6370, #16034, #18739, #13641, #16506, #11603, #23647, #1941, #8889, #26164, #26322 ),
 .UNSPECIFIED., .F., .F.,
 ( 4, 3, 3, 3, 3, 4 ),
 ( 0.000000000000000000, 2.806063833126217928E-05, 6.345755872418550124E-05, 9.706205683209630718E-05, 0.0001297115041001252684, 0.0001622821609780518274 ),
 .UNSPECIFIED. ) ;
#25528 = CARTESIAN_POINT ( 'NONE',  ( 15.03925126672133139, -5.086913985776151392, 1.171642053949083495 ) ) ;
#25529 = CARTESIAN_POINT ( 'NONE',  ( 50.75360625943719839, 0.3719558471750615269, 1.344678919698701236 ) ) ;
#25530 = DIRECTION ( 'NONE',  ( -2.964772755551650383E-16, 0.9875000000000001554, -0.1576190026614809614 ) ) ;
#25531 = CARTESIAN_POINT ( 'NONE',  ( 57.05000000000001847, 0.8156862745098041323, 2.468735688885368873 ) ) ;
#25532 = CARTESIAN_POINT ( 'NONE',  ( 48.50000000000002132, 1.391941090707534023, -3.750000000000022649 ) ) ;
#25533 = AXIS2_PLACEMENT_3D ( 'NONE', #21709, #14076, #11561 ) ;
#25534 = CARTESIAN_POINT ( 'NONE',  ( 50.40000000000001990, 0.6304760106459518232, -3.950000000000022826 ) ) ;
#25535 = ORIENTED_EDGE ( 'NONE', *, *, #2949, .T. ) ;
#25536 = DIRECTION ( 'NONE',  ( 1.000000000000000000, 3.054025858079668409E-16, -2.042474015755241579E-16 ) ) ;
#25537 = EDGE_CURVE ( 'NONE', #17902, #28408, #24880, .T. ) ;
#25538 = SURFACE_SIDE_STYLE ('',( #23341 ) ) ;
#25539 = EDGE_CURVE ( 'NONE', #1752, #27301, #24596, .T. ) ;
#25540 = ORIENTED_EDGE ( 'NONE', *, *, #30508, .F. ) ;
#25541 = EDGE_CURVE ( 'NONE', #7544, #704, #21303, .T. ) ;
#25542 = CARTESIAN_POINT ( 'NONE',  ( 61.16418558922026705, 0.6863720863842518449, -1.477277441814810688 ) ) ;
#25544 = DIRECTION ( 'NONE',  ( 0.000000000000000000, -0.9996898646859344595, -0.02490330187381124480 ) ) ;
#25543 = CARTESIAN_POINT ( 'NONE',  ( -57.93749999999998579, 1.962990915244722689, 3.399999999999801847 ) ) ;
#25545 = ORIENTED_EDGE ( 'NONE', *, *, #13832, .T. ) ;
#25546 = ORIENTED_EDGE ( 'NONE', *, *, #5958, .T. ) ;
#25547 = AXIS2_PLACEMENT_3D ( 'NONE', #6081, #17808, #15412 ) ;
#25548 = CARTESIAN_POINT ( 'NONE',  ( 51.67599084732030690, -4.149782173365514026, -1.728795876848868485 ) ) ;
#25549 = ORIENTED_EDGE ( 'NONE', *, *, #29957, .F. ) ;
#25550 = CIRCLE ( 'NONE', #13899, 1.899999999999999911 ) ;
#25551 = CARTESIAN_POINT ( 'NONE',  ( 47.10000000000002274, -3.826179070414207573, -1.000000000000000000 ) ) ;
#25552 = ORIENTED_EDGE ( 'NONE', *, *, #25413, .F. ) ;
#25553 = CARTESIAN_POINT ( 'NONE',  ( -62.04999999999998295, -2.720545749060828022, -0.4014110452728629763 ) ) ;
#25554 = DIRECTION ( 'NONE',  ( 0.000000000000000000, -0.9996898646859344595, -0.02490330187381124133 ) ) ;
#25555 = VECTOR ( 'NONE', #25487, 1000.000000000000000 ) ;
#25556 = DIRECTION ( 'NONE',  ( 0.000000000000000000, 0.000000000000000000, 1.000000000000000000 ) ) ;
#25557 = ORIENTED_EDGE ( 'NONE', *, *, #2806, .T. ) ;
#25558 = AXIS2_PLACEMENT_3D ( 'NONE', #6724, #14634, #24148 ) ;
#25559 = EDGE_CURVE ( 'NONE', #1256, #15189, #9933, .T. ) ;
#25560 = CARTESIAN_POINT ( 'NONE',  ( 68.00000000000001421, -1.025519176787267142E-28, -7.122621931239990530E-13 ) ) ;
#25561 = CARTESIAN_POINT ( 'NONE',  ( -54.68749999999998579, -3.399999999999991029, -2.060885718922576431E-13 ) ) ;
#25562 = CARTESIAN_POINT ( 'NONE',  ( 60.75000000000001421, 0.5000000000006363798, -1.718465885608440047 ) ) ;
#25563 = CARTESIAN_POINT ( 'NONE',  ( 47.10000001504278089, -3.608564799421224656, 1.949774616186315424 ) ) ;
#25564 = CYLINDRICAL_SURFACE ( 'NONE', #7944, 3.750000000000000444 ) ;
#25565 = DIRECTION ( 'NONE',  ( 0.000000000000000000, 0.000000000000000000, 1.000000000000000000 ) ) ;
#25566 = CARTESIAN_POINT ( 'NONE',  ( 58.75000000000004263, -2.008165151418633165, 0.5380862305909606125 ) ) ;
#25568 = CARTESIAN_POINT ( 'NONE',  ( 51.67746714285173226, -4.134031523355556459, 2.020495556749221322 ) ) ;
#25567 = FACE_OUTER_BOUND ( 'NONE', #13369, .T. ) ;
#25569 = CIRCLE ( 'NONE', #9898, 0.2999999999999999334 ) ;
#25570 = CARTESIAN_POINT ( 'NONE',  ( 51.80641384975955788, -4.235076411889995285, 1.097987773005780321 ) ) ;
#25571 = CIRCLE ( 'NONE', #18521, 4.099999999999999645 ) ;
#25572 = CARTESIAN_POINT ( 'NONE',  ( 51.31572262954152563, 0.7526089581382734428, -1.996089927833914146 ) ) ;
#25573 = DIRECTION ( 'NONE',  ( -2.614375865348240525E-16, 0.2008964009354147762, -0.9796124928211140670 ) ) ;
#25574 = ORIENTED_EDGE ( 'NONE', *, *, #26278, .F. ) ;
#25575 = CARTESIAN_POINT ( 'NONE',  ( 54.19698791822510486, 6.698472055538887915, -2.050000000000188116 ) ) ;
#25576 = AXIS2_PLACEMENT_3D ( 'NONE', #20015, #22094, #4816 ) ;
#25577 = ORIENTED_EDGE ( 'NONE', *, *, #30999, .F. ) ;
#25578 = EDGE_CURVE ( 'NONE', #10453, #7998, #17510, .T. ) ;
#25579 = AXIS2_PLACEMENT_3D ( 'NONE', #16355, #21133, #31241 ) ;
#25580 = CARTESIAN_POINT ( 'NONE',  ( 51.25597219945275640, -3.873145847240234030, 1.345634385052566051 ) ) ;
#25581 = ORIENTED_EDGE ( 'NONE', *, *, #11843, .T. ) ;
#25582 = CIRCLE ( 'NONE', #22090, 0.1000000000000002554 ) ;
#25583 = CARTESIAN_POINT ( 'NONE',  ( 51.74540690333468262, 3.818766532315405193, 2.049999999999813305 ) ) ;
#25584 = CARTESIAN_POINT ( 'NONE',  ( -59.22085481156723574, 1.184343223768590692, 3.558065644182727638 ) ) ;
#25586 = CARTESIAN_POINT ( 'NONE',  ( -36.21152527658241382, 3.291455042465393444, 4.036171416105503340 ) ) ;
#25585 = CARTESIAN_POINT ( 'NONE',  ( 61.20721104068434215, -0.7580073711285438831, 1.657084523451290536 ) ) ;
#25587 = ORIENTED_EDGE ( 'NONE', *, *, #7687, .T. ) ;
#25588 = VERTEX_POINT ( 'NONE', #29186 ) ;
#25589 = CARTESIAN_POINT ( 'NONE',  ( 25.69839743624499917, 5.334032503031479244, -2.050000000000089084 ) ) ;
#25590 = CYLINDRICAL_SURFACE ( 'NONE', #18599, 3.399999999999999911 ) ;
#25591 = CIRCLE ( 'NONE', #13433, 0.2500000000000000000 ) ;
#25592 = EDGE_LOOP ( 'NONE', ( #14619, #28246 ) ) ;
#25594 = DIRECTION ( 'NONE',  ( 0.000000000000000000, -4.336808689942006692E-15, 1.000000000000000000 ) ) ;
#25593 = DIRECTION ( 'NONE',  ( 1.000000000000000000, 0.000000000000000000, -0.000000000000000000 ) ) ;
#25595 = CARTESIAN_POINT ( 'NONE',  ( -56.26905989232412963, 2.944486372867089585, 1.699999999999814992 ) ) ;
#25596 = ORIENTED_EDGE ( 'NONE', *, *, #5530, .F. ) ;
#25597 = DIRECTION ( 'NONE',  ( 1.000000000000000000, 5.570239943078649173E-15, -9.650165233620068940E-15 ) ) ;
#25598 = CONICAL_SURFACE ( 'NONE', #30630, 1.625000000000000444, 0.04363323129985093030 ) ;
#25599 = CARTESIAN_POINT ( 'NONE',  ( 33.47623932017462778, 1.734723475976807094E-15, 0.000000000000000000 ) ) ;
#25600 = EDGE_CURVE ( 'NONE', #16439, #4172, #6929, .T. ) ;
#25601 = CARTESIAN_POINT ( 'NONE',  ( 57.01079425239058196, 0.7499991164627679563, 1.746008812021272227 ) ) ;
#25602 = CARTESIAN_POINT ( 'NONE',  ( -57.32202994616202574, 2.078460969082674747, -3.600000000000194600 ) ) ;
#25603 = AXIS2_PLACEMENT_3D ( 'NONE', #7360, #21947, #24449 ) ;
#25604 = CIRCLE ( 'NONE', #6905, 2.674999999999998934 ) ;
#25605 = AXIS2_PLACEMENT_3D ( 'NONE', #17903, #27543, #23288 ) ;
#25606 =( BOUNDED_CURVE ( )  B_SPLINE_CURVE ( 2, ( #22505, #27874, #22973, #977, #17910, #5714, #10629, #15218, #12996 ),
 .UNSPECIFIED., .F., .T. ) 
 B_SPLINE_CURVE_WITH_KNOTS ( ( 3, 2, 2, 2, 3 ),
 ( 0.3055555555555555802, 0.3148148148148148251, 0.3333333333333333148, 0.3518518518518518601, 0.3611111111111111605 ),
 .UNSPECIFIED. ) 
 CURVE ( )  GEOMETRIC_REPRESENTATION_ITEM ( )  RATIONAL_B_SPLINE_CURVE ( ( 0.9330127018922194093, 0.9330127018922195203, 1.000000000000000000, 0.8660254037844387076, 1.000000000000000000, 0.8660254037844387076, 1.000000000000000000, 0.9330127018922189652, 0.9330127018922194093 ) ) 
 REPRESENTATION_ITEM ( '' )  );
#25607 = AXIS2_PLACEMENT_3D ( 'NONE', #7482, #22211, #19221 ) ;
#25608 = CARTESIAN_POINT ( 'NONE',  ( -54.49999999999996447, -1.399999999999981037, -3.363870538531691601 ) ) ;
#25609 = CARTESIAN_POINT ( 'NONE',  ( -56.48542740578359656, 2.936324665650199783, 2.606018187048507517 ) ) ;
#25610 = B_SPLINE_CURVE_WITH_KNOTS ( 'NONE', 3,
 ( #7284, #2836, #29428, #24523, #27050, #12330, #5366, #10128, #12490, #29129, #15027, #22177, #14401, #9979, #2548, #29288, #7602, #17258, #2386, #22017, #464, #26598, #308, #12049, #4909, #14572, #26900, #163 ),
 .UNSPECIFIED., .F., .F.,
 ( 4, 2, 2, 2, 2, 2, 2, 2, 2, 2, 2, 2, 2, 4 ),
 ( 0.003059686050519383211, 0.004393787003443079715, 0.005060837479904928618, 0.005727887956366777521, 0.007061988909290467520, 0.007729039385752312086, 0.008396089862214158386, 0.009063140338676002952, 0.009730190815137849253, 0.01106429176806154879, 0.01239839272098524833, 0.01306544319744709463, 0.01339896843567802039, 0.01373249367390894267 ),
 .UNSPECIFIED. ) ;
#25611 = CARTESIAN_POINT ( 'NONE',  ( -56.87486116251334067, -1.737685414808513018, 3.471684241605566879 ) ) ;
#25612 = CIRCLE ( 'NONE', #8445, 4.375000000000000000 ) ;
#25613 = AXIS2_PLACEMENT_3D ( 'NONE', #13327, #27769, #10986 ) ;
#25614 = CARTESIAN_POINT ( 'NONE',  ( 48.40000000000001990, -0.6304760106459033064, -3.950000000000022826 ) ) ;
#25615 = CIRCLE ( 'NONE', #23607, 0.05000000000000017625 ) ;
#25616 = CARTESIAN_POINT ( 'NONE',  ( -36.38139716712170468, -1.027070083876041373, 5.312835761376664578 ) ) ;
#25617 = DIRECTION ( 'NONE',  ( 0.000000000000000000, 0.000000000000000000, 1.000000000000000000 ) ) ;
#25618 = ORIENTED_EDGE ( 'NONE', *, *, #11976, .F. ) ;
#25619 = ADVANCED_FACE ( 'NONE', ( #14766 ), #17162, .T. ) ;
#25620 = LINE ( 'NONE', #3937, #13787 ) ;
#25621 = AXIS2_PLACEMENT_3D ( 'NONE', #7737, #9815, #14718 ) ;
#25622 = ORIENTED_EDGE ( 'NONE', *, *, #12285, .F. ) ;
#25623 = DIRECTION ( 'NONE',  ( 4.275831445896958607E-31, 1.000000000000000000, 1.224646799147353207E-16 ) ) ;
#25625 = CARTESIAN_POINT ( 'NONE',  ( 47.10000000000002274, 2.428612866367529932E-14, -1.644487710595116631E-13 ) ) ;
#25624 = CARTESIAN_POINT ( 'NONE',  ( 48.42176022524417789, 1.183413901109590105, 3.885761703493072261 ) ) ;
#25626 = ORIENTED_EDGE ( 'NONE', *, *, #19592, .T. ) ;
#25627 = ORIENTED_EDGE ( 'NONE', *, *, #21827, .F. ) ;
#25628 = CARTESIAN_POINT ( 'NONE',  ( -44.49999999999997868, 2.818925648462311528E-15, 9.856100559121352825E-17 ) ) ;
#25629 = CIRCLE ( 'NONE', #24056, 0.04999999999999988481 ) ;
#25630 = CARTESIAN_POINT ( 'NONE',  ( -59.19999999999997442, -2.449420067797476452, 1.250136525132531817 ) ) ;
#25631 = AXIS2_PLACEMENT_3D ( 'NONE', #11911, #26933, #21598 ) ;
#25633 = DIRECTION ( 'NONE',  ( -1.293068473084537258E-16, 1.000000000000000000, 0.000000000000000000 ) ) ;
#25632 = DIRECTION ( 'NONE',  ( 1.000000000000000000, 3.054025858079668409E-16, -2.042474015755241579E-16 ) ) ;
#25634 = CIRCLE ( 'NONE', #28680, 0.1000000000000000749 ) ;
#25635 = ORIENTED_EDGE ( 'NONE', *, *, #8835, .T. ) ;
#25636 = CARTESIAN_POINT ( 'NONE',  ( -58.29792740578360366, -1.073804522883517132, -3.225979517392335350 ) ) ;
#25637 = DIRECTION ( 'NONE',  ( 0.000000000000000000, 0.000000000000000000, 1.000000000000000000 ) ) ;
#25638 = APPLICATION_PROTOCOL_DEFINITION ( 'draft international standard', 'automotive_design', 1998, #30215 ) ;
#25639 = EDGE_CURVE ( 'NONE', #25169, #19884, #27627, .T. ) ;
#25640 = CARTESIAN_POINT ( 'NONE',  ( 53.30088642852334146, 4.970682635617305500, -1.612336972319552642 ) ) ;
#25641 = CARTESIAN_POINT ( 'NONE',  ( 69.25000000000000000, -0.7500000000000000000, -1.988246715074081905 ) ) ;
#25642 = AXIS2_PLACEMENT_3D ( 'NONE', #18189, #10723, #27355 ) ;
#25643 = EDGE_LOOP ( 'NONE', ( #16916, #17734, #15434, #13080 ) ) ;
#25644 = AXIS2_PLACEMENT_3D ( 'NONE', #30374, #15960, #3481 ) ;
#25645 = CARTESIAN_POINT ( 'NONE',  ( -60.57202994616203995, -4.156921938165296204, -2.298664652687300067E-13 ) ) ;
#25646 = CIRCLE ( 'NONE', #30691, 1.487500000000000933 ) ;
#25647 = CARTESIAN_POINT ( 'NONE',  ( -36.38139716712352367, 3.953723660658955641, -3.694477770903653369 ) ) ;
#25648 = CARTESIAN_POINT ( 'NONE',  ( -59.28559899066483041, 3.161828374300069466, 1.250136525132556020 ) ) ;
#25649 = CYLINDRICAL_SURFACE ( 'NONE', #29612, 0.2500000000000000000 ) ;
#25650 = B_SPLINE_CURVE_WITH_KNOTS ( 'NONE', 3,
 ( #13536, #18465, #11308, #20840, #20698, #25888, #9114, #18165, #28102, #4045, #16392, #18784, #1814, #6583, #30324, #8630, #30469, #4191, #11490 ),
 .UNSPECIFIED., .F., .F.,
 ( 4, 3, 3, 3, 3, 3, 4 ),
 ( 0.000000000000000000, 2.270809125664990461E-05, 4.499850898804030560E-05, 6.557565265601914873E-05, 7.920624315363274039E-05, 8.325821076725717102E-05, 9.013793637923205450E-05 ),
 .UNSPECIFIED. ) ;
#25651 = EDGE_CURVE ( 'NONE', #5737, #23458, #18035, .T. ) ;
#25652 = CYLINDRICAL_SURFACE ( 'NONE', #26131, 2.800000000000000266 ) ;
#25653 = AXIS2_PLACEMENT_3D ( 'NONE', #29267, #22156, #4715 ) ;
#25655 = LINE ( 'NONE', #28192, #3299 ) ;
#25654 = CARTESIAN_POINT ( 'NONE',  ( -55.15835481156724285, -3.238593381231841928, -2.874284765127023356 ) ) ;
#25656 = VECTOR ( 'NONE', #4424, 1000.000000000000114 ) ;
#25657 = DIRECTION ( 'NONE',  ( 1.057355261547768637E-14, 0.000000000000000000, 1.000000000000000000 ) ) ;
#25659 = DIRECTION ( 'NONE',  ( 0.000000000000000000, 1.000000000000000000, -0.000000000000000000 ) ) ;
#25658 = DIRECTION ( 'NONE',  ( 0.000000000000000000, 0.000000000000000000, -1.000000000000000000 ) ) ;
#25660 = ORIENTED_EDGE ( 'NONE', *, *, #24704, .T. ) ;
#25661 = EDGE_CURVE ( 'NONE', #18852, #23886, #13220, .T. ) ;
#25662 = CARTESIAN_POINT ( 'NONE',  ( -62.06665691342191593, -2.643441408648605329, -0.3316822223133865100 ) ) ;
#25663 = EDGE_CURVE ( 'NONE', #26954, #27318, #10939, .T. ) ;
#25664 = LINE ( 'NONE', #9535, #14072 ) ;
#25665 = TOROIDAL_SURFACE ( 'NONE', #9516, 2.750000000000000000, 0.1000000000000000056 ) ;
#25667 = DIRECTION ( 'NONE',  ( 3.491481338843133355E-15, -0.000000000000000000, 1.000000000000000000 ) ) ;
#25666 = CARTESIAN_POINT ( 'NONE',  ( 58.74999999305994436, 1.869977652031684423, 0.4744892162742392339 ) ) ;
#25669 = EDGE_CURVE ( 'NONE', #9539, #10988, #20371, .T. ) ;
#25668 = DIRECTION ( 'NONE',  ( 0.000000000000000000, 0.000000000000000000, 1.000000000000000000 ) ) ;
#25670 = ORIENTED_EDGE ( 'NONE', *, *, #18744, .T. ) ;
#25671 = CARTESIAN_POINT ( 'NONE',  ( 52.02275531408258047, 3.834498708141866441, 2.049999999999818190 ) ) ;
#25672 = CARTESIAN_POINT ( 'NONE',  ( 50.36024759664407213, -1.282505688586073056, 3.869483523004606518 ) ) ;
#25673 = SHAPE_REPRESENTATION ( 'Rotator Head', ( #9018 ), #5016 ) ;
#25674 = AXIS2_PLACEMENT_3D ( 'NONE', #23261, #7257, #2524 ) ;
#25675 = AXIS2_PLACEMENT_3D ( 'NONE', #14100, #16328, #31039 ) ;
#25676 = ORIENTED_EDGE ( 'NONE', *, *, #27228, .T. ) ;
#25677 = DIRECTION ( 'NONE',  ( -3.002035892788117459E-16, 0.9996898646859344595, 0.02490330187381124133 ) ) ;
#25678 = ORIENTED_EDGE ( 'NONE', *, *, #16432, .T. ) ;
#25679 = CARTESIAN_POINT ( 'NONE',  ( -71.49999999999998579, -1.395601618875910821E-15, 2.917180974979867506E-15 ) ) ;
#25680 = CARTESIAN_POINT ( 'NONE',  ( 58.65000000000000568, 1.571497941947157084, -1.022750809561052021 ) ) ;
#25681 = EDGE_LOOP ( 'NONE', ( #21765, #28734, #52, #2571, #4240, #276, #8180 ) ) ;
#25682 = CARTESIAN_POINT ( 'NONE',  ( 22.16344984338963897, 7.321836226319897278, 1.949999999999922462 ) ) ;
#25683 = EDGE_CURVE ( 'NONE', #20775, #12730, #22582, .T. ) ;
#25684 = CARTESIAN_POINT ( 'NONE',  ( -57.45655989232412963, -3.925981830489445379, -2.181683956345066863E-13 ) ) ;
#25685 = ORIENTED_EDGE ( 'NONE', *, *, #13535, .F. ) ;
#25686 = CARTESIAN_POINT ( 'NONE',  ( 57.04536243881683788, 0.7794871794871796045, -1.732743413496389939 ) ) ;
#25687 = VERTEX_POINT ( 'NONE', #12905 ) ;
#25688 = ORIENTED_EDGE ( 'NONE', *, *, #19964, .F. ) ;
#25689 = CARTESIAN_POINT ( 'NONE',  ( -55.12499999999997158, 2.944486372867106905, -1.700000000000183364 ) ) ;
#25690 = CARTESIAN_POINT ( 'NONE',  ( -54.44999999999997442, 1.499999999999999556, 4.029888335921975262 ) ) ;
#25691 = CARTESIAN_POINT ( 'NONE',  ( 27.79265796670793875, 5.432811198890464155, -1.425000000000097300 ) ) ;
#25692 = CARTESIAN_POINT ( 'NONE',  ( -35.85663232820584057, 0.4576450603546802220, -5.200000000000000178 ) ) ;
#25693 = EDGE_CURVE ( 'NONE', #15927, #15558, #25582, .T. ) ;
#25694 = DIRECTION ( 'NONE',  ( 0.000000000000000000, 1.000000000000000000, 3.491481338843130594E-15 ) ) ;
#25695 = CIRCLE ( 'NONE', #18124, 3.950000000000000178 ) ;
#25696 = EDGE_CURVE ( 'NONE', #7044, #11180, #28658, .T. ) ;
#25698 = DIRECTION ( 'NONE',  ( 9.654113257610060303E-15, 0.000000000000000000, 1.000000000000000000 ) ) ;
#25697 = CARTESIAN_POINT ( 'NONE',  ( -36.92405921417685732, 5.098435263432259390, -1.807398698456122110 ) ) ;
#25699 = DIRECTION ( 'NONE',  ( 1.000000000000000000, 0.000000000000000000, -1.047444401652940007E-14 ) ) ;
#25700 = CARTESIAN_POINT ( 'NONE',  ( -59.66272163888239533, -2.194198658389501677, 1.525022448910328121 ) ) ;
#25701 = DIRECTION ( 'NONE',  ( 1.000000000000000000, -0.000000000000000000, -0.000000000000000000 ) ) ;
#25702 = EDGE_CURVE ( 'NONE', #10186, #16343, #14980, .T. ) ;
#25703 = CARTESIAN_POINT ( 'NONE',  ( 58.75000000000003553, -1.895722432252686884, -0.6373668173469783094 ) ) ;
#25704 = VERTEX_POINT ( 'NONE', #1353 ) ;
#25706 = FACE_OUTER_BOUND ( 'NONE', #22375, .T. ) ;
#25705 = CARTESIAN_POINT ( 'NONE',  ( 51.25000000000001421, 5.368159983410797313E-13, 3.111507638930570854E-58 ) ) ;
#25707 = EDGE_CURVE ( 'NONE', #24984, #28363, #10554, .T. ) ;
#25708 = FILL_AREA_STYLE ('',( #30599 ) ) ;
#25709 = ORIENTED_EDGE ( 'NONE', *, *, #26274, .F. ) ;
#25710 = CARTESIAN_POINT ( 'NONE',  ( 58.45000000000001705, -0.8000000000000000444, -1.778341924377873751 ) ) ;
#25711 = DIRECTION ( 'NONE',  ( 1.000000000000000000, 0.000000000000000000, -3.469446951953543191E-15 ) ) ;
#25713 = CARTESIAN_POINT ( 'NONE',  ( 56.95000000000001705, 0.7227197132926967971, -2.497551541979256218 ) ) ;
#25712 = CARTESIAN_POINT ( 'NONE',  ( -56.37499999999998579, -3.920666489018338045E-15, 3.399999999999799183 ) ) ;
#25714 = ORIENTED_EDGE ( 'NONE', *, *, #17758, .T. ) ;
#25715 = ORIENTED_EDGE ( 'NONE', *, *, #2364, .T. ) ;
#25716 = AXIS2_PLACEMENT_3D ( 'NONE', #24987, #29584, #5846 ) ;
#25717 = DIRECTION ( 'NONE',  ( 1.000000000000000000, 3.054025858079668409E-16, -2.042474015755241579E-16 ) ) ;
#25718 = ORIENTED_EDGE ( 'NONE', *, *, #2278, .T. ) ;
#25719 = CARTESIAN_POINT ( 'NONE',  ( 58.74999981196286569, -1.734557215427702026, 0.9033020670135759600 ) ) ;
#25720 = VECTOR ( 'NONE', #13402, 1000.000000000000000 ) ;
#25721 = CARTESIAN_POINT ( 'NONE',  ( 54.04962709127927667, 6.684747557764788795, -2.023090456647256730 ) ) ;
#25722 = ORIENTED_EDGE ( 'NONE', *, *, #29139, .T. ) ;
#25723 = CARTESIAN_POINT ( 'NONE',  ( 22.07280086217094706, 8.086143481909150665, -2.050000000000076206 ) ) ;
#25724 = DIRECTION ( 'NONE',  ( -7.604267291953133322E-15, 0.000000000000000000, -1.000000000000000000 ) ) ;
#25725 = DIRECTION ( 'NONE',  ( 3.002035892788116966E-16, -0.9996898646859343485, -0.02490330187381123786 ) ) ;
#25726 = ORIENTED_EDGE ( 'NONE', *, *, #14969, .F. ) ;
#25727 = ORIENTED_EDGE ( 'NONE', *, *, #17397, .F. ) ;
#25728 = CARTESIAN_POINT ( 'NONE',  ( 46.90000017523095011, -4.241673356750442991, -1.073212863078178980 ) ) ;
#25729 = CARTESIAN_POINT ( 'NONE',  ( 51.50435016707359637, -0.9265794315402079429, -1.339215852266877116 ) ) ;
#25730 = CARTESIAN_POINT ( 'NONE',  ( 58.75000000000002132, -0.5380862305913116650, 2.008165151418990213 ) ) ;
#25731 = DIRECTION ( 'NONE',  ( -1.000000000000000000, 0.000000000000000000, 1.047444401652940007E-14 ) ) ;
#25732 = EDGE_CURVE ( 'NONE', #18525, #4586, #22011, .T. ) ;
#25733 = FACE_OUTER_BOUND ( 'NONE', #15932, .T. ) ;
#25734 = ADVANCED_FACE ( 'NONE', ( #25567 ), #26637, .T. ) ;
#25735 = LINE ( 'NONE', #4043, #3536 ) ;
#25736 = EDGE_CURVE ( 'NONE', #19672, #22738, #8410, .T. ) ;
#25737 = PLANE ( 'NONE',  #21594 ) ;
#25739 = DIRECTION ( 'NONE',  ( 1.000000000000000000, 1.047444401652940007E-14, 0.000000000000000000 ) ) ;
#25738 = CARTESIAN_POINT ( 'NONE',  ( -36.48174642953024005, -2.847679722116556622, 4.601476325142769497 ) ) ;
#25740 =( GEOMETRIC_REPRESENTATION_CONTEXT ( 3 ) GLOBAL_UNCERTAINTY_ASSIGNED_CONTEXT ( ( #2841 ) ) GLOBAL_UNIT_ASSIGNED_CONTEXT ( ( #22345, #12070, #26622 ) ) REPRESENTATION_CONTEXT ( 'NONE', 'WORKASPACE' ) );
#25741 = CARTESIAN_POINT ( 'NONE',  ( 51.89999982476908968, -4.241673356750432333, 1.073212863078216506 ) ) ;
#25742 = CARTESIAN_POINT ( 'NONE',  ( 50.80000000000001847, -4.031600731908413948, -1.173113608511851869 ) ) ;
#25743 = CIRCLE ( 'NONE', #14095, 0.1000000000000021150 ) ;
#25744 = CARTESIAN_POINT ( 'NONE',  ( 61.23770293222996486, -0.8897917884435792013, -1.791164585742600179 ) ) ;
#25745 = CARTESIAN_POINT ( 'NONE',  ( 50.35762544161294585, 8.151359338959887069, -2.008578643762865656 ) ) ;
#25746 = ORIENTED_EDGE ( 'NONE', *, *, #24684, .F. ) ;
#25747 = ORIENTED_EDGE ( 'NONE', *, *, #23316, .F. ) ;
#25748 = CARTESIAN_POINT ( 'NONE',  ( 51.06335740850991556, -4.023874009802445251, 1.198297772468548406 ) ) ;
#25749 = VERTEX_POINT ( 'NONE', #15622 ) ;
#25750 = CARTESIAN_POINT ( 'NONE',  ( 52.38400031671219637, 8.538946093000150839, 2.049999999999817302 ) ) ;
#25751 = CARTESIAN_POINT ( 'NONE',  ( -59.34585481156723574, 3.673546848079181970, 0.7533615035078068400 ) ) ;
#25752 = AXIS2_PLACEMENT_3D ( 'NONE', #11869, #29528, #7275 ) ;
#25754 = CARTESIAN_POINT ( 'NONE',  ( -36.68133364217572989, 3.736273719777117197, 3.909490113446847381 ) ) ;
#25753 = DIRECTION ( 'NONE',  ( 0.000000000000000000, -0.2008964009354148039, 0.9796124928211139560 ) ) ;
#25755 = ORIENTED_EDGE ( 'NONE', *, *, #19713, .F. ) ;
#25756 = ORIENTED_EDGE ( 'NONE', *, *, #5611, .T. ) ;
#25757 = CARTESIAN_POINT ( 'NONE',  ( -63.82928932188132620, -2.649178141417726451, -0.06599374996559692619 ) ) ;
#25758 = ORIENTED_EDGE ( 'NONE', *, *, #17860, .F. ) ;
#25759 = CIRCLE ( 'NONE', #2512, 0.1000000000000003803 ) ;
#25760 = ORIENTED_EDGE ( 'NONE', *, *, #9233, .F. ) ;
#25762 = DIRECTION ( 'NONE',  ( -1.000000000000000000, -3.054025858079668409E-16, 2.042474015755241579E-16 ) ) ;
#25761 = LINE ( 'NONE', #18017, #10519 ) ;
#25763 = CARTESIAN_POINT ( 'NONE',  ( 51.87582967299545800, 8.646477722258159915, -2.039222690361161661 ) ) ;
#25764 = ORIENTED_EDGE ( 'NONE', *, *, #2449, .T. ) ;
#25765 = CARTESIAN_POINT ( 'NONE',  ( 53.91574522235882228, 6.672251602522421443, 1.774295301432037286 ) ) ;
#25766 = AXIS2_PLACEMENT_3D ( 'NONE', #20778, #28204, #25498 ) ;
#25767 = CARTESIAN_POINT ( 'NONE',  ( -36.92405921417686443, -3.062358472872079851, 4.459001320275575608 ) ) ;
#25768 = CARTESIAN_POINT ( 'NONE',  ( 57.00000000000001421, 0.6999999999999997335, 1.820027472320129514 ) ) ;
#25769 = PRODUCT_DEFINITION_SHAPE ( 'NONE', 'NONE',  #31332 ) ;
#25770 = CARTESIAN_POINT ( 'NONE',  ( -59.19702994616205416, -2.078460969082657872, 3.599999999999782041 ) ) ;
#25771 = AXIS2_PLACEMENT_3D ( 'NONE', #4544, #14193, #28612 ) ;
#25772 = EDGE_CURVE ( 'NONE', #11223, #11810, #860, .T. ) ;
#25773 = CARTESIAN_POINT ( 'NONE',  ( 15.03925126672132784, 4.018128179617494133, 3.618665901676702656 ) ) ;
#25774 = CARTESIAN_POINT ( 'NONE',  ( -59.23542740578360366, -3.725040285533367523, 1.239922660687668543 ) ) ;
#25775 =( REPRESENTATION_RELATIONSHIP ('NONE','NONE', #7047, #16755 ) REPRESENTATION_RELATIONSHIP_WITH_TRANSFORMATION ( #30709 )SHAPE_REPRESENTATION_RELATIONSHIP( ) );
#25776 = CARTESIAN_POINT ( 'NONE',  ( -59.41132486540516311, 2.423250918913632201, 1.250136525132548027 ) ) ;
#25777 = CARTESIAN_POINT ( 'NONE',  ( 54.31409749668478071, 6.709390224138188863, -2.050000000000189004 ) ) ;
#25778 = CARTESIAN_POINT ( 'NONE',  ( 53.29715246084701619, 4.966963424194753784, 1.611982351028472760 ) ) ;
#25779 = CARTESIAN_POINT ( 'NONE',  ( 60.67929986713512136, 3.641481190980049571E-16, -2.973495046503342287 ) ) ;
#25780 = ORIENTED_EDGE ( 'NONE', *, *, #30363, .T. ) ;
#25781 = AXIS2_PLACEMENT_3D ( 'NONE', #15639, #5657, #27964 ) ;
#25782 = EDGE_CURVE ( 'NONE', #8110, #11505, #21071, .T. ) ;
#25783 = CARTESIAN_POINT ( 'NONE',  ( 58.75000018803716983, 1.651902078983338740, 1.010830333487720223 ) ) ;
#25784 = ORIENTED_EDGE ( 'NONE', *, *, #6121, .F. ) ;
#25785 = DIRECTION ( 'NONE',  ( 0.000000000000000000, -1.224646799147285661E-16, 1.000000000000000000 ) ) ;
#25787 = DIRECTION ( 'NONE',  ( 1.000000000000000000, 0.000000000000000000, 0.000000000000000000 ) ) ;
#25786 = CARTESIAN_POINT ( 'NONE',  ( 58.64999999999999858, 1.932246131438032366, -0.4087173687832937885 ) ) ;
#25788 = PRODUCT_DEFINITION_SHAPE ( 'NONE', 'NONE',  #8557 ) ;
#25789 = ORIENTED_EDGE ( 'NONE', *, *, #13713, .T. ) ;
#25790 = FACE_OUTER_BOUND ( 'NONE', #24247, .T. ) ;
#25791 = FACE_OUTER_BOUND ( 'NONE', #3871, .T. ) ;
#25793 = DIRECTION ( 'NONE',  ( 0.000000000000000000, 0.000000000000000000, 1.000000000000000000 ) ) ;
#25792 = CARTESIAN_POINT ( 'NONE',  ( -61.07202994616202574, 2.078460969082674747, -3.600000000000208367 ) ) ;
#25794 = VERTEX_POINT ( 'NONE', #1815 ) ;
#25795 = CARTESIAN_POINT ( 'NONE',  ( -57.23542740578360366, 2.936324665650207333, 2.606018187048499080 ) ) ;
#25796 = CARTESIAN_POINT ( 'NONE',  ( 50.35762544161296006, 8.151359338959887069, 2.008578643762515714 ) ) ;
#25797 = CARTESIAN_POINT ( 'NONE',  ( -61.39999999999998437, -2.624491116890564690, -0.6340712715164679159 ) ) ;
#25798 =( BOUNDED_CURVE ( )  B_SPLINE_CURVE ( 3, ( #24865, #27253, #27724, #20152 ),
 .UNSPECIFIED., .F., .T. ) 
 B_SPLINE_CURVE_WITH_KNOTS ( ( 4, 4 ),
 ( 4.833974135028384467, 4.924538311792051815 ),
 .UNSPECIFIED. ) 
 CURVE ( )  GEOMETRIC_REPRESENTATION_ITEM ( )  RATIONAL_B_SPLINE_CURVE ( ( 1.000000000000000000, 0.9993166276053078168, 0.9993166276053078168, 1.000000000000000000 ) ) 
 REPRESENTATION_ITEM ( '' )  );
#25799 = FACE_OUTER_BOUND ( 'NONE', #20029, .T. ) ;
#25800 = MANIFOLD_SOLID_BREP ( 'Stock-MAS-683-1', #10470 ) ;
#25801 = CARTESIAN_POINT ( 'NONE',  ( -54.49998548284560940, 1.548795215916124013, -4.063650232134933482 ) ) ;
#25802 = ORIENTED_EDGE ( 'NONE', *, *, #21805, .F. ) ;
#25803 = ADVANCED_FACE ( 'NONE', ( #11491 ), #31063, .F. ) ;
#25804 = CARTESIAN_POINT ( 'NONE',  ( 57.03906491987265781, -0.7487895892850940927, 1.779428968492786867 ) ) ;
#25805 = EDGE_LOOP ( 'NONE', ( #16450, #14919 ) ) ;
#25806 = CARTESIAN_POINT ( 'NONE',  ( -35.85663232820581925, 2.686240680702182360, -4.475885388010699906 ) ) ;
#25807 = CARTESIAN_POINT ( 'NONE',  ( -35.85663232820584057, -0.9159215771349644708, 4.311190327366005270 ) ) ;
#25808 = CARTESIAN_POINT ( 'NONE',  ( 50.80000000000002558, -4.291790910095608425, 1.352971095042303507 ) ) ;
#25809 = AXIS2_PLACEMENT_3D ( 'NONE', #19854, #24437, #15093 ) ;
#25810 = CARTESIAN_POINT ( 'NONE',  ( 16.10660252424456829, -0.2875137064282094479, -5.407399902318746676 ) ) ;
#25812 = CARTESIAN_POINT ( 'NONE',  ( 51.70000000000001705, -0.1421112804877805724, 1.100000000000005862 ) ) ;
#25811 = DIRECTION ( 'NONE',  ( 1.000000000000000000, 1.047444401652940007E-14, 0.000000000000000000 ) ) ;
#25813 = CARTESIAN_POINT ( 'NONE',  ( -59.40362242792826919, 3.375967812128700452, 1.250136525132546916 ) ) ;
#25815 = DIRECTION ( 'NONE',  ( 0.000000000000000000, 0.000000000000000000, 1.000000000000000000 ) ) ;
#25814 = DIRECTION ( 'NONE',  ( 1.000000000000000000, 1.047444401652940007E-14, 0.000000000000000000 ) ) ;
#25816 = ORIENTED_EDGE ( 'NONE', *, *, #3991, .T. ) ;
#25817 = CARTESIAN_POINT ( 'NONE',  ( 47.00000000000003553, 2.428612866367529932E-14, 4.199999999999828759 ) ) ;
#25818 = DIRECTION ( 'NONE',  ( 0.000000000000000000, 0.000000000000000000, -1.000000000000000000 ) ) ;
#25820 = CARTESIAN_POINT ( 'NONE',  ( -35.85663232820600399, 4.683225679163309785, 2.703237727951259828 ) ) ;
#25819 = DIRECTION ( 'NONE',  ( 0.000000000000000000, -1.000000000000000000, -3.491481338843133355E-15 ) ) ;
#25821 = CARTESIAN_POINT ( 'NONE',  ( 51.27134721049148425, 0.9996319491831118231, -1.586319014895851032 ) ) ;
#25822 = VERTEX_POINT ( 'NONE', #28583 ) ;
#25823 = ORIENTED_EDGE ( 'NONE', *, *, #20965, .T. ) ;
#25824 = CARTESIAN_POINT ( 'NONE',  ( -36.89250464418362441, -5.233646053067086079, 1.367284724151337949 ) ) ;
#25825 = CARTESIAN_POINT ( 'NONE',  ( 50.36635169771309961, -1.250438735127598511, 3.874838289045730910 ) ) ;
#25826 = ORIENTED_EDGE ( 'NONE', *, *, #29744, .F. ) ;
#25827 = CARTESIAN_POINT ( 'NONE',  ( 69.20000000000005969, 0.7500000000000000000, 1.988246715072633952 ) ) ;
#25828 = AXIS2_PLACEMENT_3D ( 'NONE', #3229, #6545, #18590 ) ;
#25829 = ADVANCED_FACE ( 'NONE', ( #26366 ), #27841, .T. ) ;
#25830 = ORIENTED_EDGE ( 'NONE', *, *, #17069, .F. ) ;
#25831 = CARTESIAN_POINT ( 'NONE',  ( 58.72204580543392893, 1.874996463826736459, -0.02257357450714411046 ) ) ;
#25832 = ORIENTED_EDGE ( 'NONE', *, *, #20443, .T. ) ;
#25833 = TOROIDAL_SURFACE ( 'NONE', #29881, 4.275000000000000355, 0.1000000000000000056 ) ;
#25834 = CARTESIAN_POINT ( 'NONE',  ( -54.63452994616206126, -3.117691453623976816, 1.799999999999793765 ) ) ;
#25835 = CARTESIAN_POINT ( 'NONE',  ( -57.14405989232411542, 2.944486372867106461, -1.700000000000190248 ) ) ;
#25836 = ORIENTED_EDGE ( 'NONE', *, *, #27126, .F. ) ;
#25837 =( LENGTH_UNIT ( ) NAMED_UNIT ( * ) SI_UNIT ( .MILLI., .METRE. ) );
#25838 = ORIENTED_EDGE ( 'NONE', *, *, #21170, .T. ) ;
#25839 = ORIENTED_EDGE ( 'NONE', *, *, #21949, .F. ) ;
#25840 = EDGE_CURVE ( 'NONE', #23987, #10712, #21574, .T. ) ;
#25841 = CARTESIAN_POINT ( 'NONE',  ( -55.75952994616203995, 3.117691453623994580, -1.800000000000184563 ) ) ;
#25842 = ADVANCED_FACE ( 'NONE', ( #14788 ), #24305, .F. ) ;
#25843 = CARTESIAN_POINT ( 'NONE',  ( -55.08155989232412253, -1.962990915244704260, -3.400000000000203748 ) ) ;
#25844 = DIRECTION ( 'NONE',  ( 1.000000000000000000, -0.000000000000000000, -1.047444401652940007E-14 ) ) ;
#25846 = EDGE_CURVE ( 'NONE', #22862, #15739, #2337, .T. ) ;
#25845 = DIRECTION ( 'NONE',  ( 0.000000000000000000, 0.000000000000000000, 1.000000000000000000 ) ) ;
#25847 = AXIS2_PLACEMENT_3D ( 'NONE', #26701, #19417, #21808 ) ;
#25848 = DIRECTION ( 'NONE',  ( 0.000000000000000000, 0.000000000000000000, -1.000000000000000000 ) ) ;
#25849 = MANIFOLD_SOLID_BREP ( 'Stock-MAS-683-1', #868 ) ;
#25851 = DIRECTION ( 'NONE',  ( 1.000000000000000000, 1.047444401652940007E-14, -0.000000000000000000 ) ) ;
#25850 = CARTESIAN_POINT ( 'NONE',  ( 58.75000000000003553, -1.655311165516937910, 1.077297519403497050 ) ) ;
#25852 = CARTESIAN_POINT ( 'NONE',  ( -61.34999999999997300, -2.635021238245644160, -0.5887810068220489246 ) ) ;
#25853 = DIRECTION ( 'NONE',  ( 0.000000000000000000, 6.217248937900876626E-15, 1.000000000000000000 ) ) ;
#25854 = CARTESIAN_POINT ( 'NONE',  ( 15.66436536804551061, 5.256245472275793418, -1.286369972357296110 ) ) ;
#25855 = CARTESIAN_POINT ( 'NONE',  ( 58.75000000000003553, -1.571497941946114141, -1.022750809560766916 ) ) ;
#25856 = ADVANCED_FACE ( 'NONE', ( #538, #2614 ), #10197, .T. ) ;
#25857 = DIRECTION ( 'NONE',  ( 1.000000000000000000, 3.053848253006669023E-16, -2.042510438544995169E-16 ) ) ;
#25858 = DIRECTION ( 'NONE',  ( 0.7313537016191670181, 0.6819983600625022513, -2.468850131082252327E-15 ) ) ;
#25859 = ORIENTED_EDGE ( 'NONE', *, *, #26532, .T. ) ;
#25861 = CARTESIAN_POINT ( 'NONE',  ( 50.50000002742975624, -0.7904052113206707642, 4.025738854575410919 ) ) ;
#25860 = CARTESIAN_POINT ( 'NONE',  ( 50.95599726996785961, -0.9532299437226279260, -1.316046228059489120 ) ) ;
#25862 = VECTOR ( 'NONE', #28744, 1000.000000000000000 ) ;
#25863 = ORIENTED_EDGE ( 'NONE', *, *, #25086, .T. ) ;
#25864 = CARTESIAN_POINT ( 'NONE',  ( -44.49999999999997868, 1.499999999999999556, -3.300094695611021312 ) ) ;
#25865 = CARTESIAN_POINT ( 'NONE',  ( -61.04792740578359656, 3.330682475591789427, 0.6830477631804114935 ) ) ;
#25866 = CARTESIAN_POINT ( 'NONE',  ( -55.57202994616207548, 2.078460969082646770, 3.599999999999810019 ) ) ;
#25867 = EDGE_LOOP ( 'NONE', ( #11789, #21160, #10285, #25209 ) ) ;
#25868 = EDGE_CURVE ( 'NONE', #10898, #26742, #13483, .T. ) ;
#25869 = ORIENTED_EDGE ( 'NONE', *, *, #5524, .T. ) ;
#25870 = DIRECTION ( 'NONE',  ( 0.000000000000000000, -0.2008964009354162750, 0.9796124928211136229 ) ) ;
#25871 = ORIENTED_EDGE ( 'NONE', *, *, #23794, .F. ) ;
#25872 = LINE ( 'NONE', #26020, #22760 ) ;
#25873 = CIRCLE ( 'NONE', #19321, 0.1500000000000001887 ) ;
#25874 = CARTESIAN_POINT ( 'NONE',  ( -67.99999999999995737, -3.266925685480207642E-16, 2.202315069465528948E-15 ) ) ;
#25875 = ORIENTED_EDGE ( 'NONE', *, *, #2077, .T. ) ;
#25876 = DIRECTION ( 'NONE',  ( -1.000000000000000000, -3.054025858079668409E-16, 2.042474015755241579E-16 ) ) ;
#25877 = CARTESIAN_POINT ( 'NONE',  ( 58.65000000000004121, -1.874150328519937680, 0.06593717335357722475 ) ) ;
#25878 = DIRECTION ( 'NONE',  ( 0.000000000000000000, -0.2008964009354147484, 0.9796124928211139560 ) ) ;
#25879 = ORIENTED_EDGE ( 'NONE', *, *, #25868, .F. ) ;
#25880 = ORIENTED_EDGE ( 'NONE', *, *, #18915, .F. ) ;
#25881 = DIRECTION ( 'NONE',  ( -1.000000000000000000, 0.000000000000000000, 1.047444401652940007E-14 ) ) ;
#25882 = EDGE_CURVE ( 'NONE', #14356, #9001, #18062, .T. ) ;
#25883 = CARTESIAN_POINT ( 'NONE',  ( 51.88812122917401837, 8.998461838226445408, 1.949999999999818767 ) ) ;
#25884 = CARTESIAN_POINT ( 'NONE',  ( 61.01502350126985874, 0.5557829358563669553, -1.706838207573794453 ) ) ;
#25886 = EDGE_CURVE ( 'NONE', #16322, #1490, #19582, .T. ) ;
#25885 = CARTESIAN_POINT ( 'NONE',  ( 51.70000000000002416, 2.428612866367529932E-14, -1.805095852181900386E-13 ) ) ;
#25887 = CARTESIAN_POINT ( 'NONE',  ( 50.25000000000001421, 0.5000000000005263567, -1.863080903343375061 ) ) ;
#25888 = CARTESIAN_POINT ( 'NONE',  ( 57.00841846112073341, 0.7284616547511407747, -1.797128479182910299 ) ) ;
#25890 = CARTESIAN_POINT ( 'NONE',  ( 58.45000000000001705, -0.8000000000000000444, -1.778341924377873751 ) ) ;
#25889 = CARTESIAN_POINT ( 'NONE',  ( -35.85663232820581925, -2.525801270006313715, 4.794550352686329120 ) ) ;
#25891 = CIRCLE ( 'NONE', #16294, 0.05000000000000012768 ) ;
#25892 = CARTESIAN_POINT ( 'NONE',  ( 52.06628335902944826, 0.5434431642986583544, -1.718465885608440269 ) ) ;
#25893 = DIRECTION ( 'NONE',  ( 0.9990482215818580203, 0.008762977932702540121, -0.04273009679227964680 ) ) ;
#25894 = CARTESIAN_POINT ( 'NONE',  ( 61.23883361641919976, -0.8947175514078024028, -1.757895546654327124 ) ) ;
#25895 = CARTESIAN_POINT ( 'NONE',  ( 41.48619405471883681, -151.3359592902622239, -1.950000000000163380 ) ) ;
#25896 = ORIENTED_EDGE ( 'NONE', *, *, #22127, .F. ) ;
#25897 = ORIENTED_EDGE ( 'NONE', *, *, #11692, .T. ) ;
#25898 = DIRECTION ( 'NONE',  ( -1.000000000000000000, -1.047444401652940007E-14, -0.000000000000000000 ) ) ;
#25899 = ORIENTED_EDGE ( 'NONE', *, *, #23903, .F. ) ;
#25900 = CARTESIAN_POINT ( 'NONE',  ( 53.87654288987801721, 4.973000991543902849, 2.049999999999811973 ) ) ;
#25901 = AXIS2_PLACEMENT_3D ( 'NONE', #4720, #28953, #7427 ) ;
#25902 = CARTESIAN_POINT ( 'NONE',  ( -57.84585481156723574, 3.673546848079182414, 0.7533615035078065070 ) ) ;
#25904 = CARTESIAN_POINT ( 'NONE',  ( -36.43290890416756156, 2.776541361171022793, 4.646985486732267745 ) ) ;
#25903 = CARTESIAN_POINT ( 'NONE',  ( -61.34999999999997300, -2.456456838093036055, -0.5843327841101846332 ) ) ;
#25905 = VERTEX_POINT ( 'NONE', #18272 ) ;
#25906 = EDGE_CURVE ( 'NONE', #1993, #19631, #19086, .T. ) ;
#25907 = DIRECTION ( 'NONE',  ( 0.000000000000000000, 0.2008964009354147484, -0.9796124928211140670 ) ) ;
#25908 = ORIENTED_EDGE ( 'NONE', *, *, #29572, .T. ) ;
#25909 = CARTESIAN_POINT ( 'NONE',  ( 58.45000000000001705, 0.8000000000000000444, 1.778341924377873751 ) ) ;
#25910 = ORIENTED_EDGE ( 'NONE', *, *, #15854, .F. ) ;
#25911 = APPLICATION_CONTEXT ( 'automotive_design' ) ;
#25913 = CARTESIAN_POINT ( 'NONE',  ( 58.64999999999999858, 1.877732920581776321, -0.6121634413828938026 ) ) ;
#25912 = DIRECTION ( 'NONE',  ( 1.000000000000000000, 3.054025858079668409E-16, -2.042474015755241579E-16 ) ) ;
#25914 = ADVANCED_FACE ( 'NONE', ( #30121 ), #23618, .T. ) ;
#25915 = ORIENTED_EDGE ( 'NONE', *, *, #5560, .F. ) ;
#25916 = CARTESIAN_POINT ( 'NONE',  ( 57.00000000000001421, -0.7256836306366275524, 1.800271087100996592 ) ) ;
#25917 = FACE_OUTER_BOUND ( 'NONE', #10490, .T. ) ;
#25918 = CARTESIAN_POINT ( 'NONE',  ( -59.40619059199517693, 3.371123259826405594, 1.250136525132546694 ) ) ;
#25919 = CARTESIAN_POINT ( 'NONE',  ( -44.59999999999997300, 8.366749974758367693E-15, -1.870876429524646202E-13 ) ) ;
#25920 = CARTESIAN_POINT ( 'NONE',  ( -56.32202994616206126, 2.078460969082646770, 3.599999999999807354 ) ) ;
#25922 = EDGE_CURVE ( 'NONE', #11599, #23041, #22601, .T. ) ;
#25921 = CARTESIAN_POINT ( 'NONE',  ( 51.82417406112929115, 0.5144554499007042425, 4.312884176178978457 ) ) ;
#25923 = CARTESIAN_POINT ( 'NONE',  ( 61.25000000000001421, 1.039502773797226221, -1.800471618823823450 ) ) ;
#25924 = CARTESIAN_POINT ( 'NONE',  ( 58.75000000000001421, 0.6121634413823869858, 1.877732920581527631 ) ) ;
#25925 = VECTOR ( 'NONE', #9725, 1000.000000000000000 ) ;
#25926 = CARTESIAN_POINT ( 'NONE',  ( -57.04792740578359656, -2.256877952708267188, 2.542931754211920747 ) ) ;
#25927 = DIRECTION ( 'NONE',  ( -1.000000000000000000, -0.000000000000000000, 1.047444401652940007E-14 ) ) ;
#25928 = ORIENTED_EDGE ( 'NONE', *, *, #24867, .T. ) ;
#25929 = DIRECTION ( 'NONE',  ( 1.000000000000000000, 1.047444401652940007E-14, 0.000000000000000000 ) ) ;
#25930 = CARTESIAN_POINT ( 'NONE',  ( 51.25000000000001421, 1.100000000000537215, 1.196087371390568643 ) ) ;
#25931 = PLANE ( 'NONE',  #15628 ) ;
#25932 = CARTESIAN_POINT ( 'NONE',  ( 48.30000000000002558, 0.6462379109120994780, -4.048750000000022276 ) ) ;
#25933 = ORIENTED_EDGE ( 'NONE', *, *, #31168, .T. ) ;
#25934 = CARTESIAN_POINT ( 'NONE',  ( 58.72204580543402130, 1.635081356933473895, 0.9179489429359590780 ) ) ;
#25935 = ORIENTED_EDGE ( 'NONE', *, *, #6255, .F. ) ;
#25936 = FACE_OUTER_BOUND ( 'NONE', #25218, .T. ) ;
#25938 = CARTESIAN_POINT ( 'NONE',  ( 58.75000000694009827, -1.381609951798472791, 1.346330794794275310 ) ) ;
#25937 = CARTESIAN_POINT ( 'NONE',  ( -57.68749999999996447, -3.399999999999991029, -2.155011314204633625E-13 ) ) ;
#25939 = VERTEX_POINT ( 'NONE', #1307 ) ;
#25940 = EDGE_CURVE ( 'NONE', #107, #24006, #12475, .T. ) ;
#25941 = EDGE_LOOP ( 'NONE', ( #5298, #6305, #21101, #30135, #2837 ) ) ;
#25942 = CARTESIAN_POINT ( 'NONE',  ( 49.05000000000002558, 1.401298464324817071E-42, -5.137714790107672405E-13 ) ) ;
#25943 = EDGE_CURVE ( 'NONE', #17250, #19589, #16100, .T. ) ;
#25944 = DIRECTION ( 'NONE',  ( 0.000000000000000000, -0.000000000000000000, 1.000000000000000000 ) ) ;
#25946 = DIRECTION ( 'NONE',  ( 0.000000000000000000, -0.9996898646859343485, -0.02490330187381124133 ) ) ;
#25945 = FACE_OUTER_BOUND ( 'NONE', #4145, .T. ) ;
#25947 = ADVANCED_FACE ( 'NONE', ( #8595 ), #17559, .F. ) ;
#25948 = ORIENTED_EDGE ( 'NONE', *, *, #487, .T. ) ;
#25949 = CARTESIAN_POINT ( 'NONE',  ( -56.62499999999997158, 1.184343223768590470, 3.558065644182724974 ) ) ;
#25950 = CARTESIAN_POINT ( 'NONE',  ( -36.52757395963739384, 3.857619034241715816, 3.790808625284063815 ) ) ;
#25951 = SHAPE_DEFINITION_REPRESENTATION ( #2990, #549 ) ;
#25952 = CARTESIAN_POINT ( 'NONE',  ( -44.59999999999995879, 1.400000000000023892, -4.029888335922147569 ) ) ;
#25953 = CARTESIAN_POINT ( 'NONE',  ( -62.05955358283408430, -2.690595597012027884, 0.2275897585651485699 ) ) ;
#25954 = VERTEX_POINT ( 'NONE', #29661 ) ;
#25955 = EDGE_CURVE ( 'NONE', #2034, #10008, #847, .T. ) ;
#25956 = CARTESIAN_POINT ( 'NONE',  ( 65.00000000000005684, 4.286263797014710090E-16, 3.499999999999318767 ) ) ;
#25957 = CARTESIAN_POINT ( 'NONE',  ( -36.11187263677958725, 3.378578820313965281, -3.972872285093680844 ) ) ;
#25958 = CARTESIAN_POINT ( 'NONE',  ( 58.66133336607592952, -1.640092727267175698, -0.9092995659212040893 ) ) ;
#25959 = CARTESIAN_POINT ( 'NONE',  ( 58.75000000000002132, 6.153735859711025284E-13, 3.111507638930570854E-58 ) ) ;
#25960 = DIRECTION ( 'NONE',  ( -3.491481338843133355E-15, -3.491481338843133355E-15, 1.000000000000000000 ) ) ;
#25962 = CARTESIAN_POINT ( 'NONE',  ( 58.65000000000004121, -1.782657835994226225, -0.5811678240974795795 ) ) ;
#25961 = LINE ( 'NONE', #13603, #21123 ) ;
#25963 = PRODUCT_RELATED_PRODUCT_CATEGORY ( 'part', '', ( #11652 ) ) ;
#25964 = CIRCLE ( 'NONE', #30518, 2.000000000000000000 ) ;
#25965 = DIRECTION ( 'NONE',  ( -1.000000000000000000, -0.000000000000000000, 3.491481338843133355E-15 ) ) ;
#25967 = DIRECTION ( 'NONE',  ( 3.304235192336781034E-15, 0.000000000000000000, 1.000000000000000000 ) ) ;
#25966 = CARTESIAN_POINT ( 'NONE',  ( 33.47623932017462778, 4.018128179617509232, 3.618665901676689778 ) ) ;
#25968 = EDGE_LOOP ( 'NONE', ( #10498, #2075, #8833 ) ) ;
#25969 = DIRECTION ( 'NONE',  ( 0.000000000000000000, -1.509903313490210686E-14, 1.000000000000000000 ) ) ;
#25970 = DIRECTION ( 'NONE',  ( 3.016910393003118404E-15, 0.000000000000000000, 1.000000000000000000 ) ) ;
#25972 = CARTESIAN_POINT ( 'NONE',  ( -56.33155989232412963, 3.400000000000008349, -1.856946929144785632E-13 ) ) ;
#25971 = DIRECTION ( 'NONE',  ( -1.000000000000000000, -0.000000000000000000, -0.000000000000000000 ) ) ;
#25973 = CARTESIAN_POINT ( 'NONE',  ( -69.22071067811863543, -0.4218824419643721901, 2.057186234924341939 ) ) ;
#25974 = ORIENTED_EDGE ( 'NONE', *, *, #2930, .F. ) ;
#25975 = VERTEX_POINT ( 'NONE', #3842 ) ;
#25976 = CARTESIAN_POINT ( 'NONE',  ( 47.10000000000000853, -3.637377585518695611, -2.099877210783201331 ) ) ;
#25977 = CARTESIAN_POINT ( 'NONE',  ( 50.30000000000001847, -1.391941090707485396, 3.850000000000022737 ) ) ;
#25978 = ADVANCED_FACE ( 'NONE', ( #8443 ), #4393, .F. ) ;
#25979 =( BOUNDED_SURFACE ( )  B_SPLINE_SURFACE ( 3, 2, ( 
 ( #14322, #9746, #23996 ),
 ( #14486, #2138, #19408 ),
 ( #28900, #29052, #17039 ),
 ( #24309, #2616, #26835 ),
 ( #26213, #9893, #6899 ),
 ( #11802, #19573, #31110 ),
 ( #394, #5137, #2295 ),
 ( #14790, #22101, #16566 ) ),
 .UNSPECIFIED., .F., .F., .F. ) 
 B_SPLINE_SURFACE_WITH_KNOTS ( ( 4, 2, 2, 4 ),
 ( 3, 3 ),
 ( 0.001762834131042899637, 0.001945267826973971379, 0.002127701522905043122, 0.002492568914767187040 ),
 ( 0.000000000000000000, 1.000000000000000000 ),
 .UNSPECIFIED. ) 
 GEOMETRIC_REPRESENTATION_ITEM ( )  RATIONAL_B_SPLINE_SURFACE ( (
 ( 1.000000000000000000, 0.8699658093904929501, 1.000000000000000000),
 ( 1.000000000000000000, 0.8851796357839230023, 1.000000000000000000),
 ( 1.000000000000000000, 0.8977447492167212051, 1.000000000000000000),
 ( 1.000000000000000000, 0.9127836411835494879, 1.000000000000000000),
 ( 1.000000000000000000, 0.9151168517135812586, 1.000000000000000000),
 ( 1.000000000000000000, 0.9045976586032165034, 1.000000000000000000),
 ( 1.000000000000000000, 0.8745315534097227728, 1.000000000000000000),
 ( 1.000000000000000000, 0.8388746406931710808, 1.000000000000000000) ) ) 
 REPRESENTATION_ITEM ( '' )  SURFACE ( )  );
#25980 = ORIENTED_EDGE ( 'NONE', *, *, #7666, .F. ) ;
#25981 = CARTESIAN_POINT ( 'NONE',  ( 58.75000000000001421, 0.5000000000004131140, 1.863080903344439321 ) ) ;
#25982 = ORIENTED_EDGE ( 'NONE', *, *, #27474, .T. ) ;
#25983 = DIRECTION ( 'NONE',  ( -2.614375865348240525E-16, 0.2008964009354147762, -0.9796124928211140670 ) ) ;
#25984 = ORIENTED_EDGE ( 'NONE', *, *, #2655, .F. ) ;
#25985 = CARTESIAN_POINT ( 'NONE',  ( -57.01905989232412963, 2.944486372867092250, 1.699999999999808553 ) ) ;
#25986 = ORIENTED_EDGE ( 'NONE', *, *, #24907, .T. ) ;
#25987 = CARTESIAN_POINT ( 'NONE',  ( 0.000000000000000000, 0.000000000000000000, 0.000000000000000000 ) ) ;
#25988 = ORIENTED_EDGE ( 'NONE', *, *, #20495, .F. ) ;
#25989 = AXIS2_PLACEMENT_3D ( 'NONE', #31324, #24208, #11850 ) ;
#25990 = ORIENTED_EDGE ( 'NONE', *, *, #10190, .T. ) ;
#25991 = EDGE_CURVE ( 'NONE', #1787, #27011, #14496, .T. ) ;
#25992 = CARTESIAN_POINT ( 'NONE',  ( -55.88452994616203995, 2.093608279459368564E-14, -3.600000000000198597 ) ) ;
#25993 = CARTESIAN_POINT ( 'NONE',  ( -60.54800159808252147, 0.7228413094357374336, -3.524724055549727897 ) ) ;
#25994 = DIRECTION ( 'NONE',  ( 0.000000000000000000, 0.000000000000000000, 1.000000000000000000 ) ) ;
#25995 = CARTESIAN_POINT ( 'NONE',  ( -60.59999999999997300, 1.626093840209163176E-15, 1.891350188320046374E-15 ) ) ;
#25996 = CIRCLE ( 'NONE', #24479, 4.849999999999999645 ) ;
#25997 = FACE_OUTER_BOUND ( 'NONE', #23860, .T. ) ;
#25999 = CARTESIAN_POINT ( 'NONE',  ( -57.93749999999997158, -4.108500314926509134, 1.367561758111401016 ) ) ;
#25998 = CARTESIAN_POINT ( 'NONE',  ( -44.49999999999998579, 9.184850993650734737E-17, 0.7500000000000185407 ) ) ;
#26000 = CARTESIAN_POINT ( 'NONE',  ( -44.49999999999997868, -6.102218906431391608E-14, -1.867384948185805656E-13 ) ) ;
#26001 = CARTESIAN_POINT ( 'NONE',  ( 51.80000000000001137, -4.003661535119149129, -1.269131321892099207 ) ) ;
#26002 = CARTESIAN_POINT ( 'NONE',  ( -36.40878371307407235, -3.917459231545681764, -3.727878977586817744 ) ) ;
#26003 = CARTESIAN_POINT ( 'NONE',  ( 58.65263613458545677, -1.656197658588108856, -0.8791532451975312412 ) ) ;
#26004 = DIRECTION ( 'NONE',  ( 0.000000000000000000, -1.000000000000000000, 0.000000000000000000 ) ) ;
#26005 = TOROIDAL_SURFACE ( 'NONE', #12354, 0.3000000000000000444, 0.05000000000000000278 ) ;
#26006 = CARTESIAN_POINT ( 'NONE',  ( 60.87794714816571684, -0.5123471864359163686, 1.858409133840800198 ) ) ;
#26007 = VERTEX_POINT ( 'NONE', #10975 ) ;
#26009 = CARTESIAN_POINT ( 'NONE',  ( -54.49999999999996447, 1.433333333333357329, -4.054078878803077934 ) ) ;
#26008 = CARTESIAN_POINT ( 'NONE',  ( 54.15673930838963912, 5.684321142249388892, 2.049999999999811529 ) ) ;
#26010 = DIRECTION ( 'NONE',  ( 0.000000000000000000, 0.000000000000000000, 1.000000000000000000 ) ) ;
#26011 = ADVANCED_FACE ( 'NONE', ( #10668 ), #23183, .F. ) ;
#26012 = VERTEX_POINT ( 'NONE', #853 ) ;
#26013 = CARTESIAN_POINT ( 'NONE',  ( 58.45000000000001705, 0.8000000000000000444, 1.778341924377873751 ) ) ;
#26014 = DIRECTION ( 'NONE',  ( 1.000000000000000000, -0.000000000000000000, -1.047444401652940007E-14 ) ) ;
#26015 = CARTESIAN_POINT ( 'NONE',  ( -55.13452994616203995, 2.093608279459367933E-14, -3.600000000000195932 ) ) ;
#26016 = ORIENTED_EDGE ( 'NONE', *, *, #2865, .T. ) ;
#26017 = VERTEX_POINT ( 'NONE', #3390 ) ;
#26018 = CARTESIAN_POINT ( 'NONE',  ( 15.74504787372188552, 5.074157625981753128, 1.874066637979887373 ) ) ;
#26019 = EDGE_LOOP ( 'NONE', ( #9806, #2154, #11001, #19282, #7292, #8457, #14184, #18453 ) ) ;
#26020 = CARTESIAN_POINT ( 'NONE',  ( -54.49999999999996447, 1.400000000000023892, -4.029888335922182208 ) ) ;
#26021 = DIRECTION ( 'NONE',  ( 0.5633368246415009217, 0.8262273428075537218, 0.000000000000000000 ) ) ;
#26022 = ORIENTED_EDGE ( 'NONE', *, *, #12017, .F. ) ;
#26023 = CARTESIAN_POINT ( 'NONE',  ( 58.45000000000001705, -0.8000000000000002665, -2.421260002560650104 ) ) ;
#26024 = B_SPLINE_CURVE_WITH_KNOTS ( 'NONE', 3,
 ( #2102, #30769, #1619, #20961, #9079, #9243, #28241, #14293, #18753, #28395, #7182, #11451, #23962, #23482 ),
 .UNSPECIFIED., .F., .F.,
 ( 4, 2, 2, 2, 2, 2, 4 ),
 ( 0.000000000000000000, 0.0003953907277084696219, 0.0005930860915627040805, 0.0006919337734898216080, 0.0007413576144533806428, 0.0007660695349351558233, 0.0007907814554169310039 ),
 .UNSPECIFIED. ) ;
#26025 = CARTESIAN_POINT ( 'NONE',  ( 50.25000000000001421, 0.5380862305914526633, -2.008165151417984351 ) ) ;
#26026 = STYLED_ITEM ( 'NONE', ( #30138 ), #5173 ) ;
#26027 = PLANE ( 'NONE',  #11126 ) ;
#26028 = VERTEX_POINT ( 'NONE', #10522 ) ;
#26029 = EDGE_LOOP ( 'NONE', ( #19227, #10072, #10751, #27652 ) ) ;
#26030 = EDGE_CURVE ( 'NONE', #2983, #29251, #29824, .T. ) ;
#26031 = CARTESIAN_POINT ( 'NONE',  ( 47.00000000000002132, -4.259181259350203419, -1.100000000000000089 ) ) ;
#26032 = CARTESIAN_POINT ( 'NONE',  ( -62.09999999999997300, -2.733115994082214950, 0.2227785043249702612 ) ) ;
#26034 = CARTESIAN_POINT ( 'NONE',  ( -54.69184846062112371, 0.2309624077929086361, 3.875409454552791733 ) ) ;
#26033 = VECTOR ( 'NONE', #24430, 1000.000000000000000 ) ;
#26035 = ORIENTED_EDGE ( 'NONE', *, *, #13771, .T. ) ;
#26036 = DIRECTION ( 'NONE',  ( 1.047444401652940007E-14, 0.000000000000000000, 1.000000000000000000 ) ) ;
#26037 = CARTESIAN_POINT ( 'NONE',  ( 50.25000000000002132, 5.263408118306026973E-13, 3.111507638930570854E-58 ) ) ;
#26038 = DIRECTION ( 'NONE',  ( -4.746078037389309365E-15, 0.4531102586351761219, -0.8914544820233751832 ) ) ;
#26039 = CIRCLE ( 'NONE', #5285, 0.1500000000000001887 ) ;
#26040 = DIRECTION ( 'NONE',  ( 0.000000000000000000, 0.000000000000000000, 1.000000000000000000 ) ) ;
#26042 = DIRECTION ( 'NONE',  ( -0.000000000000000000, 0.000000000000000000, -1.000000000000000000 ) ) ;
#26041 = CARTESIAN_POINT ( 'NONE',  ( 58.72202590147323065, -0.4851612519489579833, -1.811144268316629447 ) ) ;
#26043 = EDGE_CURVE ( 'NONE', #4648, #14207, #29655, .T. ) ;
#26044 = PRODUCT_DEFINITION_SHAPE ( 'NONE', 'NONE',  #14745 ) ;
#26045 = CARTESIAN_POINT ( 'NONE',  ( -55.06249999999997158, -0.7533615035078029543, 3.673546848079176197 ) ) ;
#26046 = CYLINDRICAL_SURFACE ( 'NONE', #10508, 3.200000000000000178 ) ;
#26047 = LINE ( 'NONE', #11314, #29946 ) ;
#26048 = ORIENTED_EDGE ( 'NONE', *, *, #11056, .F. ) ;
#26049 = AXIS2_PLACEMENT_3D ( 'NONE', #23653, #28710, #26327 ) ;
#26050 = AXIS2_PLACEMENT_3D ( 'NONE', #10637, #5416, #20314 ) ;
#26051 = EDGE_CURVE ( 'NONE', #11593, #11104, #16547, .T. ) ;
#26052 = CARTESIAN_POINT ( 'NONE',  ( 58.66054497608050866, 0.5000000000006143974, -1.807104036850122109 ) ) ;
#26053 = VERTEX_POINT ( 'NONE', #16352 ) ;
#26054 = MANIFOLD_SOLID_BREP ( 'Stock-MAS-683-1', #30700 ) ;
#26055 = EDGE_CURVE ( 'NONE', #23943, #10453, #6410, .T. ) ;
#26056 = CARTESIAN_POINT ( 'NONE',  ( 52.41206581543988108, 8.644163850305695007, 2.049999999999817302 ) ) ;
#26057 = CARTESIAN_POINT ( 'NONE',  ( -56.47085481156723574, 2.489203624310592389, -2.804704140674919355 ) ) ;
#26059 = CARTESIAN_POINT ( 'NONE',  ( 51.06382050520482352, -3.930543434675132008, -1.171429914303246056 ) ) ;
#26058 = DIRECTION ( 'NONE',  ( 1.000000000000000000, 1.047444401652940007E-14, 0.000000000000000000 ) ) ;
#26060 = EDGE_CURVE ( 'NONE', #20284, #10512, #13986, .T. ) ;
#26061 = ORIENTED_EDGE ( 'NONE', *, *, #23212, .F. ) ;
#26062 = VERTEX_POINT ( 'NONE', #23953 ) ;
#26063 = DIRECTION ( 'NONE',  ( -2.614375865348241018E-16, 0.2008964009354147762, -0.9796124928211140670 ) ) ;
#26064 = ORIENTED_EDGE ( 'NONE', *, *, #25886, .T. ) ;
#26065 = TOROIDAL_SURFACE ( 'NONE', #12403, 2.824999999999998845, 0.05000000000000000278 ) ;
#26066 = CARTESIAN_POINT ( 'NONE',  ( 51.25000000000002842, -1.099999999999462963, -1.196087371390569087 ) ) ;
#26067 = VERTEX_POINT ( 'NONE', #25998 ) ;
#26069 = LINE ( 'NONE', #18962, #13007 ) ;
#26068 = CARTESIAN_POINT ( 'NONE',  ( -36.00197790576392975, 4.683225679163309785, 2.703237727951257607 ) ) ;
#26070 = AXIS2_PLACEMENT_3D ( 'NONE', #3326, #15046, #24851 ) ;
#26071 = VERTEX_POINT ( 'NONE', #23329 ) ;
#26072 = FACE_OUTER_BOUND ( 'NONE', #7675, .T. ) ;
#26073 = FACE_BOUND ( 'NONE', #23882, .T. ) ;
#26074 = CARTESIAN_POINT ( 'NONE',  ( -54.49454330418567594, -1.526701536696945860, -3.317245250669463630 ) ) ;
#26075 = CARTESIAN_POINT ( 'NONE',  ( 57.05000000000001137, 0.7794871794871797155, -1.732743413496401930 ) ) ;
#26076 = CARTESIAN_POINT ( 'NONE',  ( -58.32202994616204705, -4.156921938165296204, -2.220106322563329850E-13 ) ) ;
#26077 = CARTESIAN_POINT ( 'NONE',  ( 51.80000000000001847, 1.521694824349937303, 3.995005614707771269 ) ) ;
#26078 = VECTOR ( 'NONE', #766, 1000.000000000000000 ) ;
#26079 = AXIS2_PLACEMENT_3D ( 'NONE', #25808, #19014, #28018 ) ;
#26080 = DIRECTION ( 'NONE',  ( 0.000000000000000000, 1.000000000000000000, 0.000000000000000000 ) ) ;
#26081 = DIRECTION ( 'NONE',  ( -0.000000000000000000, 0.9495137264943719346, -0.3137254901960807585 ) ) ;
#26083 = EDGE_CURVE ( 'NONE', #11180, #833, #22111, .T. ) ;
#26082 = AXIS2_PLACEMENT_3D ( 'NONE', #2829, #9974, #12325 ) ;
#26084 = VECTOR ( 'NONE', #18741, 1000.000000000000000 ) ;
#26085 = CARTESIAN_POINT ( 'NONE',  ( -57.48542740578360366, 0.7887156198831770659, -3.845940847736172064 ) ) ;
#26086 = AXIS2_PLACEMENT_3D ( 'NONE', #25142, #13565, #3921 ) ;
#26088 = EDGE_CURVE ( 'NONE', #9001, #16975, #29493, .T. ) ;
#26087 = CARTESIAN_POINT ( 'NONE',  ( -55.81249999999997868, -0.7533615035078013999, 3.673546848079176641 ) ) ;
#26089 = ORIENTED_EDGE ( 'NONE', *, *, #646, .F. ) ;
#26090 = CARTESIAN_POINT ( 'NONE',  ( -44.59999999999996589, -1.399999999999979039, -3.959797974644846619 ) ) ;
#26091 = CARTESIAN_POINT ( 'NONE',  ( -36.77443515226921278, -0.6016956010317862091, 5.375730734456589666 ) ) ;
#26092 = DIRECTION ( 'NONE',  ( -1.000000000000000000, -0.000000000000000000, 0.000000000000000000 ) ) ;
#26093 = ORIENTED_EDGE ( 'NONE', *, *, #22553, .T. ) ;
#26094 = CARTESIAN_POINT ( 'NONE',  ( -36.14490256869204643, -5.374748457514320954, 0.5963382560600137827 ) ) ;
#26095 = ORIENTED_EDGE ( 'NONE', *, *, #10974, .T. ) ;
#26096 = CARTESIAN_POINT ( 'NONE',  ( -54.49999999999997868, -3.188085654472696540, 1.181570928782897267 ) ) ;
#26097 = DIRECTION ( 'NONE',  ( 2.117927888850091331E-16, -0.02490330187381135929, 0.9996898646859343485 ) ) ;
#26098 = ADVANCED_FACE ( 'NONE', ( #16038 ), #28142, .F. ) ;
#26099 = VERTEX_POINT ( 'NONE', #23652 ) ;
#26100 = CIRCLE ( 'NONE', #12438, 0.2000000000000000944 ) ;
#26101 = VERTEX_POINT ( 'NONE', #4001 ) ;
#26102 = CARTESIAN_POINT ( 'NONE',  ( -59.64457535546588218, -2.323701065654765419, -1.273936166954769300 ) ) ;
#26103 = CARTESIAN_POINT ( 'NONE',  ( -45.15971931043468146, 14.70000000000000107, 0.000000000000000000 ) ) ;
#26104 = VECTOR ( 'NONE', #7026, 1000.000000000000000 ) ;
#26106 = CARTESIAN_POINT ( 'NONE',  ( 58.65000000000004121, -1.278599783849087235, 1.371849028670080184 ) ) ;
#26105 = DIRECTION ( 'NONE',  ( -0.9993908270190957621, 0.03489949670250097613, 3.491481338843133355E-15 ) ) ;
#26107 = ORIENTED_EDGE ( 'NONE', *, *, #5788, .T. ) ;
#26108 = CARTESIAN_POINT ( 'NONE',  ( -56.87499999999997158, 2.489203624310591056, -2.804704140674918023 ) ) ;
#26109 = CARTESIAN_POINT ( 'NONE',  ( 50.87477060347374902, 8.633605004118187765, 1.549999999999822631 ) ) ;
#26110 = CYLINDRICAL_SURFACE ( 'NONE', #7193, 2.000000000000000000 ) ;
#26111 = CIRCLE ( 'NONE', #5380, 0.1000000000000000888 ) ;
#26112 = CIRCLE ( 'NONE', #19559, 3.524999999999996358 ) ;
#26113 = DIRECTION ( 'NONE',  ( 1.000000000000000000, 0.000000000000000000, -3.491481338843133355E-15 ) ) ;
#26114 = FACE_OUTER_BOUND ( 'NONE', #15506, .T. ) ;
#26115 = CARTESIAN_POINT ( 'NONE',  ( 51.24551381660813831, -1.093420264358021532, 1.202138525661323731 ) ) ;
#26116 = VERTEX_POINT ( 'NONE', #25850 ) ;
#26117 = CARTESIAN_POINT ( 'NONE',  ( 57.00841846112073341, -0.7284616547511407747, 1.797128479182910299 ) ) ;
#26118 = AXIS2_PLACEMENT_3D ( 'NONE', #30435, #25699, #4006 ) ;
#26119 = CARTESIAN_POINT ( 'NONE',  ( -36.42771574642738841, 2.777216423308057625, -4.646230875016845729 ) ) ;
#26120 = CARTESIAN_POINT ( 'NONE',  ( 57.00000000000001421, -0.6999999999999999556, -2.452039967047845437 ) ) ;
#26121 = FACE_OUTER_BOUND ( 'NONE', #2035, .T. ) ;
#26122 = EDGE_CURVE ( 'NONE', #4199, #21532, #13647, .T. ) ;
#26123 = VECTOR ( 'NONE', #9203, 1000.000000000000000 ) ;
#26124 = AXIS2_PLACEMENT_3D ( 'NONE', #31073, #29018, #14762 ) ;
#26125 = EDGE_CURVE ( 'NONE', #27518, #26053, #20600, .T. ) ;
#26126 = FACE_OUTER_BOUND ( 'NONE', #8454, .T. ) ;
#26127 = VECTOR ( 'NONE', #9202, 1000.000000000000000 ) ;
#26129 = EDGE_CURVE ( 'NONE', #4296, #6099, #28679, .T. ) ;
#26128 = CARTESIAN_POINT ( 'NONE',  ( -44.49999999999996447, -1.599999999999981215, -3.363870538531657406 ) ) ;
#26130 = CARTESIAN_POINT ( 'NONE',  ( 47.19756905715325956, -4.191177329985519506, -1.624749424009585885 ) ) ;
#26131 = AXIS2_PLACEMENT_3D ( 'NONE', #28668, #15989, #30880 ) ;
#26133 = CARTESIAN_POINT ( 'NONE',  ( 33.47623932017462778, -2.199885893005926185, -4.939696249117692339 ) ) ;
#26132 = CARTESIAN_POINT ( 'NONE',  ( 54.28867365409859502, 5.640057820322912363, -2.050000000000189004 ) ) ;
#26134 = ORIENTED_EDGE ( 'NONE', *, *, #10851, .T. ) ;
#26135 = DIRECTION ( 'NONE',  ( 0.000000000000000000, 0.000000000000000000, 1.000000000000000000 ) ) ;
#26136 = AXIS2_PLACEMENT_3D ( 'NONE', #9743, #2134, #11796 ) ;
#26137 =( BOUNDED_SURFACE ( )  B_SPLINE_SURFACE ( 3, 2, ( 
 ( #23552, #1540, #13392 ),
 ( #15941, #25601, #27838 ),
 ( #30835, #30499, #11344 ),
 ( #25768, #23401, #20873 ) ),
 .UNSPECIFIED., .F., .F., .F. ) 
 B_SPLINE_SURFACE_WITH_KNOTS ( ( 4, 4 ),
 ( 3, 3 ),
 ( 6.291704175186453303E-05, 0.0002258017310250082428 ),
 ( 0.000000000000000000, 1.000000000000000000 ),
 .UNSPECIFIED. ) 
 GEOMETRIC_REPRESENTATION_ITEM ( )  RATIONAL_B_SPLINE_SURFACE ( (
 ( 1.000000000000000000, 0.8397191227596314533, 1.000000000000000000),
 ( 1.000000000000000000, 0.8408372669632975249, 1.000000000000000000),
 ( 1.000000000000000000, 0.7715695853058209819, 1.000000000000000000),
 ( 1.000000000000000000, 0.7071067811864981678, 1.000000000000000000) ) ) 
 REPRESENTATION_ITEM ( '' )  SURFACE ( )  );
#26138 = DIRECTION ( 'NONE',  ( 0.000000000000000000, 0.000000000000000000, 1.000000000000000000 ) ) ;
#26140 = CARTESIAN_POINT ( 'NONE',  ( -36.80043232705879319, 5.283830060792378269, 1.151642405604297981 ) ) ;
#26139 = CARTESIAN_POINT ( 'NONE',  ( 15.17214319754843110, -2.686240675664388622, -4.475885398016685279 ) ) ;
#26141 = LINE ( 'NONE', #30737, #27668 ) ;
#26142 = ORIENTED_EDGE ( 'NONE', *, *, #24476, .F. ) ;
#26143 = VERTEX_POINT ( 'NONE', #29170 ) ;
#26144 = CARTESIAN_POINT ( 'NONE',  ( -36.22955757456080761, -4.863043649742761154, 1.860644097022644994 ) ) ;
#26145 = FACE_OUTER_BOUND ( 'NONE', #21269, .T. ) ;
#26146 = EDGE_CURVE ( 'NONE', #21339, #29648, #793, .T. ) ;
#26147 = VERTEX_POINT ( 'NONE', #19370 ) ;
#26148 = CARTESIAN_POINT ( 'NONE',  ( -60.49999999999997868, 2.624185894800579621, 0.06537116741875470538 ) ) ;
#26149 = VECTOR ( 'NONE', #22665, 1000.000000000000000 ) ;
#26150 = ORIENTED_EDGE ( 'NONE', *, *, #21867, .F. ) ;
#26151 = CARTESIAN_POINT ( 'NONE',  ( 58.72427158855713003, 1.874564523102884017, -0.04519892032209443800 ) ) ;
#26152 = VERTEX_POINT ( 'NONE', #24110 ) ;
#26153 =( NAMED_UNIT ( * ) SI_UNIT ( $, .STERADIAN. ) SOLID_ANGLE_UNIT ( ) );
#26154 = AXIS2_PLACEMENT_3D ( 'NONE', #12457, #12768, #10571 ) ;
#26155 = CARTESIAN_POINT ( 'NONE',  ( 51.67599336825460199, -3.859587729118648447, -1.644141655455117368 ) ) ;
#26156 = ORIENTED_EDGE ( 'NONE', *, *, #111, .T. ) ;
#26157 = AXIS2_PLACEMENT_3D ( 'NONE', #23736, #1695, #28319 ) ;
#26158 =( NAMED_UNIT ( * ) SI_UNIT ( $, .STERADIAN. ) SOLID_ANGLE_UNIT ( ) );
#26159 = ORIENTED_EDGE ( 'NONE', *, *, #15574, .T. ) ;
#26160 = VERTEX_POINT ( 'NONE', #17148 ) ;
#26161 = CIRCLE ( 'NONE', #12994, 4.700000000000000178 ) ;
#26162 = CARTESIAN_POINT ( 'NONE',  ( -60.43749999999995026, 1.962990915244749557, -3.400000000000205969 ) ) ;
#26163 = AXIS2_PLACEMENT_3D ( 'NONE', #5514, #15004, #15169 ) ;
#26164 = CARTESIAN_POINT ( 'NONE',  ( 57.03920447585827702, -0.8156862745098039102, 2.468735688885368429 ) ) ;
#26165 = LINE ( 'NONE', #17144, #29312 ) ;
#26166 = DIRECTION ( 'NONE',  ( 1.000000000000000000, 1.047444401652940007E-14, 0.000000000000000000 ) ) ;
#26167 = CARTESIAN_POINT ( 'NONE',  ( 58.75000000000000711, 1.469015551797814290, -1.320082690053157037 ) ) ;
#26168 = EDGE_CURVE ( 'NONE', #18665, #20522, #15011, .T. ) ;
#26170 = DIRECTION ( 'NONE',  ( 1.000000000000000000, 0.000000000000000000, -3.491481338843133355E-15 ) ) ;
#26169 = CARTESIAN_POINT ( 'NONE',  ( -36.92398358572908279, 5.231589534716062140, -1.397536681175157502 ) ) ;
#26171 = CIRCLE ( 'NONE', #22641, 1.949999999999999956 ) ;
#26172 = VECTOR ( 'NONE', #16925, 1000.000000000000000 ) ;
#26173 = CARTESIAN_POINT ( 'NONE',  ( -74.38999999999998636, -2.585162900687033808E-15, 4.707972083073595634E-15 ) ) ;
#26174 = DIRECTION ( 'NONE',  ( 0.000000000000000000, 0.000000000000000000, -1.000000000000000000 ) ) ;
#26175 = DIRECTION ( 'NONE',  ( -0.9993908270190956511, 0.03489949670250089980, 3.491481338843132961E-15 ) ) ;
#26176 = ORIENTED_EDGE ( 'NONE', *, *, #15172, .F. ) ;
#26177 =( BOUNDED_CURVE ( )  B_SPLINE_CURVE ( 2, ( #15584, #1158, #27763, #20195, #29825 ),
 .UNSPECIFIED., .F., .T. ) 
 B_SPLINE_CURVE_WITH_KNOTS ( ( 3, 2, 3 ),
 ( 0.000000000000000000, 0.01851851851851851749, 0.02777777777777778317 ),
 .UNSPECIFIED. ) 
 CURVE ( )  GEOMETRIC_REPRESENTATION_ITEM ( )  RATIONAL_B_SPLINE_CURVE ( ( 1.000000000000000000, 0.8660254037844387076, 1.000000000000000000, 0.9330127018922192983, 0.9330127018922194093 ) ) 
 REPRESENTATION_ITEM ( '' )  );
#26179 = CARTESIAN_POINT ( 'NONE',  ( 56.99368740573074632, 0.8156852809530760195, -2.468736017162952656 ) ) ;
#26178 = VECTOR ( 'NONE', #21882, 1000.000000000000000 ) ;
#26180 = CARTESIAN_POINT ( 'NONE',  ( 53.86842434078439368, 7.562405067244617918, 2.049999999999813305 ) ) ;
#26181 = ORIENTED_EDGE ( 'NONE', *, *, #859, .F. ) ;
#26183 = DIRECTION ( 'NONE',  ( 0.000000000000000000, 0.000000000000000000, 1.000000000000000000 ) ) ;
#26182 = CARTESIAN_POINT ( 'NONE',  ( 48.50000000000354561, -1.426739617988837194, 3.843749999997122746 ) ) ;
#26184 = DIRECTION ( 'NONE',  ( 1.000000000000000000, -0.000000000000000000, -0.000000000000000000 ) ) ;
#26185 = CIRCLE ( 'NONE', #6985, 1.975000000000001865 ) ;
#26186 = EDGE_CURVE ( 'NONE', #6647, #14732, #9564, .T. ) ;
#26187 = ORIENTED_EDGE ( 'NONE', *, *, #15795, .F. ) ;
#26188 = DIRECTION ( 'NONE',  ( 1.000000000000000000, 0.000000000000000000, 0.000000000000000000 ) ) ;
#26189 = CARTESIAN_POINT ( 'NONE',  ( 30.51261366513614703, 7.487866468533194819, 1.424999999999893907 ) ) ;
#26190 = CARTESIAN_POINT ( 'NONE',  ( -59.87499999999995737, -2.944486372867076707, -1.700000000000223332 ) ) ;
#26191 = EDGE_LOOP ( 'NONE', ( #25494, #16101, #15318, #5744, #19808, #15862 ) ) ;
#26192 = ORIENTED_EDGE ( 'NONE', *, *, #28454, .T. ) ;
#26193 = CARTESIAN_POINT ( 'NONE',  ( -59.58615951392652477, 3.226516192400048055, -1.172812774183070283 ) ) ;
#26194 = ORIENTED_EDGE ( 'NONE', *, *, #9789, .F. ) ;
#26195 = DIRECTION ( 'NONE',  ( 1.000000000000000000, 0.000000000000000000, 0.000000000000000000 ) ) ;
#26196 = CARTESIAN_POINT ( 'NONE',  ( -57.32202994616202574, 2.078460969082674747, -3.600000000000194600 ) ) ;
#26197 = ORIENTED_EDGE ( 'NONE', *, *, #2052, .F. ) ;
#26198 = FACE_OUTER_BOUND ( 'NONE', #21019, .T. ) ;
#26199 = DIRECTION ( 'NONE',  ( 0.000000000000000000, 0.000000000000000000, 1.000000000000000000 ) ) ;
#26200 = CARTESIAN_POINT ( 'NONE',  ( 31.50816695980749671, 7.454773700472920872, 2.049999999999889244 ) ) ;
#26201 = ORIENTED_EDGE ( 'NONE', *, *, #21270, .F. ) ;
#26202 = ORIENTED_EDGE ( 'NONE', *, *, #9189, .T. ) ;
#26203 = DIRECTION ( 'NONE',  ( 1.000000000000000000, 3.054025858079668409E-16, -2.042474015755241579E-16 ) ) ;
#26204 = DIRECTION ( 'NONE',  ( 0.9993908270191184107, -0.03489949670185085034, -3.491481338843133355E-15 ) ) ;
#26205 = DIRECTION ( 'NONE',  ( 0.000000000000000000, -1.000000000000000000, -4.336808689942015369E-15 ) ) ;
#26206 = ORIENTED_EDGE ( 'NONE', *, *, #16497, .T. ) ;
#26207 = CARTESIAN_POINT ( 'NONE',  ( -57.22499999999997300, -0.8236752438351979677, 4.016411220566566520 ) ) ;
#26208 = DIRECTION ( 'NONE',  ( 0.000000000000000000, -0.4295302013423027421, 0.9030524935654852259 ) ) ;
#26209 = ADVANCED_FACE ( 'NONE', ( #21907 ), #26794, .T. ) ;
#26210 = CARTESIAN_POINT ( 'NONE',  ( -58.89405989232411542, -2.944486372867071822, -1.700000000000227107 ) ) ;
#26212 = CARTESIAN_POINT ( 'NONE',  ( 52.20711756518984714, -0.7499999999994533262, 1.718465885608440269 ) ) ;
#26211 = CARTESIAN_POINT ( 'NONE',  ( -36.63359589171324870, -2.513248512186274652, 4.788125582312047435 ) ) ;
#26213 = CARTESIAN_POINT ( 'NONE',  ( 51.31757909864145972, 1.004435980686513963, 1.391945786376508343 ) ) ;
#26214 = CARTESIAN_POINT ( 'NONE',  ( 63.50000000000000000, -0.7500000000000000000, -2.238246715074021953 ) ) ;
#26215 = CARTESIAN_POINT ( 'NONE',  ( 48.00000000000002132, -3.908336260473453727, 1.238913909465751972 ) ) ;
#26216 = VERTEX_POINT ( 'NONE', #24556 ) ;
#26217 = CIRCLE ( 'NONE', #7018, 0.2499999999999986955 ) ;
#26218 = AXIS2_PLACEMENT_3D ( 'NONE', #20795, #18409, #10507 ) ;
#26219 = VERTEX_POINT ( 'NONE', #29456 ) ;
#26220 = ADVANCED_FACE ( 'NONE', ( #22051 ), #4891, .T. ) ;
#26221 = CARTESIAN_POINT ( 'NONE',  ( 51.80349172417631110, 1.030408547777236894, -4.190799094670026648 ) ) ;
#26222 = ORIENTED_EDGE ( 'NONE', *, *, #28181, .F. ) ;
#26223 = DIRECTION ( 'NONE',  ( 0.000000000000000000, -1.000000000000000000, -3.491481338843132961E-15 ) ) ;
#26224 = CARTESIAN_POINT ( 'NONE',  ( -55.29792740578360366, -1.073804522883516688, -3.225979517392336238 ) ) ;
#26226 = CARTESIAN_POINT ( 'NONE',  ( -36.11692583559974423, 4.018128194440848233, 3.618665885216990397 ) ) ;
#26225 = DIRECTION ( 'NONE',  ( 0.000000000000000000, 2.168404344971012812E-15, 1.000000000000000000 ) ) ;
#26227 = EDGE_LOOP ( 'NONE', ( #9783, #14961, #8118, #11917 ) ) ;
#26228 = ORIENTED_EDGE ( 'NONE', *, *, #12353, .F. ) ;
#26229 = CARTESIAN_POINT ( 'NONE',  ( 58.75000000000003553, -1.877732920580616804, -0.6121634413826790855 ) ) ;
#26230 = VERTEX_POINT ( 'NONE', #7771 ) ;
#26231 = CARTESIAN_POINT ( 'NONE',  ( 58.75000000000000711, 1.470078920828157498, -1.320078920826817992 ) ) ;
#26232 = ORIENTED_EDGE ( 'NONE', *, *, #6908, .T. ) ;
#26234 = DIRECTION ( 'NONE',  ( 0.000000000000000000, 0.2008964009354162750, -0.9796124928211136229 ) ) ;
#26233 = CARTESIAN_POINT ( 'NONE',  ( 50.41047473690881731, 0.7808213810458778381, 4.027268569371624807 ) ) ;
#26235 = ORIENTED_EDGE ( 'NONE', *, *, #1897, .F. ) ;
#26236 = CYLINDRICAL_SURFACE ( 'NONE', #25771, 4.100000000000000533 ) ;
#26237 = EDGE_CURVE ( 'NONE', #30900, #30820, #30675, .T. ) ;
#26238 = FACE_BOUND ( 'NONE', #4231, .T. ) ;
#26239 = DIRECTION ( 'NONE',  ( 3.491481338843133355E-15, 3.491481338843133355E-15, -1.000000000000000000 ) ) ;
#26240 = CARTESIAN_POINT ( 'NONE',  ( 51.59739104186229497, -1.010292945602101256, -1.272765950230260623 ) ) ;
#26241 = CARTESIAN_POINT ( 'NONE',  ( -56.13452994616205416, -3.117691453623976816, 1.799999999999788436 ) ) ;
#26242 = CARTESIAN_POINT ( 'NONE',  ( -59.18632331196522500, -2.527880932825658178, -0.9441059845029629027 ) ) ;
#26243 = CIRCLE ( 'NONE', #30277, 0.1000000000000000333 ) ;
#26244 = EDGE_CURVE ( 'NONE', #24129, #7345, #7174, .T. ) ;
#26245 = CARTESIAN_POINT ( 'NONE',  ( 22.04321716858595082, 7.679566743993206934, 1.549999999999923217 ) ) ;
#26246 = EDGE_CURVE ( 'NONE', #2667, #11593, #25109, .T. ) ;
#26247 = CARTESIAN_POINT ( 'NONE',  ( 54.41366571437519895, 6.718673005292168376, -2.050000000000189448 ) ) ;
#26248 = EDGE_CURVE ( 'NONE', #21490, #17628, #84, .T. ) ;
#26249 = CARTESIAN_POINT ( 'NONE',  ( -58.23542740578360366, 0.7887156198831916099, -3.845940847736168511 ) ) ;
#26250 = CARTESIAN_POINT ( 'NONE',  ( -55.76905989232411542, 2.190330617366546077E-14, -3.400000000000197975 ) ) ;
#26251 = CIRCLE ( 'NONE', #7058, 0.2000000000000000944 ) ;
#26252 = EDGE_LOOP ( 'NONE', ( #5809, #4456, #994, #15399, #17614, #15601, #8585, #3011, #19511, #16895 ) ) ;
#26253 = DIRECTION ( 'NONE',  ( -0.000000000000000000, -0.000000000000000000, -1.000000000000000000 ) ) ;
#26254 = CARTESIAN_POINT ( 'NONE',  ( 52.98657663771353299, 4.708191849549097086, 1.586975497715994221 ) ) ;
#26255 = CARTESIAN_POINT ( 'NONE',  ( 53.94320358904982271, 6.378589075886260673, -0.8960560664367792638 ) ) ;
#26256 = EDGE_LOOP ( 'NONE', ( #30022, #29480, #22406, #20170 ) ) ;
#26257 = EDGE_CURVE ( 'NONE', #5886, #14413, #10636, .T. ) ;
#26258 = CARTESIAN_POINT ( 'NONE',  ( -36.14504829323105639, -4.698774973472870542, 2.676767126782095385 ) ) ;
#26259 = ORIENTED_EDGE ( 'NONE', *, *, #19292, .F. ) ;
#26260 = CYLINDRICAL_SURFACE ( 'NONE', #9688, 0.2500000000000000000 ) ;
#26262 = CARTESIAN_POINT ( 'NONE',  ( 58.75000000000003553, -1.457266603152898243, 1.320165430233939841 ) ) ;
#26261 = CARTESIAN_POINT ( 'NONE',  ( 51.70000000000001705, -4.079459090034584179, -2.128991905554068254 ) ) ;
#26263 = ORIENTED_EDGE ( 'NONE', *, *, #6137, .F. ) ;
#26264 = VERTEX_POINT ( 'NONE', #2245 ) ;
#26265 = CARTESIAN_POINT ( 'NONE',  ( 58.75000000000000000, 1.972190280208464097, 0.1053114364810050774 ) ) ;
#26266 = AXIS2_PLACEMENT_3D ( 'NONE', #5231, #29598, #5704 ) ;
#26267 = CIRCLE ( 'NONE', #23250, 0.1500000000000001887 ) ;
#26268 = CARTESIAN_POINT ( 'NONE',  ( 51.80000000000001137, -3.908336260473453727, -1.238913909466101027 ) ) ;
#26269 = CARTESIAN_POINT ( 'NONE',  ( 58.73379417893125520, 1.006340787081485999, 1.582215608939591789 ) ) ;
#26270 = ORIENTED_EDGE ( 'NONE', *, *, #10566, .F. ) ;
#26271 = CARTESIAN_POINT ( 'NONE',  ( -60.11042740578358945, -0.7887156198831607457, 3.845940847736174728 ) ) ;
#26272 = CARTESIAN_POINT ( 'NONE',  ( 61.23770293222972327, 0.8897917884438596436, 1.791164585743606041 ) ) ;
#26273 = DIRECTION ( 'NONE',  ( 1.000000000000000000, 0.000000000000000000, 0.000000000000000000 ) ) ;
#26274 = EDGE_CURVE ( 'NONE', #30539, #27301, #19606, .T. ) ;
#26275 = CARTESIAN_POINT ( 'NONE',  ( -35.85663232820584057, 2.199885893005902204, 4.939696249117695892 ) ) ;
#26276 = CARTESIAN_POINT ( 'NONE',  ( 47.00000000000003553, 6.982261990806648555E-14, 4.499999999999873879 ) ) ;
#26277 = DIRECTION ( 'NONE',  ( 0.000000000000000000, -1.000000000000000000, -3.491481338843136511E-15 ) ) ;
#26278 = EDGE_CURVE ( 'NONE', #15739, #20313, #13509, .T. ) ;
#26279 = CARTESIAN_POINT ( 'NONE',  ( -35.85663232820584057, -4.945493884734804446, -1.606888370749739448 ) ) ;
#26280 = ORIENTED_EDGE ( 'NONE', *, *, #5877, .F. ) ;
#26281 = CARTESIAN_POINT ( 'NONE',  ( -57.27900635094606940, -1.737685414808519457, 3.471684241605561994 ) ) ;
#26282 = CARTESIAN_POINT ( 'NONE',  ( -35.85663232820581925, 2.525801270006329702, -4.794550352686303363 ) ) ;
#26283 = EDGE_CURVE ( 'NONE', #8004, #26599, #1886, .T. ) ;
#26284 = CARTESIAN_POINT ( 'NONE',  ( 57.00000000000001421, 0.6999999999999999556, 1.820027472320129736 ) ) ;
#26285 = CARTESIAN_POINT ( 'NONE',  ( 29.88389444396583627, 6.456032137337936128, -1.950000000000103428 ) ) ;
#26286 = EDGE_CURVE ( 'NONE', #29895, #10800, #15537, .T. ) ;
#26287 = AXIS2_PLACEMENT_3D ( 'NONE', #12498, #29296, #22185 ) ;
#26288 = AXIS2_PLACEMENT_3D ( 'NONE', #28640, #31162, #8827 ) ;
#26289 = AXIS2_PLACEMENT_3D ( 'NONE', #24859, #17431, #5710 ) ;
#26291 = CARTESIAN_POINT ( 'NONE',  ( -60.59999999999997300, -2.342723651847746336, 0.9419505778294103848 ) ) ;
#26290 = CARTESIAN_POINT ( 'NONE',  ( -59.64457535546588929, 2.323701065654787623, -1.273936166954758642 ) ) ;
#26293 = AXIS2_PLACEMENT_3D ( 'NONE', #19885, #29516, #7830 ) ;
#26292 = CARTESIAN_POINT ( 'NONE',  ( -62.05955090584385658, -2.675925004799827978, -0.3612845363725897263 ) ) ;
#26295 = CARTESIAN_POINT ( 'NONE',  ( -59.60304182990236654, 2.022940613791669673, 1.711857625294797680 ) ) ;
#26294 = CARTESIAN_POINT ( 'NONE',  ( 48.00000000000002132, -4.003661535119149129, 1.269131321891750375 ) ) ;
#26296 = ORIENTED_EDGE ( 'NONE', *, *, #8479, .F. ) ;
#26297 = CARTESIAN_POINT ( 'NONE',  ( 33.47623932017462778, 1.734723475976807094E-15, 0.000000000000000000 ) ) ;
#26298 = CARTESIAN_POINT ( 'NONE',  ( 51.80000000000001847, -4.131056160354152240, -1.100000000000000089 ) ) ;
#26300 = CARTESIAN_POINT ( 'NONE',  ( -36.56390771145526486, 5.076023720898184877, 1.868859051106935398 ) ) ;
#26299 = CARTESIAN_POINT ( 'NONE',  ( 15.48609859788817467, -2.964363692626676094, -4.273817190665769594 ) ) ;
#26301 = CARTESIAN_POINT ( 'NONE',  ( 15.17256654081411682, -4.804073784580274342, 2.042134692980114963 ) ) ;
#26302 = VERTEX_POINT ( 'NONE', #26639 ) ;
#26303 = VERTEX_POINT ( 'NONE', #4944 ) ;
#26304 = DIRECTION ( 'NONE',  ( 1.000000000000000000, -0.000000000000000000, -1.047444401652940007E-14 ) ) ;
#26305 = AXIS2_PLACEMENT_3D ( 'NONE', #5480, #1042, #27164 ) ;
#26306 = ORIENTED_EDGE ( 'NONE', *, *, #9072, .T. ) ;
#26307 = CARTESIAN_POINT ( 'NONE',  ( 56.95640338720422591, 0.7513613876702617267, -2.489093304807997509 ) ) ;
#26308 = CARTESIAN_POINT ( 'NONE',  ( 58.74664129364603582, 0.5000000000006152856, 1.856789660955970200 ) ) ;
#26309 = EDGE_LOOP ( 'NONE', ( #20714, #25164, #24624, #7011 ) ) ;
#26310 = EDGE_CURVE ( 'NONE', #10286, #24915, #7974, .T. ) ;
#26311 = CARTESIAN_POINT ( 'NONE',  ( -73.90999999999998238, 1.249612330857415632, 0.03112912734226871286 ) ) ;
#26312 = ORIENTED_EDGE ( 'NONE', *, *, #29545, .F. ) ;
#26313 = EDGE_CURVE ( 'NONE', #12164, #20434, #10928, .T. ) ;
#26314 = CARTESIAN_POINT ( 'NONE',  ( 51.80000000000001847, -3.701035844659721352, -1.983438066290037494 ) ) ;
#26315 = ORIENTED_EDGE ( 'NONE', *, *, #6684, .T. ) ;
#26316 =( NAMED_UNIT ( * ) PLANE_ANGLE_UNIT ( ) SI_UNIT ( $, .RADIAN. ) );
#26317 = EDGE_CURVE ( 'NONE', #21148, #22845, #18238, .T. ) ;
#26318 = EDGE_LOOP ( 'NONE', ( #5123, #13308, #22928, #29421, #20129 ) ) ;
#26319 = ORIENTED_EDGE ( 'NONE', *, *, #18783, .T. ) ;
#26320 = AXIS2_PLACEMENT_3D ( 'NONE', #23043, #30154, #8761 ) ;
#26321 = CARTESIAN_POINT ( 'NONE',  ( -55.19702994616203284, -2.078460969082631227, -3.600000000000202593 ) ) ;
#26322 = CARTESIAN_POINT ( 'NONE',  ( 57.05000000000001847, -0.8156862745098041323, 2.468735688885368873 ) ) ;
#26323 = DIRECTION ( 'NONE',  ( 1.000000000000000000, -0.000000000000000000, -1.047444401652940007E-14 ) ) ;
#26324 = DIRECTION ( 'NONE',  ( -1.000000000000000000, 1.219044193948983948E-29, -3.491481338843133355E-15 ) ) ;
#26325 = LINE ( 'NONE', #16834, #23145 ) ;
#26327 = DIRECTION ( 'NONE',  ( 0.000000000000000000, 0.000000000000000000, 1.000000000000000000 ) ) ;
#26326 = PRESENTATION_STYLE_ASSIGNMENT (( #18895 ) ) ;
#26328 =( BOUNDED_CURVE ( )  B_SPLINE_CURVE ( 3, ( #28948, #7256, #16924, #26568 ),
 .UNSPECIFIED., .F., .T. ) 
 B_SPLINE_CURVE_WITH_KNOTS ( ( 4, 4 ),
 ( 4.094114376165668645, 4.828985806059319152 ),
 .UNSPECIFIED. ) 
 CURVE ( )  GEOMETRIC_REPRESENTATION_ITEM ( )  RATIONAL_B_SPLINE_CURVE ( ( 1.000000000000000000, 0.9555010429016485007, 0.9555010429016485007, 1.000000000000000000 ) ) 
 REPRESENTATION_ITEM ( '' )  );
#26329 = CARTESIAN_POINT ( 'NONE',  ( -62.14999999999998437, 2.749147127886321318, 0.06848408015298346196 ) ) ;
#26330 = DIRECTION ( 'NONE',  ( 0.000000000000000000, -1.000000000000000000, -0.000000000000000000 ) ) ;
#26331 = CARTESIAN_POINT ( 'NONE',  ( 54.40000000000001990, -0.2842225609755594795, -1.577752156565102655E-15 ) ) ;
#26332 = EDGE_LOOP ( 'NONE', ( #11777, #3300, #4244, #14298 ) ) ;
#26333 = DIRECTION ( 'NONE',  ( -1.000000000000000000, -3.053848253006669023E-16, 2.042510438544995415E-16 ) ) ;
#26334 = CARTESIAN_POINT ( 'NONE',  ( 54.05511024441276646, 7.179753009059693269, 2.049999999999811529 ) ) ;
#26336 = CARTESIAN_POINT ( 'NONE',  ( 48.41300975153458097, -1.088846059295756508, -3.899771020632008423 ) ) ;
#26335 = CARTESIAN_POINT ( 'NONE',  ( 58.65000000000003411, -1.253243060178072188, 1.394635017527513510 ) ) ;
#26337 = CARTESIAN_POINT ( 'NONE',  ( 54.28771311682444178, 6.706930398806282945, -2.050000000000190781 ) ) ;
#26338 = CYLINDRICAL_SURFACE ( 'NONE', #299, 2.000000000000000000 ) ;
#26339 = VECTOR ( 'NONE', #26961, 1000.000000000000000 ) ;
#26340 = ORIENTED_EDGE ( 'NONE', *, *, #26313, .F. ) ;
#26341 = CARTESIAN_POINT ( 'NONE',  ( 51.69060524973902204, 0.7995873297242745981, 1.427997211818381684 ) ) ;
#26342 = CARTESIAN_POINT ( 'NONE',  ( 50.80000000000002558, -4.319730106884873244, 1.256953381662059277 ) ) ;
#26343 = CARTESIAN_POINT ( 'NONE',  ( -59.31249999999997868, -1.962990915244731793, 3.399999999999781419 ) ) ;
#26344 = ORIENTED_EDGE ( 'NONE', *, *, #15742, .T. ) ;
#26345 = ORIENTED_EDGE ( 'NONE', *, *, #16160, .T. ) ;
#26346 = EDGE_CURVE ( 'NONE', #14356, #22384, #13284, .T. ) ;
#26347 = CYLINDRICAL_SURFACE ( 'NONE', #27042, 1.000000000000000000 ) ;
#26348 = VERTEX_POINT ( 'NONE', #25343 ) ;
#26349 = EDGE_CURVE ( 'NONE', #16856, #7637, #25606, .T. ) ;
#26350 = DIRECTION ( 'NONE',  ( -1.000000000000000000, -0.000000000000000000, -0.000000000000000000 ) ) ;
#26351 = CARTESIAN_POINT ( 'NONE',  ( -56.50952994616203995, 3.117691453623994580, -1.800000000000187006 ) ) ;
#26352 = EDGE_LOOP ( 'NONE', ( #20786, #13302, #18005, #25747 ) ) ;
#26353 = CARTESIAN_POINT ( 'NONE',  ( 22.07280086217093285, 8.086143481909154218, -1.950000000000076339 ) ) ;
#26354 = FACE_OUTER_BOUND ( 'NONE', #13579, .T. ) ;
#26355 = CARTESIAN_POINT ( 'NONE',  ( 33.98208436257321097, 8.188484708538934953, 1.949999999999879385 ) ) ;
#26356 = ORIENTED_EDGE ( 'NONE', *, *, #4617, .F. ) ;
#26357 = CARTESIAN_POINT ( 'NONE',  ( -58.62499999999997158, -3.673546848079170424, -0.7533615035078236044 ) ) ;
#26358 = FACE_OUTER_BOUND ( 'NONE', #5383, .T. ) ;
#26359 = CARTESIAN_POINT ( 'NONE',  ( -44.49999999999999289, 0.000000000000000000, 0.000000000000000000 ) ) ;
#26360 = ORIENTED_EDGE ( 'NONE', *, *, #12620, .F. ) ;
#26361 = DIRECTION ( 'NONE',  ( -1.000000000000000000, 0.000000000000000000, 1.047444401652940007E-14 ) ) ;
#26362 = CARTESIAN_POINT ( 'NONE',  ( 56.97542489291938494, 0.7477441023849552559, 1.746698826563745977 ) ) ;
#26363 = ADVANCED_FACE ( 'NONE', ( #3508 ), #8244, .T. ) ;
#26364 =( BOUNDED_SURFACE ( )  B_SPLINE_SURFACE ( 3, 2, ( 
 ( #12910, #8324, #17998 ),
 ( #10388, #8179, #25273 ),
 ( #25110, #20235, #20542 ),
 ( #30176, #27009, #5316 ),
 ( #24647, #19906, #17846 ),
 ( #29534, #2961, #22292 ),
 ( #27483, #17531, #5801 ),
 ( #27181, #5492, #15144 ) ),
 .UNSPECIFIED., .F., .F., .T. ) 
 B_SPLINE_SURFACE_WITH_KNOTS ( ( 4, 2, 2, 4 ),
 ( 3, 3 ),
 ( 0.001762834131042892915, 0.001945267826973966826, 0.002127701522905040520, 0.002492568914767187907 ),
 ( 0.000000000000000000, 1.000000000000000000 ),
 .UNSPECIFIED. ) 
 GEOMETRIC_REPRESENTATION_ITEM ( )  RATIONAL_B_SPLINE_SURFACE ( (
 ( 1.000000000000000000, 0.8699658093904940603, 1.000000000000000000),
 ( 1.000000000000000000, 0.8851796357839156748, 1.000000000000000000),
 ( 1.000000000000000000, 0.8977447492167196508, 1.000000000000000000),
 ( 1.000000000000000000, 0.9127836411835481556, 1.000000000000000000),
 ( 1.000000000000000000, 0.9151168517135812586, 1.000000000000000000),
 ( 1.000000000000000000, 0.9045976586032163924, 1.000000000000000000),
 ( 1.000000000000000000, 0.8745315534097299892, 1.000000000000000000),
 ( 1.000000000000000000, 0.8388746406931726352, 1.000000000000000000) ) ) 
 REPRESENTATION_ITEM ( '' )  SURFACE ( )  );
#26365 = CARTESIAN_POINT ( 'NONE',  ( 58.75000000000000711, 1.470078920828144620, -1.470078920826818125 ) ) ;
#26367 = DIRECTION ( 'NONE',  ( 0.000000000000000000, 0.000000000000000000, 1.000000000000000000 ) ) ;
#26366 = FACE_OUTER_BOUND ( 'NONE', #13096, .T. ) ;
#26368 = CARTESIAN_POINT ( 'NONE',  ( 51.70000000000001705, -4.259946800035238290, 0.9999999999999995559 ) ) ;
#26369 = CARTESIAN_POINT ( 'NONE',  ( 47.04572677324562591, -4.276948333784439171, 0.9210526315789451246 ) ) ;
#26370 = DIRECTION ( 'NONE',  ( 1.000000000000000000, 1.047444401652940007E-14, 0.000000000000000000 ) ) ;
#26371 = PRODUCT_DEFINITION ( 'UNKNOWN', '', #4040, #27522 ) ;
#26372 = EDGE_LOOP ( 'NONE', ( #25220, #29377, #21586, #20474 ) ) ;
#26373 = ORIENTED_EDGE ( 'NONE', *, *, #5551, .T. ) ;
#26374 = AXIS2_PLACEMENT_3D ( 'NONE', #13214, #13679, #11012 ) ;
#26375 = CARTESIAN_POINT ( 'NONE',  ( 51.12687253673779253, 0.9194130538826106314, 1.491219977510798156 ) ) ;
#26376 = ORIENTED_EDGE ( 'NONE', *, *, #31282, .T. ) ;
#26377 = FACE_OUTER_BOUND ( 'NONE', #16226, .T. ) ;
#26378 = CARTESIAN_POINT ( 'NONE',  ( -55.04792740578361077, 3.330682475591790315, 0.6830477631804101613 ) ) ;
#26380 = FACE_OUTER_BOUND ( 'NONE', #18484, .T. ) ;
#26379 = FACE_OUTER_BOUND ( 'NONE', #7643, .T. ) ;
#26381 = ORIENTED_EDGE ( 'NONE', *, *, #8115, .T. ) ;
#26382 = ORIENTED_EDGE ( 'NONE', *, *, #7473, .T. ) ;
#26383 = CARTESIAN_POINT ( 'NONE',  ( 61.00000000000000711, 0.8111533433300022189, -1.409596402461000597 ) ) ;
#26384 = ORIENTED_EDGE ( 'NONE', *, *, #24665, .F. ) ;
#26385 = EDGE_CURVE ( 'NONE', #13383, #18442, #25798, .T. ) ;
#26386 = CARTESIAN_POINT ( 'NONE',  ( -74.38999999999998636, 1.249612330857415410, 0.03112912734226870939 ) ) ;
#26387 = ORIENTED_EDGE ( 'NONE', *, *, #27559, .T. ) ;
#26388 = CARTESIAN_POINT ( 'NONE',  ( 50.40000000000001279, 0.6462379109120992560, 4.048750000000022276 ) ) ;
#26389 = APPLICATION_CONTEXT ( 'automotive_design' ) ;
#26390 = ORIENTED_EDGE ( 'NONE', *, *, #2490, .T. ) ;
#26391 = CARTESIAN_POINT ( 'NONE',  ( 57.05000000000001137, -0.7500000000000002220, 1.746008434843742796 ) ) ;
#26392 = CARTESIAN_POINT ( 'NONE',  ( 57.00221072626734298, 0.7147032416868923654, 1.808443027029684291 ) ) ;
#26393 = DIRECTION ( 'NONE',  ( -3.002035892788117459E-16, 0.9996898646859344595, 0.02490330187381124133 ) ) ;
#26394 = CIRCLE ( 'NONE', #13217, 0.1500000000000000777 ) ;
#26395 = CARTESIAN_POINT ( 'NONE',  ( -44.49999999999997868, -1.499999999999999556, -4.029888335921975262 ) ) ;
#26396 = CARTESIAN_POINT ( 'NONE',  ( -61.07202994616202574, 2.078460969082674747, -3.600000000000208367 ) ) ;
#26397 = FACE_OUTER_BOUND ( 'NONE', #13121, .T. ) ;
#26398 = AXIS2_PLACEMENT_3D ( 'NONE', #8085, #17752, #15352 ) ;
#26399 = CIRCLE ( 'NONE', #7196, 1.000000000000000000 ) ;
#26400 = ADVANCED_FACE ( 'NONE', ( #12675 ), #12995, .T. ) ;
#26401 = CARTESIAN_POINT ( 'NONE',  ( 58.66054497607991891, 0.5000000000007229772, 1.807104036850091910 ) ) ;
#26402 = CARTESIAN_POINT ( 'NONE',  ( -56.28335481156722864, 3.238593381231848145, 2.874284765127022467 ) ) ;
#26403 = CARTESIAN_POINT ( 'NONE',  ( 52.20711756518983293, 0.5000000000005468959, -1.718465885608440269 ) ) ;
#26404 = ORIENTED_EDGE ( 'NONE', *, *, #30575, .F. ) ;
#26405 = DIRECTION ( 'NONE',  ( -1.000000000000000000, -3.053848253006669023E-16, 2.042510438544995415E-16 ) ) ;
#26406 = ORIENTED_EDGE ( 'NONE', *, *, #26820, .T. ) ;
#26407 = DIRECTION ( 'NONE',  ( 0.000000000000000000, 0.000000000000000000, 1.000000000000000000 ) ) ;
#26408 = DIRECTION ( 'NONE',  ( 2.470865626055588132E-12, -0.5454670984319637261, -0.8381322357052104488 ) ) ;
#26409 = CARTESIAN_POINT ( 'NONE',  ( 54.02156981857547891, 6.375678713436270684, 1.975347020395713526 ) ) ;
#26410 = ORIENTED_EDGE ( 'NONE', *, *, #18730, .T. ) ;
#26411 = DIRECTION ( 'NONE',  ( 1.057355261547768637E-14, 0.000000000000000000, 1.000000000000000000 ) ) ;
#26412 = ORIENTED_EDGE ( 'NONE', *, *, #5998, .T. ) ;
#26413 = FACE_OUTER_BOUND ( 'NONE', #20945, .T. ) ;
#26415 = CARTESIAN_POINT ( 'NONE',  ( 58.65838214097802705, -1.301971553119757763, 1.349359547237667600 ) ) ;
#26414 = CARTESIAN_POINT ( 'NONE',  ( 58.75000000000000711, 1.065927491745594757, -1.652350234724163203 ) ) ;
#26416 = VERTEX_POINT ( 'NONE', #5878 ) ;
#26417 = CARTESIAN_POINT ( 'NONE',  ( 51.25000000000001421, 5.368152558471320595E-13, 3.111507638930570854E-58 ) ) ;
#26418 = ADVANCED_FACE ( 'NONE', ( #22357 ), #15696, .F. ) ;
#26419 = DIRECTION ( 'NONE',  ( -1.000000000000000000, -0.000000000000000000, 3.491481338843133355E-15 ) ) ;
#26421 = CARTESIAN_POINT ( 'NONE',  ( 58.75000000694006275, 0.9428687169911466048, 1.682988785001243492 ) ) ;
#26420 = FACE_OUTER_BOUND ( 'NONE', #16778, .T. ) ;
#26422 = ORIENTED_EDGE ( 'NONE', *, *, #26567, .F. ) ;
#26423 = CARTESIAN_POINT ( 'NONE',  ( -54.49999999999997868, 3.673546848079181082, 0.7533615035078053968 ) ) ;
#26424 = CARTESIAN_POINT ( 'NONE',  ( 61.23793632918098240, 0.8908246368668226722, 1.774550402280007155 ) ) ;
#26425 = CARTESIAN_POINT ( 'NONE',  ( 68.00000000000001421, 1.401298464324817071E-42, -7.122621931239992550E-13 ) ) ;
#26426 = EDGE_CURVE ( 'NONE', #29340, #9758, #24950, .T. ) ;
#26427 = CARTESIAN_POINT ( 'NONE',  ( 15.03925126672132961, -4.018128179617538542, -3.618665901676658248 ) ) ;
#26428 = ITEM_DEFINED_TRANSFORMATION ( 'NONE', 'NONE', #20727,  #9018 ) ;
#26429 = CARTESIAN_POINT ( 'NONE',  ( -54.49999999999997868, 0.000000000000000000, 0.000000000000000000 ) ) ;
#26430 = CARTESIAN_POINT ( 'NONE',  ( 52.15659567665551322, -0.4999999999994547695, 1.807104036850121886 ) ) ;
#26431 = B_SPLINE_CURVE_WITH_KNOTS ( 'NONE', 3,
 ( #27336, #17364, #15301, #20809, #12759, #30440, #10987, #22437, #3853, #732, #24946, #3692, #18431, #13502, #5318, #20667, #10239, #23192 ),
 .UNSPECIFIED., .F., .F.,
 ( 4, 2, 2, 2, 2, 2, 2, 2, 4 ),
 ( 1.986428814944108226E-17, 0.0007541749550748564745, 0.001508349910149693216, 0.002262524865224529742, 0.003016699820299365616, 0.003770874775374201925, 0.004525049730449038667, 0.005279224685523875409, 0.006033399640598711283 ),
 .UNSPECIFIED. ) ;
#26432 = DIRECTION ( 'NONE',  ( -1.000000000000000000, -0.000000000000000000, 3.491481338843133355E-15 ) ) ;
#26433 = ORIENTED_EDGE ( 'NONE', *, *, #27243, .T. ) ;
#26434 = EDGE_CURVE ( 'NONE', #4172, #16714, #10452, .T. ) ;
#26435 = DIRECTION ( 'NONE',  ( -3.696862594069201137E-15, -0.9356455129756980904, -0.3529411764705883137 ) ) ;
#26436 = CARTESIAN_POINT ( 'NONE',  ( 15.22780280894162708, -3.779372851356274765, 3.883777284340669045 ) ) ;
#26437 = CARTESIAN_POINT ( 'NONE',  ( -71.49999999999998579, 0.9743475445367603127, -4.751120590182400960 ) ) ;
#26438 = CARTESIAN_POINT ( 'NONE',  ( 22.56915537023571261, 6.668482724649285487, -1.950000000000079226 ) ) ;
#26439 = DIRECTION ( 'NONE',  ( -1.000000000000000000, -1.047444401652940007E-14, -0.000000000000000000 ) ) ;
#26441 = DIRECTION ( 'NONE',  ( 0.000000000000000000, 0.4531102586343168093, 0.8914544820238118339 ) ) ;
#26440 = DIRECTION ( 'NONE',  ( -1.000000000000000000, -2.586136946169074517E-16, 0.000000000000000000 ) ) ;
#26442 = EDGE_CURVE ( 'NONE', #13516, #23278, #5569, .T. ) ;
#26443 = LINE ( 'NONE', #1911, #19055 ) ;
#26445 = CARTESIAN_POINT ( 'NONE',  ( 69.00000000000001421, 1.401298464324817071E-42, -7.227366371405287181E-13 ) ) ;
#26444 = CARTESIAN_POINT ( 'NONE',  ( 15.03925126672132961, 7.778712668717615929E-15, -5.200000000000000178 ) ) ;
#26446 = ORIENTED_EDGE ( 'NONE', *, *, #17811, .F. ) ;
#26447 = DIRECTION ( 'NONE',  ( 0.000000000000000000, 0.000000000000000000, -1.000000000000000000 ) ) ;
#26448 = CARTESIAN_POINT ( 'NONE',  ( 50.50000000000002132, -0.7901969350669644232, 4.025772098418840095 ) ) ;
#26449 = AXIS2_PLACEMENT_3D ( 'NONE', #13299, #18251, #20633 ) ;
#26451 = CARTESIAN_POINT ( 'NONE',  ( -35.85663232820581925, 5.340403872473301838, 0.9205822173396537300 ) ) ;
#26450 = CARTESIAN_POINT ( 'NONE',  ( 58.65000000000001990, 6.143261415694495821E-13, 3.111507638930570854E-58 ) ) ;
#26452 = CARTESIAN_POINT ( 'NONE',  ( 15.30042582489636160, -4.683225673667250177, 2.703237737472941493 ) ) ;
#26453 = ORIENTED_EDGE ( 'NONE', *, *, #16432, .F. ) ;
#26454 = ORIENTED_EDGE ( 'NONE', *, *, #16574, .T. ) ;
#26455 = CARTESIAN_POINT ( 'NONE',  ( 51.32256723588026404, -1.004590634318890174, -1.391663617071707826 ) ) ;
#26456 = EDGE_CURVE ( 'NONE', #10573, #12424, #9351, .T. ) ;
#26457 = ORIENTED_EDGE ( 'NONE', *, *, #19429, .F. ) ;
#26458 = CYLINDRICAL_SURFACE ( 'NONE', #4898, 0.2500000000000000555 ) ;
#26459 = ADVANCED_FACE ( 'NONE', ( #25488 ), #18859, .F. ) ;
#26460 = DIRECTION ( 'NONE',  ( 0.000000000000000000, 0.9996898646859344595, 0.02490330187381124133 ) ) ;
#26461 = EDGE_LOOP ( 'NONE', ( #15266, #12128, #13011, #29058, #25216 ) ) ;
#26462 = EDGE_CURVE ( 'NONE', #16343, #10792, #5353, .T. ) ;
#26463 = ORIENTED_EDGE ( 'NONE', *, *, #17141, .T. ) ;
#26464 = ORIENTED_EDGE ( 'NONE', *, *, #27816, .T. ) ;
#26465 =( LENGTH_UNIT ( ) NAMED_UNIT ( * ) SI_UNIT ( .MILLI., .METRE. ) );
#26466 = ORIENTED_EDGE ( 'NONE', *, *, #23564, .F. ) ;
#26467 = ORIENTED_EDGE ( 'NONE', *, *, #26146, .F. ) ;
#26468 = CARTESIAN_POINT ( 'NONE',  ( -55.32202994616205416, -4.156921938165296204, -2.115361882398036228E-13 ) ) ;
#26469 = DIRECTION ( 'NONE',  ( 2.581436205204234499E-16, -0.9796124928211140670, -0.2008964009354146651 ) ) ;
#26470 = AXIS2_PLACEMENT_3D ( 'NONE', #26297, #4598, #26447 ) ;
#26471 = CARTESIAN_POINT ( 'NONE',  ( -54.49454330418567594, -1.526701536696946082, 3.317245250669463630 ) ) ;
#26472 = CIRCLE ( 'NONE', #5221, 2.000000000000000000 ) ;
#26473 = CARTESIAN_POINT ( 'NONE',  ( -61.13542439536082895, -2.534004151299444896, -0.9379212110198712482 ) ) ;
#26475 = CARTESIAN_POINT ( 'NONE',  ( -61.34999999999997300, -2.528827883897363904, -0.7921676171260561006 ) ) ;
#26474 = CARTESIAN_POINT ( 'NONE',  ( -59.39247302616080049, -3.117158037005095750, 1.361260878598222757 ) ) ;
#26476 = EDGE_CURVE ( 'NONE', #27301, #30539, #23644, .T. ) ;
#26477 = CARTESIAN_POINT ( 'NONE',  ( 47.01039059310604529, -4.157292525004591788, 1.048498855808312813 ) ) ;
#26478 = CARTESIAN_POINT ( 'NONE',  ( 58.75000000000000711, 1.320082690054482866, -1.469015551796560182 ) ) ;
#26480 = CARTESIAN_POINT ( 'NONE',  ( -60.44999999999996021, 1.979096954302128589E-15, 6.602471875703214707E-16 ) ) ;
#26479 = DIRECTION ( 'NONE',  ( 0.000000000000000000, 0.000000000000000000, 1.000000000000000000 ) ) ;
#26481 = ORIENTED_EDGE ( 'NONE', *, *, #10430, .F. ) ;
#26482 = DIRECTION ( 'NONE',  ( -8.860386339788720432E-15, 0.8459051693633012903, 0.5333333333333336590 ) ) ;
#26483 = EDGE_CURVE ( 'NONE', #865, #171, #11997, .T. ) ;
#26484 = CARTESIAN_POINT ( 'NONE',  ( -67.34999999999998010, -4.352537305703398686E-16, 3.270044734337918230E-15 ) ) ;
#26485 = LINE ( 'NONE', #26803, #22100 ) ;
#26486 = CARTESIAN_POINT ( 'NONE',  ( 54.38834443889974324, 6.716312293568780234, -2.020139939762307879 ) ) ;
#26487 = ORIENTED_EDGE ( 'NONE', *, *, #13871, .F. ) ;
#26488 = CARTESIAN_POINT ( 'NONE',  ( -59.69999999999997442, 3.400000000000007905, -2.001823990013003858E-13 ) ) ;
#26489 = EDGE_LOOP ( 'NONE', ( #5127, #2558, #20509, #11028 ) ) ;
#26490 = VECTOR ( 'NONE', #8714, 1000.000000000000000 ) ;
#26491 = DIRECTION ( 'NONE',  ( 1.000000000000000000, 1.047444401652940007E-14, 0.000000000000000000 ) ) ;
#26492 = CARTESIAN_POINT ( 'NONE',  ( -56.32202994616206126, 2.078460969082646770, 3.599999999999807354 ) ) ;
#26493 = EDGE_LOOP ( 'NONE', ( #23920, #531, #10745, #2173 ) ) ;
#26494 = ORIENTED_EDGE ( 'NONE', *, *, #14228, .F. ) ;
#26495 = CARTESIAN_POINT ( 'NONE',  ( 15.81621483022873420, 4.847650360853553053, 2.396424556482827928 ) ) ;
#26496 = ORIENTED_EDGE ( 'NONE', *, *, #5706, .F. ) ;
#26497 = CARTESIAN_POINT ( 'NONE',  ( 50.35762544161294585, 8.151359338959888845, -1.950000000000174927 ) ) ;
#26498 = CARTESIAN_POINT ( 'NONE',  ( -56.44702994616204705, 4.156921938165313080, -1.854183217685626176E-13 ) ) ;
#26499 = ORIENTED_EDGE ( 'NONE', *, *, #16917, .T. ) ;
#26500 = CARTESIAN_POINT ( 'NONE',  ( 19.23646557533807666, 5.338914163118007039, 6.538284140784940128E-16 ) ) ;
#26501 = CARTESIAN_POINT ( 'NONE',  ( -59.36488781976483864, -2.508594352967794983, -1.045061501994807296 ) ) ;
#26502 = CIRCLE ( 'NONE', #5271, 0.1500000000000003830 ) ;
#26503 = VERTEX_POINT ( 'NONE', #15991 ) ;
#26504 = DIRECTION ( 'NONE',  ( 0.000000000000000000, -1.000000000000000000, 0.000000000000000000 ) ) ;
#26505 =( BOUNDED_CURVE ( )  B_SPLINE_CURVE ( 2, ( #12743, #15284, #10693, #22421, #12896, #887, #17512, #22746, #3575 ),
 .UNSPECIFIED., .F., .T. ) 
 B_SPLINE_CURVE_WITH_KNOTS ( ( 3, 2, 2, 2, 3 ),
 ( 0.6388888888888889506, 0.6481481481481481399, 0.6666666666666666297, 0.6851851851851852304, 0.6944444444444445308 ),
 .UNSPECIFIED. ) 
 CURVE ( )  GEOMETRIC_REPRESENTATION_ITEM ( )  RATIONAL_B_SPLINE_CURVE ( ( 0.9330127018922194093, 0.9330127018922197424, 1.000000000000000000, 0.8660254037844387076, 1.000000000000000000, 0.8660254037844387076, 1.000000000000000000, 0.9330127018922189652, 0.9330127018922194093 ) ) 
 REPRESENTATION_ITEM ( '' )  );
#26506 = DIRECTION ( 'NONE',  ( -1.000000000000000000, 1.219044193948983948E-29, -3.491481338843133355E-15 ) ) ;
#26507 = CARTESIAN_POINT ( 'NONE',  ( 50.55256015243838164, 0.05146993878642957404, -0.7900664826958426756 ) ) ;
#26508 = ORIENTED_EDGE ( 'NONE', *, *, #18373, .F. ) ;
#26509 = DIRECTION ( 'NONE',  ( -1.000000000000000000, -3.053848253006669023E-16, 2.042510438544995415E-16 ) ) ;
#26510 = CARTESIAN_POINT ( 'NONE',  ( 56.96931127949304141, 0.7396072067343685275, 1.750137474527811321 ) ) ;
#26511 = AXIS2_PLACEMENT_3D ( 'NONE', #22790, #22930, #15322 ) ;
#26512 = CARTESIAN_POINT ( 'NONE',  ( 58.65000000000004121, -1.782657835994225781, -0.5811678240974800236 ) ) ;
#26513 = CIRCLE ( 'NONE', #13858, 4.100000000000022737 ) ;
#26514 = EDGE_CURVE ( 'NONE', #9168, #23979, #9448, .T. ) ;
#26515 = DIRECTION ( 'NONE',  ( 0.000000000000000000, 0.9996898646859344595, 0.02490330187381124480 ) ) ;
#26516 = EDGE_CURVE ( 'NONE', #1141, #25117, #15836, .T. ) ;
#26517 = DIRECTION ( 'NONE',  ( 1.000000000000000000, -0.000000000000000000, -1.047444401652940007E-14 ) ) ;
#26518 = CARTESIAN_POINT ( 'NONE',  ( 61.24473505568558096, -0.9276313280769659109, -1.700547749640250350 ) ) ;
#26519 = EDGE_CURVE ( 'NONE', #21490, #29648, #26825, .T. ) ;
#26520 = CIRCLE ( 'NONE', #10334, 2.374999999999998668 ) ;
#26521 = ORIENTED_EDGE ( 'NONE', *, *, #15831, .F. ) ;
#26522 = EDGE_LOOP ( 'NONE', ( #9291, #19857, #17163, #13730, #12644, #20416 ) ) ;
#26523 = CARTESIAN_POINT ( 'NONE',  ( 51.90000000000001279, 1.029992063861229212E-15, -4.375000000000002665 ) ) ;
#26524 = EDGE_LOOP ( 'NONE', ( #16710, #11629, #18152, #24426 ) ) ;
#26525 = DIRECTION ( 'NONE',  ( 1.000000000000000000, -0.000000000000000000, -0.000000000000000000 ) ) ;
#26526 = CARTESIAN_POINT ( 'NONE',  ( -59.90835481156723574, -0.8699069336946634312, 4.241846523238430144 ) ) ;
#26528 = CARTESIAN_POINT ( 'NONE',  ( 51.25000000000001421, 0.7500000000005367928, 1.718465885608440269 ) ) ;
#26527 = CARTESIAN_POINT ( 'NONE',  ( 61.25000000000002132, 6.415596960124259844E-13, 3.111507638930570854E-58 ) ) ;
#26529 = VERTEX_POINT ( 'NONE', #28350 ) ;
#26530 = CARTESIAN_POINT ( 'NONE',  ( 22.08713154258123978, 7.931348155120199195, -2.050000000000076650 ) ) ;
#26531 = ORIENTED_EDGE ( 'NONE', *, *, #14630, .T. ) ;
#26532 = EDGE_CURVE ( 'NONE', #26416, #1831, #25961, .T. ) ;
#26533 = CARTESIAN_POINT ( 'NONE',  ( 51.70000000000000995, 4.174380580618773706, -1.932497546739578631 ) ) ;
#26534 = ORIENTED_EDGE ( 'NONE', *, *, #9489, .T. ) ;
#26535 = CARTESIAN_POINT ( 'NONE',  ( 50.34896831693479413, 1.383117500627097263, 3.859810431918047957 ) ) ;
#26536 = ORIENTED_EDGE ( 'NONE', *, *, #22961, .T. ) ;
#26537 = CIRCLE ( 'NONE', #11357, 0.04999999999999988481 ) ;
#26538 = LINE ( 'NONE', #24015, #1538 ) ;
#26539 = CARTESIAN_POINT ( 'NONE',  ( 57.00000000000001421, 0.7049799947465446026, 1.816196764953787124 ) ) ;
#26540 = B_SPLINE_CURVE_WITH_KNOTS ( 'NONE', 3,
 ( #13968, #21301, #27421, #22520, #514, #27103, #14909, #10171, #24424, #2891, #2735, #10321, #12541, #29470, #29796, #3196, #661, #7784, #19539, #8111, #19840, #5585 ),
 .UNSPECIFIED., .F., .F.,
 ( 4, 3, 3, 3, 3, 3, 3, 4 ),
 ( 0.000000000000000000, 1.393664602030251122E-05, 2.794505907987546679E-05, 4.337356477558444669E-05, 6.134619026776088897E-05, 8.251722506675484789E-05, 8.560979848730156062E-05, 8.708485877085708770E-05 ),
 .UNSPECIFIED. ) ;
#26541 = CARTESIAN_POINT ( 'NONE',  ( 56.95000000000001705, 0.6820512820512815155, -1.773360101234998210 ) ) ;
#26542 = AXIS2_PLACEMENT_3D ( 'NONE', #9217, #18877, #26460 ) ;
#26543 = PRODUCT_RELATED_PRODUCT_CATEGORY ( 'part', '', ( #23518 ) ) ;
#26544 = CARTESIAN_POINT ( 'NONE',  ( -55.20655989232412963, -3.925981830489445379, -2.103125626221096647E-13 ) ) ;
#26545 = CARTESIAN_POINT ( 'NONE',  ( -59.19151862111560547, -2.538026038378716542, -0.9449667484854825661 ) ) ;
#26546 = CARTESIAN_POINT ( 'NONE',  ( -58.74999999999997158, 2.944486372867083368, 1.699999999999819655 ) ) ;
#26547 = CARTESIAN_POINT ( 'NONE',  ( -56.22085481156723574, 1.184343223768591358, 3.558065644182726750 ) ) ;
#26548 = CIRCLE ( 'NONE', #6337, 1.975000000000001865 ) ;
#26549 = FACE_OUTER_BOUND ( 'NONE', #22915, .T. ) ;
#26550 = EDGE_CURVE ( 'NONE', #13819, #11624, #5440, .T. ) ;
#26551 = DIRECTION ( 'NONE',  ( 0.000000000000000000, 0.000000000000000000, 1.000000000000000000 ) ) ;
#26552 = CIRCLE ( 'NONE', #18978, 0.1499999999999998557 ) ;
#26553 = ORIENTED_EDGE ( 'NONE', *, *, #2325, .T. ) ;
#26554 = FACE_OUTER_BOUND ( 'NONE', #31159, .T. ) ;
#26555 = CARTESIAN_POINT ( 'NONE',  ( 15.03925126672133139, -4.383220986679487119, -0.4611378927914498438 ) ) ;
#26556 = CARTESIAN_POINT ( 'NONE',  ( 53.81464057712624793, 5.799094425976102585, -1.402257306246839752 ) ) ;
#26557 = VERTEX_POINT ( 'NONE', #8853 ) ;
#26558 = CARTESIAN_POINT ( 'NONE',  ( 48.40000000000001990, 0.6304760106459518232, 3.950000000000022826 ) ) ;
#26559 = ORIENTED_EDGE ( 'NONE', *, *, #6765, .F. ) ;
#26560 = AXIS2_PLACEMENT_3D ( 'NONE', #31182, #19322, #11712 ) ;
#26561 = CARTESIAN_POINT ( 'NONE',  ( 15.74652664997117490, -0.2088129849845545005, -5.405094643512597941 ) ) ;
#26563 = CARTESIAN_POINT ( 'NONE',  ( -61.57738852934189566, -2.654103483775546390, -0.5064680332891128289 ) ) ;
#26562 = DIRECTION ( 'NONE',  ( 0.000000000000000000, 0.000000000000000000, 1.000000000000000000 ) ) ;
#26564 = ORIENTED_EDGE ( 'NONE', *, *, #8165, .F. ) ;
#26565 = B_SPLINE_CURVE_WITH_KNOTS ( 'NONE', 3,
 ( #1171, #29837, #874, #10533, #10826, #8149, #17337, #29985, #5290, #12577, #5622, #20036, #7678 ),
 .UNSPECIFIED., .F., .F.,
 ( 4, 3, 3, 3, 4 ),
 ( -2.000024084956990982E-06, 0.000000000000000000, 4.241049103993853043E-05, 9.571654392116296867E-05, 0.0001361917980506076374 ),
 .UNSPECIFIED. ) ;
#26566 = LINE ( 'NONE', #28947, #20450 ) ;
#26567 = EDGE_CURVE ( 'NONE', #1256, #22240, #872, .T. ) ;
#26568 = CARTESIAN_POINT ( 'NONE',  ( 51.25000000000001421, 1.100000000000534994, -1.001327244211404732 ) ) ;
#26570 = CARTESIAN_POINT ( 'NONE',  ( -59.69313819382897179, 2.416215365816545724, -1.234576943822310424 ) ) ;
#26569 = LINE ( 'NONE', #12173, #4431 ) ;
#26571 = ORIENTED_EDGE ( 'NONE', *, *, #15081, .T. ) ;
#26572 = CARTESIAN_POINT ( 'NONE',  ( -58.62499999999997158, -3.673546848079174421, -0.7533615035078059519 ) ) ;
#26573 = CARTESIAN_POINT ( 'NONE',  ( -57.68749999999996447, 0.7533615035078071731, -3.673546848079177085 ) ) ;
#26574 = DIRECTION ( 'NONE',  ( 0.000000000000000000, -0.4295302013422799270, -0.9030524935654961061 ) ) ;
#26575 = AXIS2_PLACEMENT_3D ( 'NONE', #7242, #17222, #26551 ) ;
#26576 = DIRECTION ( 'NONE',  ( -1.000000000000000000, -2.586136946169074517E-16, 0.000000000000000000 ) ) ;
#26577 = AXIS2_PLACEMENT_3D ( 'NONE', #9571, #26333, #7638 ) ;
#26578 = CARTESIAN_POINT ( 'NONE',  ( -59.60741592600796679, 2.216588895794640912, 1.589776205006679266 ) ) ;
#26579 = LINE ( 'NONE', #29278, #4074 ) ;
#26580 = DIRECTION ( 'NONE',  ( -1.000000000000000000, -3.054025858079668409E-16, 2.042474015755241579E-16 ) ) ;
#26581 = AXIS2_PLACEMENT_3D ( 'NONE', #17995, #5642, #5491 ) ;
#26583 = VERTEX_POINT ( 'NONE', #30727 ) ;
#26582 = EDGE_CURVE ( 'NONE', #12058, #22168, #26674, .T. ) ;
#26584 = AXIS2_PLACEMENT_3D ( 'NONE', #4515, #23988, #19258 ) ;
#26585 = CARTESIAN_POINT ( 'NONE',  ( 47.27788309694084745, -3.792101016927676316, -1.560991511224512740 ) ) ;
#26586 = CIRCLE ( 'NONE', #24565, 0.1000000000000002137 ) ;
#26587 = CARTESIAN_POINT ( 'NONE',  ( 16.07512358269929109, -2.917650619476095386, 4.554978966839795973 ) ) ;
#26588 = DIRECTION ( 'NONE',  ( 0.000000000000000000, 0.8740818021021506956, -0.4857787595540346559 ) ) ;
#26589 = DIRECTION ( 'NONE',  ( -1.000000000000000000, -3.053848253006669023E-16, 2.042510438544995415E-16 ) ) ;
#26590 = VERTEX_POINT ( 'NONE', #6655 ) ;
#26591 = CARTESIAN_POINT ( 'NONE',  ( -62.05495586881989567, -2.687269152040965725, 0.2433159615545962828 ) ) ;
#26592 = EDGE_CURVE ( 'NONE', #19631, #1993, #23142, .T. ) ;
#26594 = CARTESIAN_POINT ( 'NONE',  ( 53.32367365360940425, 7.956671815864365449, -1.890488970402769198 ) ) ;
#26593 = CARTESIAN_POINT ( 'NONE',  ( -59.50169947458163477, 2.403253767585081579, -1.124049747732222659 ) ) ;
#26595 = AXIS2_PLACEMENT_3D ( 'NONE', #29087, #23881, #29250 ) ;
#26596 = CARTESIAN_POINT ( 'NONE',  ( -54.49999999999999289, 1.399999999999998357, 3.300094695610798823 ) ) ;
#26598 = CARTESIAN_POINT ( 'NONE',  ( 22.58884618656104593, 6.655783678991567420, 1.424999999999921663 ) ) ;
#26597 = CARTESIAN_POINT ( 'NONE',  ( 51.88812122917230596, 8.998461838226505805, 2.049999999999819522 ) ) ;
#26599 = VERTEX_POINT ( 'NONE', #13913 ) ;
#26600 = CARTESIAN_POINT ( 'NONE',  ( -44.49999999999997868, -1.499999999999999556, -4.029888335921975262 ) ) ;
#26601 = VECTOR ( 'NONE', #17488, 1000.000000000000114 ) ;
#26602 = UNCERTAINTY_MEASURE_WITH_UNIT (LENGTH_MEASURE( 1.000000000000000082E-05 ), #7468, 'distance_accuracy_value', 'NONE');
#26603 = PLANE ( 'NONE',  #11053 ) ;
#26604 = CARTESIAN_POINT ( 'NONE',  ( 58.73097752866983967, -0.4999999999993850475, -1.835761897403959564 ) ) ;
#26605 = DIRECTION ( 'NONE',  ( 1.000000000000000000, -0.000000000000000000, -1.047444401652940007E-14 ) ) ;
#26606 = VECTOR ( 'NONE', #11129, 1000.000000000000000 ) ;
#26607 = ORIENTED_EDGE ( 'NONE', *, *, #14517, .T. ) ;
#26608 = ORIENTED_EDGE ( 'NONE', *, *, #21720, .F. ) ;
#26609 = CARTESIAN_POINT ( 'NONE',  ( 58.45000000000001705, 0.000000000000000000, 0.000000000000000000 ) ) ;
#26610 = AXIS2_PLACEMENT_3D ( 'NONE', #10665, #25379, #8132 ) ;
#26611 = AXIS2_PLACEMENT_3D ( 'NONE', #24234, #10125, #12642 ) ;
#26612 = ADVANCED_FACE ( 'NONE', ( #11572 ), #11499, .T. ) ;
#26613 = VERTEX_POINT ( 'NONE', #16161 ) ;
#26614 = AXIS2_PLACEMENT_3D ( 'NONE', #15769, #23055, #25104 ) ;
#26615 = CARTESIAN_POINT ( 'NONE',  ( 47.12445916330874951, -4.150097527438618705, 1.728039211944948139 ) ) ;
#26616 = CARTESIAN_POINT ( 'NONE',  ( -56.31249999999997868, -3.238593381231836155, -2.874284765127025576 ) ) ;
#26617 = ORIENTED_EDGE ( 'NONE', *, *, #15428, .T. ) ;
#26618 = CARTESIAN_POINT ( 'NONE',  ( -36.04518387042616467, -5.340403875751214002, -0.9205822004571946326 ) ) ;
#26619 = EDGE_LOOP ( 'NONE', ( #17667, #7796, #21726, #27833 ) ) ;
#26620 = CARTESIAN_POINT ( 'NONE',  ( 51.60223906999866728, -3.901712759401290143, -1.540267080488221030 ) ) ;
#26621 = VERTEX_POINT ( 'NONE', #3266 ) ;
#26622 =( NAMED_UNIT ( * ) SI_UNIT ( $, .STERADIAN. ) SOLID_ANGLE_UNIT ( ) );
#26624 = ORIENTED_EDGE ( 'NONE', *, *, #5008, .T. ) ;
#26623 = CIRCLE ( 'NONE', #3440, 0.04999999999999988481 ) ;
#26625 = B_SPLINE_CURVE_WITH_KNOTS ( 'NONE', 3,
 ( #15101, #3070, #388, #27292, #5608, #12715 ),
 .UNSPECIFIED., .F., .F.,
 ( 4, 2, 4 ),
 ( 9.263427422397553349E-18, 0.0001101512007266922219, 0.0002203024014533751739 ),
 .UNSPECIFIED. ) ;
#26626 = ADVANCED_FACE ( 'NONE', ( #10559 ), #8593, .T. ) ;
#26627 = VECTOR ( 'NONE', #1656, 1000.000000000000000 ) ;
#26628 = EDGE_LOOP ( 'NONE', ( #3985, #18809, #2939, #2932 ) ) ;
#26629 = VECTOR ( 'NONE', #10563, 1000.000000000000000 ) ;
#26630 = CARTESIAN_POINT ( 'NONE',  ( -57.44702994616203284, -2.078460969082631227, -3.600000000000210587 ) ) ;
#26631 = CIRCLE ( 'NONE', #30167, 0.05000000000000001665 ) ;
#26632 = CARTESIAN_POINT ( 'NONE',  ( 53.25573957143294734, 8.250120694359615925, -2.050000000000185452 ) ) ;
#26633 = CARTESIAN_POINT ( 'NONE',  ( 34.55000000000001847, 0.000000000000000000, 2.600000000000000089 ) ) ;
#26634 = DIRECTION ( 'NONE',  ( -3.491481338843133355E-15, -3.491481338843133355E-15, 1.000000000000000000 ) ) ;
#26635 = CARTESIAN_POINT ( 'NONE',  ( 60.75000000000001421, 0.5000000000006363798, 1.718465885608440047 ) ) ;
#26636 = ADVANCED_FACE ( 'NONE', ( #20071 ), #19334, .T. ) ;
#26637 =( BOUNDED_SURFACE ( )  B_SPLINE_SURFACE ( 3, 2, ( 
 ( #5969, #22595, #13072 ),
 ( #20699, #30470, #20383 ),
 ( #11022, #8631, #8774 ),
 ( #22758, #18466, #23219 ) ),
 .UNSPECIFIED., .F., .F., .F. ) 
 B_SPLINE_SURFACE_WITH_KNOTS ( ( 4, 4 ),
 ( 3, 3 ),
 ( 1.163945177512966334, 1.279805501628815900 ),
 ( 0.000000000000000000, 1.000000000000000000 ),
 .UNSPECIFIED. ) 
 GEOMETRIC_REPRESENTATION_ITEM ( )  RATIONAL_B_SPLINE_SURFACE ( (
 ( 1.000000000000000000, 0.5604218610591209515, 1.000000000000000000),
 ( 1.000000000000000000, 0.5752896509278202508, 1.000000000000000000),
 ( 1.000000000000000000, 0.5899361674293628344, 1.000000000000000000),
 ( 1.000000000000000000, 0.6043181045777068494, 1.000000000000000000) ) ) 
 REPRESENTATION_ITEM ( '' )  SURFACE ( )  );
#26638 = AXIS2_PLACEMENT_3D ( 'NONE', #5099, #21757, #28862 ) ;
#26640 = CARTESIAN_POINT ( 'NONE',  ( -36.38012252111052902, -1.026563698233164956, -5.312790900508132630 ) ) ;
#26639 = CARTESIAN_POINT ( 'NONE',  ( 51.70000000000001705, -4.179189514726507682, 0.9999999999999997780 ) ) ;
#26641 = AXIS2_PLACEMENT_3D ( 'NONE', #1188, #6578, #23052 ) ;
#26642 = ADVANCED_FACE ( 'NONE', ( #19186 ), #4593, .T. ) ;
#26643 = ADVANCED_FACE ( 'NONE', ( #4734 ), #11, .F. ) ;
#26644 = DIRECTION ( 'NONE',  ( 1.000000000000000000, 1.047444401652940007E-14, -0.000000000000000000 ) ) ;
#26645 = CARTESIAN_POINT ( 'NONE',  ( 15.18459684427940104, -2.199885893005965265, 4.939696249117676352 ) ) ;
#26647 = CARTESIAN_POINT ( 'NONE',  ( 61.25000000000003553, -0.9999999999993586242, 1.655766640118854438 ) ) ;
#26646 = CARTESIAN_POINT ( 'NONE',  ( 15.67083574136752411, 5.009497273852853816, -2.047744636826899445 ) ) ;
#26648 = ORIENTED_EDGE ( 'NONE', *, *, #22642, .F. ) ;
#26649 = LINE ( 'NONE', #9717, #14433 ) ;
#26650 = CARTESIAN_POINT ( 'NONE',  ( 47.38241355479843264, -4.256399122627302134, -1.449625929767729193 ) ) ;
#26651 = AXIS2_PLACEMENT_3D ( 'NONE', #12506, #7616, #29595 ) ;
#26653 = CARTESIAN_POINT ( 'NONE',  ( 48.45869172792486523, -1.344780351710840982, -3.858600739747802599 ) ) ;
#26652 = DIRECTION ( 'NONE',  ( -1.000000000000000000, -1.047444401652940007E-14, -0.000000000000000000 ) ) ;
#26654 = FACE_BOUND ( 'NONE', #27858, .T. ) ;
#26655 = VERTEX_POINT ( 'NONE', #24800 ) ;
#26656 = CARTESIAN_POINT ( 'NONE',  ( 51.26902472369699382, -3.881932310064108549, -1.329369065055225452 ) ) ;
#26657 = AXIS2_PLACEMENT_3D ( 'NONE', #15784, #20712, #21012 ) ;
#26658 = EDGE_CURVE ( 'NONE', #23537, #28771, #2907, .T. ) ;
#26659 = AXIS2_PLACEMENT_3D ( 'NONE', #26444, #2835, #4738 ) ;
#26660 = EDGE_LOOP ( 'NONE', ( #15813, #11212, #2993, #18776, #27200, #27813 ) ) ;
#26661 = CARTESIAN_POINT ( 'NONE',  ( 60.75000000000001421, 0.5000000000006328271, -1.718465885608478239 ) ) ;
#26662 = CARTESIAN_POINT ( 'NONE',  ( -59.44702994616203995, 4.156921938165313080, -1.958927657850919798E-13 ) ) ;
#26663 = ORIENTED_EDGE ( 'NONE', *, *, #22943, .T. ) ;
#26664 = VERTEX_POINT ( 'NONE', #6986 ) ;
#26665 = CARTESIAN_POINT ( 'NONE',  ( 50.25000000000004263, -1.791164585742575976, -0.8897917884440847969 ) ) ;
#26666 = CLOSED_SHELL ( 'NONE', ( #24934, #13303, #1496, #24640, #28970, #25155, #18022, #13077 ) ) ;
#26667 = ORIENTED_EDGE ( 'NONE', *, *, #24904, .F. ) ;
#26668 = CIRCLE ( 'NONE', #23121, 1.824999999999999956 ) ;
#26669 = DIRECTION ( 'NONE',  ( -0.000000000000000000, 0.000000000000000000, 1.000000000000000000 ) ) ;
#26670 = CIRCLE ( 'NONE', #18080, 1.000000000000000000 ) ;
#26671 = CARTESIAN_POINT ( 'NONE',  ( -56.25952994616206126, -4.643455692769913008E-15, 3.599999999999798916 ) ) ;
#26672 = ORIENTED_EDGE ( 'NONE', *, *, #29676, .F. ) ;
#26673 = CARTESIAN_POINT ( 'NONE',  ( -56.52900635094608361, 3.400000000000004352, 0.9110272542656328021 ) ) ;
#26674 = CIRCLE ( 'NONE', #25144, 0.1500000000000001887 ) ;
#26675 = CIRCLE ( 'NONE', #12998, 0.1000000000000001166 ) ;
#26676 = DIRECTION ( 'NONE',  ( 3.491481338843133355E-15, 3.491481338843133355E-15, -1.000000000000000000 ) ) ;
#26677 = ADVANCED_FACE ( 'NONE', ( #16648 ), #20234, .F. ) ;
#26678 = CARTESIAN_POINT ( 'NONE',  ( 31.50816695936848433, 7.454773701384803886, 1.949999999999889377 ) ) ;
#26679 = ORIENTED_EDGE ( 'NONE', *, *, #15556, .T. ) ;
#26680 = CARTESIAN_POINT ( 'NONE',  ( -58.81249999999996447, -0.7533615035078081723, 3.673546848079176197 ) ) ;
#26681 = EDGE_CURVE ( 'NONE', #18396, #3567, #7278, .T. ) ;
#26682 = CARTESIAN_POINT ( 'NONE',  ( 51.25000000000001421, 1.100000000000537215, -1.996089927833914146 ) ) ;
#26683 = FACE_OUTER_BOUND ( 'NONE', #29280, .T. ) ;
#26684 = DIRECTION ( 'NONE',  ( 0.000000000000000000, 0.2008964009354148039, -0.9796124928211139560 ) ) ;
#26685 = CARTESIAN_POINT ( 'NONE',  ( 56.95000000000001705, 0.6820512820512819596, 1.773360101234998210 ) ) ;
#26686 = TOROIDAL_SURFACE ( 'NONE', #16042, 2.649999999999999911, 0.05000000000000000278 ) ;
#26687 = CIRCLE ( 'NONE', #1377, 1.625000000000001332 ) ;
#26689 = CARTESIAN_POINT ( 'NONE',  ( 50.80258015808398397, 5.323456221955952384E-13, -1.996089927833914146 ) ) ;
#26688 = DIRECTION ( 'NONE',  ( 0.000000000000000000, -0.2008964009354147484, 0.9796124928211139560 ) ) ;
#26690 = EDGE_CURVE ( 'NONE', #7967, #2624, #726, .T. ) ;
#26691 = ADVANCED_FACE ( 'NONE', ( #12909 ), #23785, .T. ) ;
#26692 = CARTESIAN_POINT ( 'NONE',  ( 51.75288078123234925, -4.174487749534351977, 1.011178756798950307 ) ) ;
#26693 = FACE_OUTER_BOUND ( 'NONE', #24030, .T. ) ;
#26694 = CIRCLE ( 'NONE', #4935, 1.250000000000000222 ) ;
#26695 = CARTESIAN_POINT ( 'NONE',  ( 51.97945110550962511, 4.337541896208987779, 2.049999999999818190 ) ) ;
#26696 = VECTOR ( 'NONE', #20541, 1000.000000000000000 ) ;
#26697 = ORIENTED_EDGE ( 'NONE', *, *, #27488, .F. ) ;
#26698 = ORIENTED_EDGE ( 'NONE', *, *, #26146, .T. ) ;
#26699 = CARTESIAN_POINT ( 'NONE',  ( 58.69114869172459237, 0.5000000000006147305, -1.811349421029180284 ) ) ;
#26700 = ORIENTED_EDGE ( 'NONE', *, *, #7399, .T. ) ;
#26701 = CARTESIAN_POINT ( 'NONE',  ( 52.13000000000003098, -0.4999999999994542144, -1.996089927833914146 ) ) ;
#26702 = CARTESIAN_POINT ( 'NONE',  ( -60.78335481156722864, 3.238593381231847257, 2.874284765127023356 ) ) ;
#26704 = PLANE ( 'NONE',  #23104 ) ;
#26703 = CARTESIAN_POINT ( 'NONE',  ( 58.75000000000002132, 6.153735859711025284E-13, 3.111507638930570854E-58 ) ) ;
#26705 = CIRCLE ( 'NONE', #30734, 3.950000000000000178 ) ;
#26706 = ORIENTED_EDGE ( 'NONE', *, *, #13301, .T. ) ;
#26707 = EDGE_LOOP ( 'NONE', ( #5832, #19200, #15759, #15028, #3479, #1, #27374, #14019, #21422, #6747, #8296, #25880, #10496, #26648, #29993, #31082, #5378 ) ) ;
#26708 = CARTESIAN_POINT ( 'NONE',  ( 58.75000000000002842, -1.106298139390583302, 1.666164585743104443 ) ) ;
#26709 = AXIS2_PLACEMENT_3D ( 'NONE', #20094, #10255, #10108 ) ;
#26710 = EDGE_LOOP ( 'NONE', ( #18964, #29513, #15480, #11186 ) ) ;
#26711 = CARTESIAN_POINT ( 'NONE',  ( 23.93113343277027738, 5.410774079442639106, 1.949999999999916023 ) ) ;
#26712 = VECTOR ( 'NONE', #17075, 1000.000000000000000 ) ;
#26713 = ORIENTED_EDGE ( 'NONE', *, *, #10288, .T. ) ;
#26714 = DIRECTION ( 'NONE',  ( -1.000000000000000000, 0.000000000000000000, 1.047444401652940007E-14 ) ) ;
#26715 =( BOUNDED_SURFACE ( )  B_SPLINE_SURFACE ( 3, 2, ( 
 ( #29445, #12212, #21891 ),
 ( #27067, #26618, #179 ),
 ( #5388, #26919, #5229 ),
 ( #2859, #15048, #14736 ),
 ( #481, #12348, #5086 ),
 ( #9834, #28993, #14588 ),
 ( #29597, #7466, #12511 ),
 ( #22197, #2706, #24397 ),
 ( #22035, #10146, #17136 ),
 ( #332, #19667, #3018 ),
 ( #12661, #633, #10294 ),
 ( #7921, #24091, #17594 ),
 ( #4759, #14418, #2402 ),
 ( #12066, #23128, #30068 ),
 ( #18067, #18227, #3328 ),
 ( #15825, #15683, #22962 ) ),
 .UNSPECIFIED., .F., .F., .T. ) 
 B_SPLINE_SURFACE_WITH_KNOTS ( ( 4, 2, 2, 2, 2, 2, 2, 4 ),
 ( 3, 3 ),
 ( 0.001780502285214257806, 0.002558945925323789783, 0.002753556835351172669, 0.002948167745378555554, 0.003337389565433321326, 0.003726611385488087097, 0.004115833205542852868, 0.004894276845652385279 ),
 ( 0.000000000000000000, 1.000000000000000000 ),
 .UNSPECIFIED. ) 
 GEOMETRIC_REPRESENTATION_ITEM ( )  RATIONAL_B_SPLINE_SURFACE ( (
 ( 1.000000000000000000, 0.9418517008537213853, 1.000000000000000000),
 ( 1.000000000000000000, 0.9417987965884944135, 1.000000000000000000),
 ( 1.000000000000000000, 0.9418198861734204952, 1.000000000000000000),
 ( 1.000000000000000000, 0.9434060303845512863, 1.000000000000000000),
 ( 1.000000000000000000, 0.9437939819948102382, 1.000000000000000000),
 ( 1.000000000000000000, 0.9445989566712813534, 1.000000000000000000),
 ( 1.000000000000000000, 0.9450169930049779898, 1.000000000000000000),
 ( 1.000000000000000000, 0.9461610507673671178, 1.000000000000000000),
 ( 1.000000000000000000, 0.9467217966427039499, 1.000000000000000000),
 ( 1.000000000000000000, 0.9467345476124477965, 1.000000000000000000),
 ( 1.000000000000000000, 0.9461964028052916031, 1.000000000000000000),
 ( 1.000000000000000000, 0.9446801822473822607, 1.000000000000000000),
 ( 1.000000000000000000, 0.9437582546537023331, 1.000000000000000000),
 ( 1.000000000000000000, 0.9418129560294634661, 1.000000000000000000),
 ( 1.000000000000000000, 0.9418016889778226819, 1.000000000000000000),
 ( 1.000000000000000000, 0.9418517008537213853, 1.000000000000000000) ) ) 
 REPRESENTATION_ITEM ( '' )  SURFACE ( )  );
#26716 = ORIENTED_EDGE ( 'NONE', *, *, #8809, .T. ) ;
#26717 = CARTESIAN_POINT ( 'NONE',  ( 47.10000000000002274, 2.428612866367529932E-14, -1.644487710595116631E-13 ) ) ;
#26718 = EDGE_CURVE ( 'NONE', #16137, #12097, #15930, .T. ) ;
#26719 = CARTESIAN_POINT ( 'NONE',  ( 57.04073536323585358, 0.7493370604887438224, 1.778939771162194372 ) ) ;
#26720 = EDGE_CURVE ( 'NONE', #3768, #18823, #10993, .T. ) ;
#26721 = DIRECTION ( 'NONE',  ( -0.9396926207859095381, -0.008517430876163519654, 0.3419140708010985352 ) ) ;
#26722 = EDGE_CURVE ( 'NONE', #9911, #21964, #21651, .T. ) ;
#26723 = CARTESIAN_POINT ( 'NONE',  ( -60.32202994616201863, 2.078460969082674747, -3.600000000000205258 ) ) ;
#26724 = CARTESIAN_POINT ( 'NONE',  ( 51.39453088482484588, 4.389042235173731932, -1.550000000000179012 ) ) ;
#26725 = CARTESIAN_POINT ( 'NONE',  ( 22.32336313483207135, 6.618105965108083133, 1.549999999999922107 ) ) ;
#26726 = CARTESIAN_POINT ( 'NONE',  ( -35.85663232820581925, -3.426725943139554253, -3.937891353488750301 ) ) ;
#26727 = AXIS2_PLACEMENT_3D ( 'NONE', #10960, #8725, #1005 ) ;
#26728 = CARTESIAN_POINT ( 'NONE',  ( 15.03925126672133139, -5.377732432866646484, -0.5657657256215582464 ) ) ;
#26729 = CARTESIAN_POINT ( 'NONE',  ( -59.69999999999997442, 8.366749974758454467E-15, -2.120534355533670266E-13 ) ) ;
#26730 = VERTEX_POINT ( 'NONE', #3726 ) ;
#26731 = CARTESIAN_POINT ( 'NONE',  ( 51.80000000000002558, 6.475000000000061817, 2.049999999999819522 ) ) ;
#26733 = CARTESIAN_POINT ( 'NONE',  ( 58.64999999999999858, 1.782657835995388407, -0.5811678240976838605 ) ) ;
#26732 = CARTESIAN_POINT ( 'NONE',  ( 47.00000000000002132, -3.726179070414207928, 1.100000000000000533 ) ) ;
#26734 = DIRECTION ( 'NONE',  ( -0.09218405009745890555, 0.9957419851084061690, 4.429949212628659047E-16 ) ) ;
#26735 = ORIENTED_EDGE ( 'NONE', *, *, #22066, .F. ) ;
#26736 = CARTESIAN_POINT ( 'NONE',  ( -54.49608498031047787, 1.530604779201329091, 4.051096982736678953 ) ) ;
#26737 = ORIENTED_EDGE ( 'NONE', *, *, #29511, .F. ) ;
#26738 = CARTESIAN_POINT ( 'NONE',  ( 15.39414421509791353, 0.2904410314644420565, -5.200000000384609855 ) ) ;
#26739 = CARTESIAN_POINT ( 'NONE',  ( -35.85663232820579083, -4.861582140531640839, 2.394243978978324972 ) ) ;
#26741 = CARTESIAN_POINT ( 'NONE',  ( -61.36283645075994286, -2.621142715471549423, -0.6477737761984685427 ) ) ;
#26740 = DIRECTION ( 'NONE',  ( 0.000000000000000000, 0.000000000000000000, 1.000000000000000000 ) ) ;
#26742 = VERTEX_POINT ( 'NONE', #17845 ) ;
#26743 = CARTESIAN_POINT ( 'NONE',  ( 58.64999999999999858, 1.972190280208463209, 0.1053114364810046055 ) ) ;
#26744 = DIRECTION ( 'NONE',  ( 0.000000000000000000, 0.000000000000000000, -1.000000000000000000 ) ) ;
#26746 = CARTESIAN_POINT ( 'NONE',  ( -54.48478889579405404, -1.513794642953540270, -4.039462313877657529 ) ) ;
#26745 = DIRECTION ( 'NONE',  ( 1.000000000000000000, 1.047444401652940007E-14, 0.000000000000000000 ) ) ;
#26747 = ORIENTED_EDGE ( 'NONE', *, *, #18427, .T. ) ;
#26748 = CARTESIAN_POINT ( 'NONE',  ( -60.68749999999996447, 0.8699069336946680941, -4.241846523238426592 ) ) ;
#26749 = DIRECTION ( 'NONE',  ( 1.000000000000000000, 3.053848253006669023E-16, -2.042510438544995415E-16 ) ) ;
#26750 = CARTESIAN_POINT ( 'NONE',  ( -60.54800159808252147, 1.949167012834402697E-15, 6.802637593289325421E-16 ) ) ;
#26751 = COLOUR_RGB ( '', 0.66274510, 0.83137255, 0.94901961) ;
#26752 = ADVANCED_FACE ( 'NONE', ( #11312 ), #27482, .F. ) ;
#26753 = AXIS2_PLACEMENT_3D ( 'NONE', #614, #14570, #2545 ) ;
#26754 = CARTESIAN_POINT ( 'NONE',  ( -54.49999999999997868, -3.745083032500879039, 0.1919715595446555012 ) ) ;
#26755 = CARTESIAN_POINT ( 'NONE',  ( -57.72099364905386665, -3.399999999999994138, 0.9110272542655947214 ) ) ;
#26756 = FACE_BOUND ( 'NONE', #15920, .T. ) ;
#26757 = ORIENTED_EDGE ( 'NONE', *, *, #29572, .F. ) ;
#26758 = DIRECTION ( 'NONE',  ( -1.000000000000000000, -0.000000000000000000, -0.000000000000000000 ) ) ;
#26759 = CARTESIAN_POINT ( 'NONE',  ( 27.87224558658655482, 5.458855767854803531, -1.950000000000095435 ) ) ;
#26760 = DIRECTION ( 'NONE',  ( 1.000000000000000000, 3.054025858079668409E-16, -2.042474015755241579E-16 ) ) ;
#26761 = EDGE_CURVE ( 'NONE', #6108, #28026, #29678, .T. ) ;
#26762 = CARTESIAN_POINT ( 'NONE',  ( -59.47497210890824704, 3.405470396758961904, -1.108618695965261969 ) ) ;
#26763 = CARTESIAN_POINT ( 'NONE',  ( 49.00000000000004974, 1.401298464324817071E-42, 2.674999999999486011 ) ) ;
#26765 = CARTESIAN_POINT ( 'NONE',  ( -59.19495429951913223, -2.548385458854336871, -0.9469503383366065785 ) ) ;
#26764 = CARTESIAN_POINT ( 'NONE',  ( 61.25000000000000000, 1.996089927834492350, 0.1250000000010043355 ) ) ;
#26766 = VERTEX_POINT ( 'NONE', #10705 ) ;
#26767 = CIRCLE ( 'NONE', #7067, 5.338914163118009704 ) ;
#26768 = DIRECTION ( 'NONE',  ( 0.000000000000000000, -0.9996898646859344595, -0.02490330187381124133 ) ) ;
#26769 = ORIENTED_EDGE ( 'NONE', *, *, #30850, .F. ) ;
#26770 = CARTESIAN_POINT ( 'NONE',  ( 61.00000000000001421, 0.8112099027105408311, 1.409560742431902103 ) ) ;
#26772 = CARTESIAN_POINT ( 'NONE',  ( -59.59999999999998010, 8.366749974758452890E-15, -2.117042874194827196E-13 ) ) ;
#26771 = CARTESIAN_POINT ( 'NONE',  ( 15.66436536804551594, -2.847679722116473133, -4.601476325142666468 ) ) ;
#26773 = CARTESIAN_POINT ( 'NONE',  ( 58.65000000000000568, 1.671477153794444392, 0.8495817349409554575 ) ) ;
#26774 = EDGE_LOOP ( 'NONE', ( #24991, #16790, #2441, #18290 ) ) ;
#26775 = ORIENTED_EDGE ( 'NONE', *, *, #19496, .F. ) ;
#26776 = CARTESIAN_POINT ( 'NONE',  ( 68.00000000000000000, 0.7500000000000000000, -1.988246715074068582 ) ) ;
#26777 = ORIENTED_EDGE ( 'NONE', *, *, #17984, .F. ) ;
#26778 = CARTESIAN_POINT ( 'NONE',  ( 56.95000053796676553, -0.7321038892619347038, -1.754109389045036771 ) ) ;
#26779 = CARTESIAN_POINT ( 'NONE',  ( -54.67292740578360366, -3.330682475591782765, -0.6830477631804114935 ) ) ;
#26780 = ORIENTED_EDGE ( 'NONE', *, *, #16973, .T. ) ;
#26781 = DIRECTION ( 'NONE',  ( 1.000000000000000000, 1.047444401652940007E-14, -0.000000000000000000 ) ) ;
#26782 = ORIENTED_EDGE ( 'NONE', *, *, #16203, .T. ) ;
#26783 = ADVANCED_FACE ( 'NONE', ( #8635 ), #30473, .F. ) ;
#26784 = CARTESIAN_POINT ( 'NONE',  ( -60.51905989232411542, -2.944486372867088697, 1.699999999999773914 ) ) ;
#26785 = CIRCLE ( 'NONE', #23763, 10.00000000000000178 ) ;
#26786 = ORIENTED_EDGE ( 'NONE', *, *, #357, .F. ) ;
#26787 = VECTOR ( 'NONE', #18011, 1000.000000000000000 ) ;
#26788 = VECTOR ( 'NONE', #23911, 1000.000000000000114 ) ;
#26789 = CARTESIAN_POINT ( 'NONE',  ( -60.07202994616204705, 2.078460969082646770, 3.599999999999794031 ) ) ;
#26790 = CARTESIAN_POINT ( 'NONE',  ( 50.45717930666029361, 1.210123066480781606, 3.917958458743180827 ) ) ;
#26791 = FACE_OUTER_BOUND ( 'NONE', #2798, .T. ) ;
#26792 = DIRECTION ( 'NONE',  ( -4.270088556250598741E-15, 0.000000000000000000, -1.000000000000000000 ) ) ;
#26793 = CIRCLE ( 'NONE', #1511, 1.000000000000000000 ) ;
#26795 = LINE ( 'NONE', #27086, #24050 ) ;
#26794 = CYLINDRICAL_SURFACE ( 'NONE', #26638, 0.05000000000000012768 ) ;
#26796 = CARTESIAN_POINT ( 'NONE',  ( 46.99360240935735078, -4.235057606083818982, 1.098058400101960652 ) ) ;
#26797 = CARTESIAN_POINT ( 'NONE',  ( -61.34999999999997300, -2.515554072771550853, -0.7899129066418597578 ) ) ;
#26799 = CARTESIAN_POINT ( 'NONE',  ( 51.24099374247644789, 1.086790822299314785, -1.208135181987622708 ) ) ;
#26798 = CARTESIAN_POINT ( 'NONE',  ( 58.75000000000000711, 1.499837071478669959, -1.323060376180706710 ) ) ;
#26800 = EDGE_LOOP ( 'NONE', ( #19958, #13234, #4245, #6906 ) ) ;
#26801 = CARTESIAN_POINT ( 'NONE',  ( -44.49999999999996447, -1.514093959731525496, -3.183260039818558429 ) ) ;
#26802 = FACE_OUTER_BOUND ( 'NONE', #15611, .T. ) ;
#26804 = CARTESIAN_POINT ( 'NONE',  ( -35.85663232820584057, -3.056483311920853208, -4.206888370749738648 ) ) ;
#26803 = CARTESIAN_POINT ( 'NONE',  ( 51.25000000000001421, 0.6500000000005367040, -1.489337100860647967 ) ) ;
#26805 = VERTEX_POINT ( 'NONE', #25742 ) ;
#26806 = CARTESIAN_POINT ( 'NONE',  ( -59.69999999999997442, 8.366749974758454467E-15, -2.120534355533670266E-13 ) ) ;
#26807 = ORIENTED_EDGE ( 'NONE', *, *, #31098, .T. ) ;
#26808 = VECTOR ( 'NONE', #9421, 1000.000000000000000 ) ;
#26809 = CARTESIAN_POINT ( 'NONE',  ( 16.00221665700884088, -4.939398376933302082, 2.210903708596471340 ) ) ;
#26810 = EDGE_LOOP ( 'NONE', ( #17472, #4214, #18909 ) ) ;
#26811 = ORIENTED_EDGE ( 'NONE', *, *, #10229, .F. ) ;
#26812 = DIRECTION ( 'NONE',  ( 0.000000000000000000, -1.000000000000000000, 0.000000000000000000 ) ) ;
#26813 = EDGE_LOOP ( 'NONE', ( #7682, #19078, #16538, #30776 ) ) ;
#26814 = AXIS2_PLACEMENT_3D ( 'NONE', #15128, #10222, #19891 ) ;
#26815 = DIRECTION ( 'NONE',  ( 0.9993908270190956511, -0.03489949670250202390, -3.491481338843132961E-15 ) ) ;
#26816 = EDGE_CURVE ( 'NONE', #29802, #5422, #21389, .T. ) ;
#26817 = CARTESIAN_POINT ( 'NONE',  ( -57.44702994616203284, -2.078460969082631227, -3.600000000000210587 ) ) ;
#26818 = EDGE_LOOP ( 'NONE', ( #18477, #21958, #3990, #30974 ) ) ;
#26819 = EDGE_CURVE ( 'NONE', #22989, #1198, #10474, .T. ) ;
#26820 = EDGE_CURVE ( 'NONE', #24297, #16594, #4913, .T. ) ;
#26821 = CARTESIAN_POINT ( 'NONE',  ( 51.14630318392394770, 0.9364487020639118420, -1.503522130792751987 ) ) ;
#26822 = EDGE_CURVE ( 'NONE', #17335, #22245, #18311, .T. ) ;
#26823 = CARTESIAN_POINT ( 'NONE',  ( 32.57869118458520319, 7.908463456459324803, 1.949999999999884936 ) ) ;
#26824 = EDGE_LOOP ( 'NONE', ( #9790, #4611, #28035, #3241 ) ) ;
#26825 =( BOUNDED_CURVE ( )  B_SPLINE_CURVE ( 3, ( #11396, #18706, #13441, #23143 ),
 .UNSPECIFIED., .F., .T. ) 
 B_SPLINE_CURVE_WITH_KNOTS ( ( 4, 4 ),
 ( 1.817784745758537435, 2.232964403949253551 ),
 .UNSPECIFIED. ) 
 CURVE ( )  GEOMETRIC_REPRESENTATION_ITEM ( )  RATIONAL_B_SPLINE_CURVE ( ( 1.000000000000000000, 0.9856869983806464397, 0.9856869983806464397, 1.000000000000000000 ) ) 
 REPRESENTATION_ITEM ( '' )  );
#26826 = CARTESIAN_POINT ( 'NONE',  ( 51.78977120336473661, -4.154252208774217969, -1.054526470899727508 ) ) ;
#26827 = CARTESIAN_POINT ( 'NONE',  ( 51.29845177546386026, 3.894758067259835421, -2.050000000000178790 ) ) ;
#26828 = DIRECTION ( 'NONE',  ( 1.000000000000000000, 3.125586771759065906E-16, 0.000000000000000000 ) ) ;
#26829 = LINE ( 'NONE', #27131, #11945 ) ;
#26830 = DIRECTION ( 'NONE',  ( 0.000000000000000000, -1.224646799147353207E-16, 1.000000000000000000 ) ) ;
#26831 = EDGE_CURVE ( 'NONE', #8781, #28086, #24162, .T. ) ;
#26833 = DIRECTION ( 'NONE',  ( 1.000000000000000000, 1.047444401652940007E-14, 0.000000000000000000 ) ) ;
#26832 = CARTESIAN_POINT ( 'NONE',  ( -36.31440869660537629, -3.100731772197714342, 4.174739983989991465 ) ) ;
#26834 = AXIS2_PLACEMENT_3D ( 'NONE', #5198, #7880, #20412 ) ;
#26835 = CARTESIAN_POINT ( 'NONE',  ( 51.38214458811555829, 1.084857585946179315, 1.209959298770756808 ) ) ;
#26836 = CARTESIAN_POINT ( 'NONE',  ( 52.15659567665549901, 0.5000000000005454526, -1.807104036850122331 ) ) ;
#26837 = CARTESIAN_POINT ( 'NONE',  ( 52.54946733419066618, 4.465216787881845839, 1.565330858589529806 ) ) ;
#26838 = EDGE_LOOP ( 'NONE', ( #14615, #1409, #625, #5158 ) ) ;
#26839 = ADVANCED_FACE ( 'NONE', ( #29863 ), #27811, .T. ) ;
#26840 = VERTEX_POINT ( 'NONE', #22762 ) ;
#26841 = DIRECTION ( 'NONE',  ( 0.000000000000000000, 0.000000000000000000, -1.000000000000000000 ) ) ;
#26842 = CARTESIAN_POINT ( 'NONE',  ( -56.04792740578360366, -1.073804522883516688, -3.225979517392335794 ) ) ;
#26844 = CARTESIAN_POINT ( 'NONE',  ( 58.75000000000003553, -1.800471618824212694, -1.039502773796582069 ) ) ;
#26843 = DIRECTION ( 'NONE',  ( 1.000000000000000000, 1.047444401652940007E-14, 0.000000000000000000 ) ) ;
#26845 = ORIENTED_EDGE ( 'NONE', *, *, #7519, .T. ) ;
#26846 = ORIENTED_EDGE ( 'NONE', *, *, #28595, .T. ) ;
#26847 = CARTESIAN_POINT ( 'NONE',  ( 27.27214205000342062, 5.011961650406415281, -1.950000000000094769 ) ) ;
#26848 = ADVANCED_FACE ( 'NONE', ( #6431 ), #16093, .T. ) ;
#26849 = VERTEX_POINT ( 'NONE', #3586 ) ;
#26850 = CARTESIAN_POINT ( 'NONE',  ( -44.49999999999999289, -1.499999999999999556, 4.029888335921975262 ) ) ;
#26851 = EDGE_CURVE ( 'NONE', #25588, #24297, #13222, .T. ) ;
#26852 = CIRCLE ( 'NONE', #9162, 0.1000000000000000472 ) ;
#26853 = CARTESIAN_POINT ( 'NONE',  ( 61.25000000000001421, 1.000000000000641709, 1.586072192556190252 ) ) ;
#26854 = EDGE_CURVE ( 'NONE', #21024, #6022, #15772, .T. ) ;
#26855 = FACE_OUTER_BOUND ( 'NONE', #6753, .T. ) ;
#26856 = CARTESIAN_POINT ( 'NONE',  ( 69.25000000000004263, 4.557543281186736018E-17, 2.749999999999274358 ) ) ;
#26857 = CARTESIAN_POINT ( 'NONE',  ( -55.83155989232411542, -1.962990915244706924, -3.400000000000204636 ) ) ;
#26858 = CARTESIAN_POINT ( 'NONE',  ( 53.75952070206891875, 7.747157889885662563, -2.050000000000187228 ) ) ;
#26859 = CARTESIAN_POINT ( 'NONE',  ( 36.55000000000001847, 2.265596578422603100E-16, 1.850000000000000089 ) ) ;
#26860 = CARTESIAN_POINT ( 'NONE',  ( -35.85663232820579793, -4.018128179617549200, -3.618665901676661800 ) ) ;
#26861 = MECHANICAL_DESIGN_GEOMETRIC_PRESENTATION_REPRESENTATION (  '', ( #1084 ), #24830 ) ;
#26862 = CARTESIAN_POINT ( 'NONE',  ( -62.29999999999998295, 1.106939637198029038E-15, 2.238576962872695299E-15 ) ) ;
#26863 = FACE_OUTER_BOUND ( 'NONE', #5009, .T. ) ;
#26864 = VERTEX_POINT ( 'NONE', #8949 ) ;
#26865 = EDGE_CURVE ( 'NONE', #24464, #473, #9123, .T. ) ;
#26866 = CARTESIAN_POINT ( 'NONE',  ( 15.03925126672132784, 5.377732432866636714, 0.5657657256216092057 ) ) ;
#26867 = CARTESIAN_POINT ( 'NONE',  ( -36.48821680285139735, -2.849134329833951096, -4.601168830303078217 ) ) ;
#26868 = CARTESIAN_POINT ( 'NONE',  ( 54.11548317488421134, 5.698162681109456784, 2.049999999999810640 ) ) ;
#26869 = ORIENTED_EDGE ( 'NONE', *, *, #13176, .F. ) ;
#26870 = CYLINDRICAL_SURFACE ( 'NONE', #8272, 0.1499999999999999667 ) ;
#26871 = ORIENTED_EDGE ( 'NONE', *, *, #12385, .F. ) ;
#26872 = ADVANCED_FACE ( 'NONE', ( #21648 ), #26046, .F. ) ;
#26873 = DIRECTION ( 'NONE',  ( 1.000000000000000000, -1.219044193948983948E-29, 3.491481338843133355E-15 ) ) ;
#26874 = DIRECTION ( 'NONE',  ( -2.117927888850090838E-16, 0.02490330187381123786, -0.9996898646859343485 ) ) ;
#26876 = CARTESIAN_POINT ( 'NONE',  ( 22.07280086217093640, 8.086143481909152442, -1.950000000000076339 ) ) ;
#26875 = DIRECTION ( 'NONE',  ( 1.000000000000000000, 1.047444401652940007E-14, 0.000000000000000000 ) ) ;
#26877 = ORIENTED_EDGE ( 'NONE', *, *, #28613, .F. ) ;
#26878 = DIRECTION ( 'NONE',  ( 1.000000000000000000, 3.053848253006669023E-16, -2.042510438544995415E-16 ) ) ;
#26879 = CIRCLE ( 'NONE', #29905, 0.09999999999999996392 ) ;
#26881 = CARTESIAN_POINT ( 'NONE',  ( -54.46439202372638277, -1.502116081466616793, -4.031358338852112588 ) ) ;
#26880 = CARTESIAN_POINT ( 'NONE',  ( 53.43503425481907954, 4.477923827963745218, 2.048707174794345942 ) ) ;
#26882 = CARTESIAN_POINT ( 'NONE',  ( -35.85663232820584057, 3.275050215668857234, 2.949461045527371983 ) ) ;
#26883 = CARTESIAN_POINT ( 'NONE',  ( -59.06249999999997158, 4.108500314926511798, -1.367561758111406789 ) ) ;
#26884 = CARTESIAN_POINT ( 'NONE',  ( 61.24959995150299363, 0.9774770340133932534, 1.663387054287940092 ) ) ;
#26885 = CARTESIAN_POINT ( 'NONE',  ( 34.50000000000001421, 0.000000000000000000, -2.649999999999999911 ) ) ;
#26886 = CARTESIAN_POINT ( 'NONE',  ( -55.06249999999997158, -0.7533615035078029543, 3.673546848079176197 ) ) ;
#26887 = AXIS2_PLACEMENT_3D ( 'NONE', #27977, #28138, #1387 ) ;
#26888 = CARTESIAN_POINT ( 'NONE',  ( -54.81249999999997868, -3.238593381231840151, -2.874284765127020691 ) ) ;
#26889 = CARTESIAN_POINT ( 'NONE',  ( 51.70000000000001705, -4.179189514726508570, -0.9000000000000002442 ) ) ;
#26890 = CARTESIAN_POINT ( 'NONE',  ( 51.89161117884413699, 9.098400920926795976, -2.050000000000180123 ) ) ;
#26891 = ORIENTED_EDGE ( 'NONE', *, *, #18193, .T. ) ;
#26892 = CARTESIAN_POINT ( 'NONE',  ( 58.65000000000001990, 6.143261415694495821E-13, 3.111507638930570854E-58 ) ) ;
#26893 = CARTESIAN_POINT ( 'NONE',  ( 24.09848814319705568, 5.630607826402612481, -1.950000000000083666 ) ) ;
#26894 = LINE ( 'NONE', #24375, #19081 ) ;
#26895 = CARTESIAN_POINT ( 'NONE',  ( 15.03925126672132961, 1.123735532908305634, 5.289358697221540950 ) ) ;
#26896 = AXIS2_PLACEMENT_3D ( 'NONE', #27976, #28614, #4383 ) ;
#26897 = EDGE_CURVE ( 'NONE', #9415, #5317, #18601, .T. ) ;
#26898 = CARTESIAN_POINT ( 'NONE',  ( 61.24019690292481499, -0.9013423465685174163, 1.739682280371792178 ) ) ;
#26900 = CARTESIAN_POINT ( 'NONE',  ( 22.07284336892448096, 7.567314370317718364, 1.424999999999923439 ) ) ;
#26899 = CARTESIAN_POINT ( 'NONE',  ( 58.65000076404082563, 0.5493821916573852215, 1.793020333199914385 ) ) ;
#26901 = EDGE_CURVE ( 'NONE', #4064, #27932, #4354, .T. ) ;
#26902 = ORIENTED_EDGE ( 'NONE', *, *, #22288, .F. ) ;
#26903 = CARTESIAN_POINT ( 'NONE',  ( 58.73371041428940487, -1.830356084954447793, 0.4073466955389919431 ) ) ;
#26904 = ORIENTED_EDGE ( 'NONE', *, *, #9699, .T. ) ;
#26905 = UNCERTAINTY_MEASURE_WITH_UNIT (LENGTH_MEASURE( 1.000000000000000082E-05 ), #437, 'distance_accuracy_value', 'NONE');
#26906 = EDGE_CURVE ( 'NONE', #18872, #26583, #30039, .T. ) ;
#26907 = CARTESIAN_POINT ( 'NONE',  ( 56.95000000000001705, 0.000000000000000000, 0.000000000000000000 ) ) ;
#26909 = CARTESIAN_POINT ( 'NONE',  ( 58.74664129364624898, -0.4999999999993849364, -1.856789660955697308 ) ) ;
#26908 = CARTESIAN_POINT ( 'NONE',  ( 57.00555950015162665, 0.7236022373656367801, -2.438089627148707805 ) ) ;
#26910 = DIRECTION ( 'NONE',  ( 6.938893903907228378E-15, 1.734723475976807094E-15, 1.000000000000000000 ) ) ;
#26911 = VERTEX_POINT ( 'NONE', #13833 ) ;
#26912 = ORIENTED_EDGE ( 'NONE', *, *, #3762, .T. ) ;
#26913 = CARTESIAN_POINT ( 'NONE',  ( -57.53335481156722864, -4.108500314926509134, 1.367561758111407455 ) ) ;
#26914 = FACE_OUTER_BOUND ( 'NONE', #16746, .T. ) ;
#26915 = ORIENTED_EDGE ( 'NONE', *, *, #21435, .T. ) ;
#26916 = DIRECTION ( 'NONE',  ( 0.000000000000000000, 1.000000000000000000, 3.491481338843252079E-15 ) ) ;
#26917 = CARTESIAN_POINT ( 'NONE',  ( -55.36042740578360366, -2.936324665650200672, -2.606018187048498191 ) ) ;
#26918 = AXIS2_PLACEMENT_3D ( 'NONE', #13306, #15716, #25363 ) ;
#26919 = CARTESIAN_POINT ( 'NONE',  ( -36.22818246778668794, -5.326563020867394194, -0.9981196555229843170 ) ) ;
#26920 = ORIENTED_EDGE ( 'NONE', *, *, #21672, .T. ) ;
#26921 = CARTESIAN_POINT ( 'NONE',  ( 0.000000000000000000, 0.000000000000000000, 0.000000000000000000 ) ) ;
#26922 = EDGE_CURVE ( 'NONE', #29622, #26053, #30806, .T. ) ;
#26923 = DIRECTION ( 'NONE',  ( 0.000000000000000000, 0.000000000000000000, 1.000000000000000000 ) ) ;
#26924 = APPLICATION_CONTEXT ( 'automotive_design' ) ;
#26925 = ORIENTED_EDGE ( 'NONE', *, *, #27206, .T. ) ;
#26926 = CARTESIAN_POINT ( 'NONE',  ( -57.94702994616203995, 4.156921938165313080, -1.906555437768272735E-13 ) ) ;
#26927 = CARTESIAN_POINT ( 'NONE',  ( -67.99999999999995737, 0.5554785485864213168, -2.708628542650378890 ) ) ;
#26928 = CARTESIAN_POINT ( 'NONE',  ( 48.39103590182073589, -1.199904535326233646, -3.921111011342365504 ) ) ;
#26929 = PRODUCT_RELATED_PRODUCT_CATEGORY ( 'part', '', ( #26984 ) ) ;
#26930 = CARTESIAN_POINT ( 'NONE',  ( -54.47366401599046526, -1.505709097230404803, 3.303769268891089350 ) ) ;
#26931 = DIRECTION ( 'NONE',  ( -1.000000000000000000, 0.000000000000000000, 1.047444401652940007E-14 ) ) ;
#26932 = FACE_OUTER_BOUND ( 'NONE', #27182, .T. ) ;
#26934 = CARTESIAN_POINT ( 'NONE',  ( -36.22955757456079340, -0.2668145608218571163, -5.199999998579026617 ) ) ;
#26933 = DIRECTION ( 'NONE',  ( -1.000000000000000000, 0.000000000000000000, 1.047444401652940007E-14 ) ) ;
#26935 = CIRCLE ( 'NONE', #2169, 2.600000000000000089 ) ;
#26936 = DIRECTION ( 'NONE',  ( -1.000000000000000000, -1.047444401652940007E-14, -0.000000000000000000 ) ) ;
#26937 = DIRECTION ( 'NONE',  ( 0.000000000000000000, 2.529805069132844337E-15, -1.000000000000000000 ) ) ;
#26939 = CARTESIAN_POINT ( 'NONE',  ( 57.05000000000001847, -0.7500000000000000000, 2.421260002560650104 ) ) ;
#26938 = DIRECTION ( 'NONE',  ( 1.000000000000000000, -1.219044193948983948E-29, 3.491481338843133355E-15 ) ) ;
#26940 = EDGE_CURVE ( 'NONE', #26017, #28731, #28190, .T. ) ;
#26941 = ORIENTED_EDGE ( 'NONE', *, *, #708, .F. ) ;
#26942 = DIRECTION ( 'NONE',  ( 0.000000000000000000, 0.000000000000000000, -1.000000000000000000 ) ) ;
#26943 = CARTESIAN_POINT ( 'NONE',  ( 51.80000000000002558, 3.850000000000016520, 1.678541033159270279 ) ) ;
#26945 = CARTESIAN_POINT ( 'NONE',  ( 58.65000000000001990, 6.143261415694495821E-13, 3.111507638930570854E-58 ) ) ;
#26944 = CARTESIAN_POINT ( 'NONE',  ( 15.98305126557416855, 3.597789892641498621, -4.037455662930067746 ) ) ;
#26946 = CARTESIAN_POINT ( 'NONE',  ( 57.00000000000001421, 0.7263660278559024297, 2.436986164851962844 ) ) ;
#26947 = ORIENTED_EDGE ( 'NONE', *, *, #26761, .T. ) ;
#26948 = DIRECTION ( 'NONE',  ( 1.000000000000000000, -1.219044193948983948E-29, 3.491481338843133355E-15 ) ) ;
#26949 = ORIENTED_EDGE ( 'NONE', *, *, #14824, .T. ) ;
#26950 = DIRECTION ( 'NONE',  ( 0.9993908270190956511, -0.03489949670250202390, -3.491481338843132961E-15 ) ) ;
#26951 = ORIENTED_EDGE ( 'NONE', *, *, #26283, .F. ) ;
#26952 = ORIENTED_EDGE ( 'NONE', *, *, #14032, .T. ) ;
#26953 = CARTESIAN_POINT ( 'NONE',  ( 47.06312566212017146, 8.366466760780054912, 1.949999999999836087 ) ) ;
#26954 = VERTEX_POINT ( 'NONE', #19106 ) ;
#26955 = CARTESIAN_POINT ( 'NONE',  ( 57.05000000000001847, -0.8000000000000002665, 2.421260002560650104 ) ) ;
#26956 = ADVANCED_FACE ( 'NONE', ( #4522, #19266 ), #30963, .T. ) ;
#26957 = CARTESIAN_POINT ( 'NONE',  ( -60.19702994616203995, 4.156921938165313080, -1.985113767892243204E-13 ) ) ;
#26958 = EDGE_LOOP ( 'NONE', ( #29847, #18448 ) ) ;
#26959 = CARTESIAN_POINT ( 'NONE',  ( -44.49999999999999289, 0.000000000000000000, 0.000000000000000000 ) ) ;
#26960 = CIRCLE ( 'NONE', #29005, 1.875000000000001776 ) ;
#26961 = DIRECTION ( 'NONE',  ( 1.000000000000000000, 2.586136946169074517E-16, -0.000000000000000000 ) ) ;
#26962 = CIRCLE ( 'NONE', #12801, 1.975000000000001865 ) ;
#26963 = CARTESIAN_POINT ( 'NONE',  ( 25.08803375996945917, 5.428914793826548291, 2.049999999999911893 ) ) ;
#26964 = ORIENTED_EDGE ( 'NONE', *, *, #19144, .T. ) ;
#26965 = FACE_OUTER_BOUND ( 'NONE', #17874, .T. ) ;
#26966 = CARTESIAN_POINT ( 'NONE',  ( -54.45487361440510909, -1.499999999999999112, 4.029888335921975262 ) ) ;
#26967 = CARTESIAN_POINT ( 'NONE',  ( 58.72200624034167760, -0.9185080301417619664, -1.634766674884353010 ) ) ;
#26968 = DIRECTION ( 'NONE',  ( 0.000000000000000000, 0.000000000000000000, 1.000000000000000000 ) ) ;
#26969 = EDGE_CURVE ( 'NONE', #18051, #26216, #31111, .T. ) ;
#26970 = CARTESIAN_POINT ( 'NONE',  ( 57.02007310689670305, 0.7405013978967619481, 2.427462356522636533 ) ) ;
#26971 = APPLICATION_CONTEXT ( 'automotive_design' ) ;
#26973 = CARTESIAN_POINT ( 'NONE',  ( 50.25000000000000711, 1.039502773797110979, -1.800471618823823450 ) ) ;
#26972 = CARTESIAN_POINT ( 'NONE',  ( -36.77443515226921278, -3.646557212684091276, 3.995389720703579339 ) ) ;
#26974 = CARTESIAN_POINT ( 'NONE',  ( 65.00000000000001421, -1.025519176787267142E-28, -6.808388610744108654E-13 ) ) ;
#26975 = CARTESIAN_POINT ( 'NONE',  ( -56.72499999999997300, 4.506217466977128439, 0.9241234443029089363 ) ) ;
#26976 = EDGE_CURVE ( 'NONE', #24355, #14302, #12022, .T. ) ;
#26977 = DIRECTION ( 'NONE',  ( -2.581436205204234499E-16, 0.9796124928211140670, 0.2008964009354147762 ) ) ;
#26978 = AXIS2_PLACEMENT_3D ( 'NONE', #27341, #13085, #22770 ) ;
#26979 = VERTEX_POINT ( 'NONE', #23520 ) ;
#26980 = VERTEX_POINT ( 'NONE', #6900 ) ;
#26981 = B_SPLINE_CURVE_WITH_KNOTS ( 'NONE', 3,
 ( #9047, #5183, #14832, #23454, #1923, #1744, #135, #24493, #18874, #11414 ),
 .UNSPECIFIED., .F., .F.,
 ( 4, 2, 2, 2, 4 ),
 ( 0.000000000000000000, 0.0004363777631660865864, 0.0006545666447491310181, 0.0007636610855406569202, 0.0008727555263321828223 ),
 .UNSPECIFIED. ) ;
#26982 = VERTEX_POINT ( 'NONE', #23847 ) ;
#26983 = DIRECTION ( 'NONE',  ( 0.000000000000000000, -1.000000000000000000, -3.491481338843131383E-15 ) ) ;
#26984 = PRODUCT ( 'Rotator Head', 'Rotator Head', '', ( #20442 ) ) ;
#26985 = CARTESIAN_POINT ( 'NONE',  ( -57.67292740578359656, -3.330682475591783209, -0.6830477631804108274 ) ) ;
#26987 = DIRECTION ( 'NONE',  ( 0.9993908270190956511, -0.03489949670250202390, -3.491481338843132961E-15 ) ) ;
#26986 = DIRECTION ( 'NONE',  ( 3.002035892788116966E-16, -0.9996898646859343485, -0.02490330187381123786 ) ) ;
#26988 = ORIENTED_EDGE ( 'NONE', *, *, #28754, .F. ) ;
#26989 = ORIENTED_EDGE ( 'NONE', *, *, #27008, .T. ) ;
#26990 = CARTESIAN_POINT ( 'NONE',  ( 54.18129837870574050, 6.362043366690858903, -2.050000000000185008 ) ) ;
#26991 = ORIENTED_EDGE ( 'NONE', *, *, #14851, .F. ) ;
#26992 = LINE ( 'NONE', #28917, #13023 ) ;
#26993 = EDGE_CURVE ( 'NONE', #20519, #1750, #1821, .T. ) ;
#26994 =( BOUNDED_CURVE ( )  B_SPLINE_CURVE ( 3, ( #2391, #168, #11883, #19345 ),
 .UNSPECIFIED., .F., .T. ) 
 B_SPLINE_CURVE_WITH_KNOTS ( ( 4, 4 ),
 ( 4.041453792691655167, 4.300872134317202722 ),
 .UNSPECIFIED. ) 
 CURVE ( )  GEOMETRIC_REPRESENTATION_ITEM ( )  RATIONAL_B_SPLINE_CURVE ( ( 1.000000000000000000, 0.9943997021150918769, 0.9943997021150918769, 1.000000000000000000 ) ) 
 REPRESENTATION_ITEM ( '' )  );
#26995 = ORIENTED_EDGE ( 'NONE', *, *, #5206, .T. ) ;
#26996 = CARTESIAN_POINT ( 'NONE',  ( 29.93605863095885056, 6.616288078318222077, -2.050000000000103295 ) ) ;
#26997 = CARTESIAN_POINT ( 'NONE',  ( -57.14405989232411542, 2.944486372867110457, -1.700000000000182920 ) ) ;
#26998 = CARTESIAN_POINT ( 'NONE',  ( 15.61033468494299470, -4.977801270594324201, -2.126472881633288736 ) ) ;
#27000 = CARTESIAN_POINT ( 'NONE',  ( -60.82202994616204705, 2.078460969082646770, 3.599999999999791367 ) ) ;
#26999 = CIRCLE ( 'NONE', #11846, 4.786668705877438867 ) ;
#27001 = EDGE_CURVE ( 'NONE', #6668, #15602, #25303, .T. ) ;
#27002 = CARTESIAN_POINT ( 'NONE',  ( 52.48717296556561251, 8.620750214766545128, -2.050000000000182343 ) ) ;
#27003 = DIRECTION ( 'NONE',  ( 1.000000000000000000, 0.000000000000000000, -0.000000000000000000 ) ) ;
#27004 = CARTESIAN_POINT ( 'NONE',  ( 50.40671278470074412, 1.343285922954075007, -3.873819829599202791 ) ) ;
#27005 = TOROIDAL_SURFACE ( 'NONE', #19951, 2.525000000001608846, 0.1000000000000000056 ) ;
#27006 = CIRCLE ( 'NONE', #4751, 2.000000000000000000 ) ;
#27007 = CARTESIAN_POINT ( 'NONE',  ( 15.90468948301723273, -4.892019442464182077, -2.306425897666045000 ) ) ;
#27008 = EDGE_CURVE ( 'NONE', #29991, #91, #28433, .T. ) ;
#27009 = CARTESIAN_POINT ( 'NONE',  ( 51.36283714269054457, -1.001673184507024805, 1.284520656909109659 ) ) ;
#27010 = EDGE_CURVE ( 'NONE', #29446, #3131, #14546, .T. ) ;
#27011 = VERTEX_POINT ( 'NONE', #7991 ) ;
#27012 = EDGE_CURVE ( 'NONE', #5143, #24008, #13841, .T. ) ;
#27013 = CARTESIAN_POINT ( 'NONE',  ( -37.18272003341173360, -24.59258869922088309, -3.011723503324820852E-15 ) ) ;
#27014 = CARTESIAN_POINT ( 'NONE',  ( 54.33851379069789544, 5.996232874381098199, 2.046523307115193369 ) ) ;
#27015 = VERTEX_POINT ( 'NONE', #12722 ) ;
#27016 = DIRECTION ( 'NONE',  ( 1.000000000000000000, 3.054025858079668409E-16, -2.042474015755241579E-16 ) ) ;
#27017 = ORIENTED_EDGE ( 'NONE', *, *, #1351, .F. ) ;
#27018 = CARTESIAN_POINT ( 'NONE',  ( 15.56274145962646926, 1.026563698233153632, -5.312790900508132630 ) ) ;
#27019 = CONICAL_SURFACE ( 'NONE', #13357, 1.600000000000000533, 0.7853981633974497223 ) ;
#27020 = CARTESIAN_POINT ( 'NONE',  ( -36.11780688638071268, -5.377732434016947671, 0.5657657146878161125 ) ) ;
#27022 = CARTESIAN_POINT ( 'NONE',  ( 58.45000000000001705, 0.8156862745098041323, -2.468735688885368873 ) ) ;
#27021 = DIRECTION ( 'NONE',  ( 0.000000000000000000, 0.000000000000000000, 1.000000000000000000 ) ) ;
#27023 = EDGE_LOOP ( 'NONE', ( #22074, #24490, #13699, #27573, #8114, #7779 ) ) ;
#27024 = DIRECTION ( 'NONE',  ( 1.000000000000000000, 1.047444401652940007E-14, 0.000000000000000000 ) ) ;
#27025 = CARTESIAN_POINT ( 'NONE',  ( 51.80000000000001847, 2.428612866367529932E-14, -1.808587333520743709E-13 ) ) ;
#27026 = ORIENTED_EDGE ( 'NONE', *, *, #26434, .F. ) ;
#27028 = CARTESIAN_POINT ( 'NONE',  ( -60.59999999999997300, -2.426837276046140079, -1.064406330116907329 ) ) ;
#27027 = DIRECTION ( 'NONE',  ( 1.000000000000000000, 3.054025858079668409E-16, -2.042474015755241579E-16 ) ) ;
#27029 = FACE_OUTER_BOUND ( 'NONE', #5028, .T. ) ;
#27030 = CARTESIAN_POINT ( 'NONE',  ( -60.06249999999996447, -3.238593381231840596, -2.874284765127020247 ) ) ;
#27031 = FACE_OUTER_BOUND ( 'NONE', #8497, .T. ) ;
#27032 = CARTESIAN_POINT ( 'NONE',  ( -55.37499999999997868, 2.489203624310592389, -2.804704140674917134 ) ) ;
#27033 = CARTESIAN_POINT ( 'NONE',  ( -54.49999999999995737, -3.717069605117153230, -0.3187059169208771303 ) ) ;
#27034 = CARTESIAN_POINT ( 'NONE',  ( -59.69999999999994600, 0.04532186801287400868, -3.495089302298031608 ) ) ;
#27035 = SPHERICAL_SURFACE ( 'NONE', #25490, 0.05000000000000000278 ) ;
#27036 = CARTESIAN_POINT ( 'NONE',  ( 15.97944027357902108, -0.5584590966806823875, 5.380195666604553395 ) ) ;
#27037 = ADVANCED_FACE ( 'NONE', ( #7530, #29215 ), #17190, .T. ) ;
#27039 = ORIENTED_EDGE ( 'NONE', *, *, #14792, .T. ) ;
#27038 = AXIS2_PLACEMENT_3D ( 'NONE', #22398, #2923, #12564 ) ;
#27040 = EDGE_CURVE ( 'NONE', #31257, #8227, #30237, .T. ) ;
#27041 = CARTESIAN_POINT ( 'NONE',  ( 15.61033468494288101, -3.560621078037094378, 4.077054076718838793 ) ) ;
#27042 = AXIS2_PLACEMENT_3D ( 'NONE', #9255, #21454, #68 ) ;
#27043 = DIRECTION ( 'NONE',  ( 0.000000000000000000, 1.000000000000000000, -0.000000000000000000 ) ) ;
#27044 = CIRCLE ( 'NONE', #11899, 4.349999999999997868 ) ;
#27045 = CARTESIAN_POINT ( 'NONE',  ( -59.45343688171008267, 3.370349218368761779, -1.096185326745346078 ) ) ;
#27046 = EDGE_CURVE ( 'NONE', #9856, #23389, #17806, .T. ) ;
#27047 = EDGE_CURVE ( 'NONE', #9761, #22848, #12440, .T. ) ;
#27048 = CARTESIAN_POINT ( 'NONE',  ( 58.64999999999999858, 1.972190280208564683, -0.1053114364790997820 ) ) ;
#27050 = CARTESIAN_POINT ( 'NONE',  ( 30.02700392305997212, 6.560679691584609508, 1.424999999999895239 ) ) ;
#27049 = DIRECTION ( 'NONE',  ( 1.000000000000000000, 1.047444401652940007E-14, 0.000000000000000000 ) ) ;
#27051 = VERTEX_POINT ( 'NONE', #22102 ) ;
#27052 = DIRECTION ( 'NONE',  ( 1.000000000000000000, 0.000000000000000000, -1.047444401652940007E-14 ) ) ;
#27053 = ORIENTED_EDGE ( 'NONE', *, *, #16399, .F. ) ;
#27054 = DIRECTION ( 'NONE',  ( 0.000000000000000000, -1.000000000000000000, -3.491481338843133355E-15 ) ) ;
#27056 = CARTESIAN_POINT ( 'NONE',  ( -54.49999999999997868, 5.725223786013876262E-16, -4.650000000000000355 ) ) ;
#27055 = CARTESIAN_POINT ( 'NONE',  ( -54.48976431536610932, -2.364211421526874357, -2.673742973752935903 ) ) ;
#27057 = CARTESIAN_POINT ( 'NONE',  ( 58.45000000000001705, 0.000000000000000000, 0.000000000000000000 ) ) ;
#27058 = ORIENTED_EDGE ( 'NONE', *, *, #25600, .T. ) ;
#27059 = AXIS2_PLACEMENT_3D ( 'NONE', #1768, #26170, #21433 ) ;
#27060 = ORIENTED_EDGE ( 'NONE', *, *, #6652, .F. ) ;
#27061 = CARTESIAN_POINT ( 'NONE',  ( -59.20655989232412963, 1.962990915244715806, 3.399999999999800071 ) ) ;
#27062 = CIRCLE ( 'NONE', #27557, 4.000000000000022204 ) ;
#27063 = CARTESIAN_POINT ( 'NONE',  ( 33.47623932017462778, 5.377732432866649148, -0.5657657256215208319 ) ) ;
#27064 = VERTEX_POINT ( 'NONE', #24607 ) ;
#27065 = CYLINDRICAL_SURFACE ( 'NONE', #2885, 0.1000000000000000472 ) ;
#27066 = CARTESIAN_POINT ( 'NONE',  ( -44.49999999999997868, 0.000000000000000000, 4.299999999999998046 ) ) ;
#27067 = CARTESIAN_POINT ( 'NONE',  ( -36.11692583559979397, -5.377732435184391591, -0.5657657035909954280 ) ) ;
#27068 = ORIENTED_EDGE ( 'NONE', *, *, #9550, .T. ) ;
#27069 = CARTESIAN_POINT ( 'NONE',  ( 0.000000000000000000, 0.000000000000000000, 0.000000000000000000 ) ) ;
#27070 = CIRCLE ( 'NONE', #7379, 2.424999999999998934 ) ;
#27071 = DIRECTION ( 'NONE',  ( 0.000000000000000000, 0.000000000000000000, -1.000000000000000000 ) ) ;
#27072 = SURFACE_STYLE_FILL_AREA ( #5089 ) ;
#27073 = AXIS2_PLACEMENT_3D ( 'NONE', #6236, #10823, #30296 ) ;
#27074 = ADVANCED_BREP_SHAPE_REPRESENTATION ( '', ( #15609, #9018 ), #3487 ) ;
#27075 = ADVANCED_FACE ( 'NONE', ( #544, #20024 ), #14791, .F. ) ;
#27076 = ORIENTED_EDGE ( 'NONE', *, *, #26550, .T. ) ;
#27077 = EDGE_CURVE ( 'NONE', #20165, #10936, #14973, .T. ) ;
#27078 = CARTESIAN_POINT ( 'NONE',  ( -59.94702994616205416, -2.078460969082657872, 3.599999999999778932 ) ) ;
#27079 = EDGE_CURVE ( 'NONE', #5843, #6314, #19869, .T. ) ;
#27080 = CARTESIAN_POINT ( 'NONE',  ( 50.36545094904631270, 1.397701019745849704, 3.854421226863028682 ) ) ;
#27081 = CARTESIAN_POINT ( 'NONE',  ( -44.49999999999997868, 0.2499224661714902207, 0.006225825468451445105 ) ) ;
#27082 = FACE_OUTER_BOUND ( 'NONE', #15242, .T. ) ;
#27083 = CARTESIAN_POINT ( 'NONE',  ( 51.80000000000001137, -4.144693941441892626, -1.074391609828098781 ) ) ;
#27084 = CARTESIAN_POINT ( 'NONE',  ( -58.70655989232410832, 1.962990915244761991, -3.400000000000191314 ) ) ;
#27086 = CARTESIAN_POINT ( 'NONE',  ( -35.85663232820584057, 3.426725943139506292, 3.937891353488775170 ) ) ;
#27085 = CARTESIAN_POINT ( 'NONE',  ( 51.12687253673781385, -0.9194130538815391551, -1.491219977510798600 ) ) ;
#27087 = VECTOR ( 'NONE', #24339, 1000.000000000000000 ) ;
#27088 = DIRECTION ( 'NONE',  ( -1.000000000000000000, 0.000000000000000000, 1.047444401652940007E-14 ) ) ;
#27089 = CARTESIAN_POINT ( 'NONE',  ( 48.47372026270296885, 1.373706569044511605, -3.853361913240786585 ) ) ;
#27090 = CIRCLE ( 'NONE', #14956, 1.949999999999999956 ) ;
#27092 = DIRECTION ( 'NONE',  ( 1.000000000000000000, 1.047444401652940007E-14, 0.000000000000000000 ) ) ;
#27091 = CARTESIAN_POINT ( 'NONE',  ( 54.49969840703174384, -0.002993017367578260958, -4.282759600741087525 ) ) ;
#27093 = EDGE_CURVE ( 'NONE', #14020, #12243, #18027, .T. ) ;
#27094 = ORIENTED_EDGE ( 'NONE', *, *, #19121, .T. ) ;
#27095 = TOROIDAL_SURFACE ( 'NONE', #7975, 1.239999999999999991, 0.01000000000000000021 ) ;
#27096 = CARTESIAN_POINT ( 'NONE',  ( -54.49999999999997868, 1.549999999999999600, -3.332135201338624952 ) ) ;
#27097 = VECTOR ( 'NONE', #27362, 1000.000000000000000 ) ;
#27098 = CARTESIAN_POINT ( 'NONE',  ( -62.09999999999997300, -2.693793069130350659, 0.1829724042179160792 ) ) ;
#27100 = CARTESIAN_POINT ( 'NONE',  ( 52.79530352569713614, 4.045408597361428882, 0.6880653358388769680 ) ) ;
#27099 = DIRECTION ( 'NONE',  ( 3.016910393003118404E-15, 0.000000000000000000, 1.000000000000000000 ) ) ;
#27101 = CARTESIAN_POINT ( 'NONE',  ( 47.00000000000002842, -3.994701997234459068, 2.069753729861246061 ) ) ;
#27102 = EDGE_LOOP ( 'NONE', ( #23349, #3702, #5223, #2502, #9140 ) ) ;
#27103 = CARTESIAN_POINT ( 'NONE',  ( -61.35505088056748235, -2.631273283024623488, 0.4666624523549950943 ) ) ;
#27104 = B_SPLINE_CURVE_WITH_KNOTS ( 'NONE', 3,
 ( #4574, #23896, #2188, #19166 ),
 .UNSPECIFIED., .F., .F.,
 ( 4, 4 ),
 ( 0.000000000000000000, 8.537476505502571882E-05 ),
 .UNSPECIFIED. ) ;
#27105 = AXIS2_PLACEMENT_3D ( 'NONE', #27745, #3531, #8424 ) ;
#27106 = ORIENTED_EDGE ( 'NONE', *, *, #6509, .T. ) ;
#27107 = CARTESIAN_POINT ( 'NONE',  ( 16.08093158123429944, -5.226279933021935165, 1.394410282272784407 ) ) ;
#27108 = B_SPLINE_CURVE_WITH_KNOTS ( 'NONE', 3,
 ( #15166, #19926, #29729, #27028 ),
 .UNSPECIFIED., .F., .F.,
 ( 4, 4 ),
 ( 0.000000000000000000, 1.854844919671800558E-05 ),
 .UNSPECIFIED. ) ;
#27109 = VERTEX_POINT ( 'NONE', #15105 ) ;
#27110 = ORIENTED_EDGE ( 'NONE', *, *, #2643, .T. ) ;
#27111 = CIRCLE ( 'NONE', #15988, 0.4576450603546999840 ) ;
#27112 = CARTESIAN_POINT ( 'NONE',  ( 15.74652664997094220, 5.205077242910887136, 1.471673150993847212 ) ) ;
#27113 = EDGE_LOOP ( 'NONE', ( #25081, #26915, #4144, #18644 ) ) ;
#27114 = SURFACE_SIDE_STYLE ('',( #24889 ) ) ;
#27115 = CARTESIAN_POINT ( 'NONE',  ( 48.00000000000002842, -4.387164041431067751, 1.383037119376590685 ) ) ;
#27116 = CARTESIAN_POINT ( 'NONE',  ( -58.82202994616202574, 2.078460969082674747, -3.600000000000199929 ) ) ;
#27117 = ORIENTED_EDGE ( 'NONE', *, *, #9841, .F. ) ;
#27118 = CIRCLE ( 'NONE', #2354, 0.1000000000000002554 ) ;
#27119 = DIRECTION ( 'NONE',  ( 1.000000000000000000, 0.000000000000000000, -1.047444401652940007E-14 ) ) ;
#27120 = ORIENTED_EDGE ( 'NONE', *, *, #17120, .T. ) ;
#27121 = DIRECTION ( 'NONE',  ( -1.000000000000000000, 0.000000000000000000, -3.491481338843153471E-15 ) ) ;
#27122 = COLOUR_RGB ( '', 0.08235294, 0.09019608, 0.10196078) ;
#27123 = CARTESIAN_POINT ( 'NONE',  ( 25.69798005929094131, 5.334073409755834660, 2.049999999999910116 ) ) ;
#27124 = ORIENTED_EDGE ( 'NONE', *, *, #28923, .F. ) ;
#27125 = AXIS2_PLACEMENT_3D ( 'NONE', #6425, #13688, #26040 ) ;
#27126 = EDGE_CURVE ( 'NONE', #14388, #9993, #22256, .T. ) ;
#27127 = CIRCLE ( 'NONE', #29623, 1.975000000000001865 ) ;
#27128 = CARTESIAN_POINT ( 'NONE',  ( 51.76135430833949158, -4.169908074913990070, -1.021033875312352457 ) ) ;
#27129 = CARTESIAN_POINT ( 'NONE',  ( 53.05250010753324830, 4.165967808473761913, -2.050000000000185008 ) ) ;
#27130 = CARTESIAN_POINT ( 'NONE',  ( -61.34999999999997300, -2.524557112582767715, -0.7907883100310012514 ) ) ;
#27131 = CARTESIAN_POINT ( 'NONE',  ( -67.99999999999995737, -0.6629581230868689667, 3.232721226309677842 ) ) ;
#27132 = CARTESIAN_POINT ( 'NONE',  ( 57.00319509709754584, -0.7184317838911207232, 2.441240553461111684 ) ) ;
#27134 = CARTESIAN_POINT ( 'NONE',  ( 58.65000045311413146, -1.008695754909590070, 1.580645149931285021 ) ) ;
#27133 = CARTESIAN_POINT ( 'NONE',  ( -35.98994760229914647, -3.426725948577701519, 3.937891352654260491 ) ) ;
#27135 = CIRCLE ( 'NONE', #1345, 4.199999999999993072 ) ;
#27136 = B_SPLINE_CURVE_WITH_KNOTS ( 'NONE', 3,
 ( #9316, #6948, #20883, #6472, #16612, #8999, #26254, #28150, #4562, #14209, #31154, #3934, #25778, #13574, #23412, #23262, #11209, #15267, #16764, #1026, #128, #16910 ),
 .UNSPECIFIED., .F., .F.,
 ( 4, 2, 2, 2, 2, 1, 2, 2, 1, 2, 2, 4 ),
 ( 0.000000000000000000, 0.1038980121052294342, 0.1558470181578441305, 0.2077960242104588684, 0.2337705272367660847, 0.2467577787499208308, 0.2483811851890659617, 0.2500045916282110925, 0.2532514045065013542, 0.2597450302630850971, 0.3116940363157674199, 0.4155920484211318988 ),
 .UNSPECIFIED. ) ;
#27137 = CIRCLE ( 'NONE', #13471, 0.09999999999999997780 ) ;
#27138 = CARTESIAN_POINT ( 'NONE',  ( 50.36545094904631270, -1.397701019745800854, -3.854421226863028238 ) ) ;
#27139 = CARTESIAN_POINT ( 'NONE',  ( 52.10742411006411601, 0.5153926522295700918, -1.803012591436477630 ) ) ;
#27140 = ADVANCED_FACE ( 'NONE', ( #29498 ), #5459, .T. ) ;
#27141 = CARTESIAN_POINT ( 'NONE',  ( 51.87416143049283335, 8.598705507415685290, -1.950000000000180256 ) ) ;
#27143 = CARTESIAN_POINT ( 'NONE',  ( -54.49999999999999289, 1.599999999999998090, 3.363870538531247067 ) ) ;
#27142 = CIRCLE ( 'NONE', #9953, 0.7375000000000040412 ) ;
#27144 = VERTEX_POINT ( 'NONE', #10349 ) ;
#27145 = CIRCLE ( 'NONE', #13479, 0.05000000000000009298 ) ;
#27146 = CIRCLE ( 'NONE', #31124, 2.525000000000001243 ) ;
#27147 = ORIENTED_EDGE ( 'NONE', *, *, #12813, .F. ) ;
#27148 = ORIENTED_EDGE ( 'NONE', *, *, #11563, .F. ) ;
#27149 = AXIS2_PLACEMENT_3D ( 'NONE', #15873, #20659, #27762 ) ;
#27150 = AXIS2_PLACEMENT_3D ( 'NONE', #15410, #25057, #24445 ) ;
#27151 =( BOUNDED_SURFACE ( )  B_SPLINE_SURFACE ( 3, 2, ( 
 ( #23270, #27381, #5691 ),
 ( #15342, #3314, #22659 ),
 ( #10605, #8222, #4095 ),
 ( #23578, #21223, #26415 ),
 ( #2033, #13733, #21054 ),
 ( #25938, #2182, #23421 ),
 ( #16771, #23741, #18676 ),
 ( #1881, #9173, #28326 ),
 ( #26262, #30520, #20890 ),
 ( #9005, #1701, #4569 ) ),
 .UNSPECIFIED., .F., .F., .F. ) 
 B_SPLINE_SURFACE_WITH_KNOTS ( ( 4, 2, 2, 2, 4 ),
 ( 3, 3 ),
 ( 0.0001706658715701448250, 0.0002229276920781092194, 0.0002751895125860735866, 0.0003274513330940380081, 0.0003797131536020023753 ),
 ( 0.000000000000000000, 1.000000000000000000 ),
 .UNSPECIFIED. ) 
 GEOMETRIC_REPRESENTATION_ITEM ( )  RATIONAL_B_SPLINE_SURFACE ( (
 ( 1.000000000000000000, 0.7071067811873470443, 1.000000000000000000),
 ( 1.000000000000000000, 0.7375607040708359596, 1.000000000000000000),
 ( 1.000000000000000000, 0.7730431127426509175, 1.000000000000000000),
 ( 1.000000000000000000, 0.8321012486970587041, 1.000000000000000000),
 ( 1.000000000000000000, 0.8541932017381176356, 1.000000000000000000),
 ( 1.000000000000000000, 0.8545723906027663519, 1.000000000000000000),
 ( 1.000000000000000000, 0.8327032135020736581, 1.000000000000000000),
 ( 1.000000000000000000, 0.7734559727054440836, 1.000000000000000000),
 ( 1.000000000000000000, 0.7377766653990520673, 1.000000000000000000),
 ( 1.000000000000000000, 0.7071067811865519026, 1.000000000000000000) ) ) 
 REPRESENTATION_ITEM ( '' )  SURFACE ( )  );
#27152 = DIRECTION ( 'NONE',  ( 0.000000000000000000, 0.000000000000000000, 1.000000000000000000 ) ) ;
#27153 = CARTESIAN_POINT ( 'NONE',  ( -57.36042740578360366, 3.725040285533370632, -1.239922660687675871 ) ) ;
#27155 = CARTESIAN_POINT ( 'NONE',  ( 50.59602332238209499, 0.1408342061609078322, 1.212874140286674063 ) ) ;
#27154 = CARTESIAN_POINT ( 'NONE',  ( 16.10660252424455763, 5.231589534716049705, 1.397536681175259199 ) ) ;
#27156 = ORIENTED_EDGE ( 'NONE', *, *, #4375, .F. ) ;
#27157 = EDGE_LOOP ( 'NONE', ( #9645, #10541, #14504, #8567, #14589, #27930 ) ) ;
#27158 = CARTESIAN_POINT ( 'NONE',  ( 51.52173077008821167, -4.267091652301652438, -1.720255306494824055 ) ) ;
#27159 = ORIENTED_EDGE ( 'NONE', *, *, #2975, .T. ) ;
#27160 = CYLINDRICAL_SURFACE ( 'NONE', #24664, 3.399999999999999911 ) ;
#27161 = ORIENTED_EDGE ( 'NONE', *, *, #22427, .F. ) ;
#27162 = CARTESIAN_POINT ( 'NONE',  ( 33.40812713680993085, 8.122903765861718028, -2.049999999999987832 ) ) ;
#27163 = LINE ( 'NONE', #21965, #10627 ) ;
#27164 = DIRECTION ( 'NONE',  ( 0.000000000000000000, -0.2008964009354143876, 0.9796124928211140670 ) ) ;
#27165 = EDGE_LOOP ( 'NONE', ( #9295, #30052, #19613, #9695 ) ) ;
#27166 = AXIS2_PLACEMENT_3D ( 'NONE', #18054, #10900, #27698 ) ;
#27167 = ADVANCED_FACE ( 'NONE', ( #26693 ), #29667, .F. ) ;
#27168 = AXIS2_PLACEMENT_3D ( 'NONE', #24278, #7642, #2591 ) ;
#27169 = CARTESIAN_POINT ( 'NONE',  ( 15.61552784268253546, -5.277544294472352071, -1.204650266290682170 ) ) ;
#27170 = CARTESIAN_POINT ( 'NONE',  ( -60.70655989232412963, 1.962990915244722245, 3.399999999999792077 ) ) ;
#27171 = CARTESIAN_POINT ( 'NONE',  ( 53.31611809544273939, 8.197428291949847790, -2.050000000000185452 ) ) ;
#27172 = CARTESIAN_POINT ( 'NONE',  ( 58.66107449606978008, 1.802323084877999859, 0.5180360531268706215 ) ) ;
#27173 = CIRCLE ( 'NONE', #24639, 0.09999999999999986677 ) ;
#27174 = DIRECTION ( 'NONE',  ( 0.000000000000000000, 0.000000000000000000, 1.000000000000000000 ) ) ;
#27175 = AXIS2_PLACEMENT_3D ( 'NONE', #14435, #5243, #14893 ) ;
#27176 = CARTESIAN_POINT ( 'NONE',  ( 58.65000000000002700, -0.8495817349395312634, -1.671477153794241666 ) ) ;
#27177 = CARTESIAN_POINT ( 'NONE',  ( 50.25000000000000711, 0.8897917884437445135, 1.791164585743606041 ) ) ;
#27178 = FACE_OUTER_BOUND ( 'NONE', #6812, .T. ) ;
#27179 = DIRECTION ( 'NONE',  ( 1.000000000000000000, 0.000000000000000000, -0.000000000000000000 ) ) ;
#27180 = ADVANCED_FACE ( 'NONE', ( #4990 ), #14646, .T. ) ;
#27181 = CARTESIAN_POINT ( 'NONE',  ( 50.95599726996785961, -0.9532299437226279260, 1.316046228059489120 ) ) ;
#27182 = EDGE_LOOP ( 'NONE', ( #35, #8339, #6869, #2890 ) ) ;
#27183 = CIRCLE ( 'NONE', #21130, 1.000000000000000000 ) ;
#27184 = CARTESIAN_POINT ( 'NONE',  ( -54.49999999999997868, 0.000000000000000000, 2.168404344971008868E-14 ) ) ;
#27185 = CARTESIAN_POINT ( 'NONE',  ( -36.58361892165925155, -3.265074799938336270, -4.311675893544455462 ) ) ;
#27186 = CARTESIAN_POINT ( 'NONE',  ( 54.40373534988020765, 5.983016911212706290, -1.963089969304966820 ) ) ;
#27187 = ORIENTED_EDGE ( 'NONE', *, *, #15658, .T. ) ;
#27188 = CARTESIAN_POINT ( 'NONE',  ( -60.64999999999998437, -2.511038422848939078, 0.9923134781793048198 ) ) ;
#27189 =( BOUNDED_CURVE ( )  B_SPLINE_CURVE ( 2, ( #4606, #24392, #14411, #7295, #24245, #26913, #2850, #21735, #28840 ),
 .UNSPECIFIED., .F., .T. ) 
 B_SPLINE_CURVE_WITH_KNOTS ( ( 3, 2, 2, 2, 3 ),
 ( 0.4722222222222222099, 0.4814814814814814548, 0.5000000000000000000, 0.5185185185185184897, 0.5277777777777777901 ),
 .UNSPECIFIED. ) 
 CURVE ( )  GEOMETRIC_REPRESENTATION_ITEM ( )  RATIONAL_B_SPLINE_CURVE ( ( 0.9330127018922194093, 0.9330127018922194093, 1.000000000000000000, 0.8660254037844387076, 1.000000000000000000, 0.8660254037844387076, 1.000000000000000000, 0.9330127018922194093, 0.9330127018922194093 ) ) 
 REPRESENTATION_ITEM ( '' )  );
#27190 = CIRCLE ( 'NONE', #10007, 4.050000000000000711 ) ;
#27191 = ORIENTED_EDGE ( 'NONE', *, *, #28420, .F. ) ;
#27192 = CARTESIAN_POINT ( 'NONE',  ( 53.53640187423193453, 5.215699251213354870, 1.635615235160198466 ) ) ;
#27193 = DIRECTION ( 'NONE',  ( 1.000000000000000000, 1.047444401652940007E-14, 0.000000000000000000 ) ) ;
#27195 = FACE_OUTER_BOUND ( 'NONE', #3189, .T. ) ;
#27194 = DIRECTION ( 'NONE',  ( -1.047444401652940007E-14, 0.000000000000000000, -1.000000000000000000 ) ) ;
#27196 = ADVANCED_FACE ( 'NONE', ( #8449 ), #12871, .T. ) ;
#27197 = VERTEX_POINT ( 'NONE', #27603 ) ;
#27198 = CARTESIAN_POINT ( 'NONE',  ( 60.99999998418545033, -0.8156891353810385992, -1.406736638527428029 ) ) ;
#27199 = CARTESIAN_POINT ( 'NONE',  ( 57.05000000000001847, -0.7500000000000000000, -1.778341924377873751 ) ) ;
#27200 = ORIENTED_EDGE ( 'NONE', *, *, #5571, .F. ) ;
#27202 = PLANE ( 'NONE',  #31238 ) ;
#27201 = LINE ( 'NONE', #5510, #12060 ) ;
#27203 = CARTESIAN_POINT ( 'NONE',  ( 51.80000048029783244, 4.021162535479849254, 2.019963026417355589 ) ) ;
#27204 = CARTESIAN_POINT ( 'NONE',  ( -57.12499999999997158, -3.673546848079173976, -0.7533615035078062849 ) ) ;
#27205 = DIRECTION ( 'NONE',  ( 1.189524669241239105E-14, 0.000000000000000000, 1.000000000000000000 ) ) ;
#27206 = EDGE_CURVE ( 'NONE', #31281, #2592, #14757, .T. ) ;
#27207 = CARTESIAN_POINT ( 'NONE',  ( -55.06249999999997158, -0.7533615035078029543, 3.673546848079176197 ) ) ;
#27208 = CARTESIAN_POINT ( 'NONE',  ( -59.30000000000042348, -2.541725022351402963, -2.757196748647571027 ) ) ;
#27209 = FACE_OUTER_BOUND ( 'NONE', #22059, .T. ) ;
#27210 = EDGE_CURVE ( 'NONE', #12796, #13195, #14489, .T. ) ;
#27211 = CARTESIAN_POINT ( 'NONE',  ( -62.09999999999997300, -2.737380368259866525, 0.2631615932906978261 ) ) ;
#27212 = ORIENTED_EDGE ( 'NONE', *, *, #18757, .F. ) ;
#27213 = AXIS2_PLACEMENT_3D ( 'NONE', #30945, #7199, #9590 ) ;
#27214 = CARTESIAN_POINT ( 'NONE',  ( 15.29449157529454695, -2.734387802834054693, 4.440904455451909705 ) ) ;
#27215 = LINE ( 'NONE', #27512, #23064 ) ;
#27216 = EDGE_CURVE ( 'NONE', #20056, #19660, #27767, .T. ) ;
#27217 = CARTESIAN_POINT ( 'NONE',  ( 53.88560433715219489, 6.996395185205533274, -1.802990336641044244 ) ) ;
#27218 = CARTESIAN_POINT ( 'NONE',  ( -36.63359589171280106, 4.847650360853540619, -2.396424556482824375 ) ) ;
#27219 = DIRECTION ( 'NONE',  ( -5.046468293750706671E-15, 0.000000000000000000, -1.000000000000000000 ) ) ;
#27220 = CARTESIAN_POINT ( 'NONE',  ( 28.65063797331448825, 5.832638074306361275, 2.049999999999899902 ) ) ;
#27221 = ORIENTED_EDGE ( 'NONE', *, *, #9451, .F. ) ;
#27222 = DIRECTION ( 'NONE',  ( 0.000000000000000000, -1.000000000000000000, -4.336808689942025625E-15 ) ) ;
#27223 = ORIENTED_EDGE ( 'NONE', *, *, #22127, .T. ) ;
#27224 = UNCERTAINTY_MEASURE_WITH_UNIT (LENGTH_MEASURE( 1.000000000000000082E-05 ), #21276, 'distance_accuracy_value', 'NONE');
#27225 = CARTESIAN_POINT ( 'NONE',  ( -62.34999999999997300, -2.749147127886318653, -0.06848408015297867413 ) ) ;
#27227 = DIRECTION ( 'NONE',  ( 0.000000000000000000, -1.000000000000000000, 0.000000000000000000 ) ) ;
#27226 = CARTESIAN_POINT ( 'NONE',  ( -54.48711142618073211, -2.373575576312949131, -2.672219526802753098 ) ) ;
#27228 = EDGE_CURVE ( 'NONE', #22535, #22261, #2839, .T. ) ;
#27229 = ORIENTED_EDGE ( 'NONE', *, *, #18602, .T. ) ;
#27230 = AXIS2_PLACEMENT_3D ( 'NONE', #21259, #30891, #6995 ) ;
#27231 = ORIENTED_EDGE ( 'NONE', *, *, #2155, .F. ) ;
#27232 = CARTESIAN_POINT ( 'NONE',  ( 51.21562071718021514, -0.9844478935104048478, 1.555267182539685766 ) ) ;
#27233 = CARTESIAN_POINT ( 'NONE',  ( -67.98046642889043767, -0.6631150920522017600, 3.233486639521210293 ) ) ;
#27234 = ORIENTED_EDGE ( 'NONE', *, *, #6121, .T. ) ;
#27235 = EDGE_CURVE ( 'NONE', #468, #25169, #23091, .T. ) ;
#27237 = DIRECTION ( 'NONE',  ( 1.000000000000000000, 3.053848253006669023E-16, -2.042510438544995415E-16 ) ) ;
#27236 = CARTESIAN_POINT ( 'NONE',  ( -57.94702994616203995, 4.156921938165313080, -1.906555437768272735E-13 ) ) ;
#27238 = CARTESIAN_POINT ( 'NONE',  ( 50.34137136386934230, 1.344608935533184946, 3.858631320448700386 ) ) ;
#27239 = DIRECTION ( 'NONE',  ( 0.000000000000000000, -1.000000000000000000, 0.000000000000000000 ) ) ;
#27240 = DIRECTION ( 'NONE',  ( 1.000000000000000000, 0.000000000000000000, 0.000000000000000000 ) ) ;
#27241 = DIRECTION ( 'NONE',  ( -1.000000000000000000, -0.000000000000000000, -0.000000000000000000 ) ) ;
#27242 = EDGE_CURVE ( 'NONE', #24297, #26503, #838, .T. ) ;
#27243 = EDGE_CURVE ( 'NONE', #10684, #12730, #1822, .T. ) ;
#27244 = ORIENTED_EDGE ( 'NONE', *, *, #19445, .T. ) ;
#27245 = CARTESIAN_POINT ( 'NONE',  ( -58.82202994616202574, 2.078460969082674747, -3.600000000000199929 ) ) ;
#27246 = CARTESIAN_POINT ( 'NONE',  ( 52.98658227084825256, 8.418175601153722099, -2.050000000000184563 ) ) ;
#27247 = CARTESIAN_POINT ( 'NONE',  ( 48.29999997257028355, -0.7904052113206601060, -4.025738854575411807 ) ) ;
#27248 = CARTESIAN_POINT ( 'NONE',  ( 15.74652664997094575, 0.2088129849845392905, 5.405094643512426522 ) ) ;
#27249 = CARTESIAN_POINT ( 'NONE',  ( 51.67583320948680381, -3.859603212985638354, 1.644059474114338615 ) ) ;
#27250 =( GEOMETRIC_REPRESENTATION_CONTEXT ( 3 ) GLOBAL_UNCERTAINTY_ASSIGNED_CONTEXT ( ( #18052 ) ) GLOBAL_UNIT_ASSIGNED_CONTEXT ( ( #15208, #3172, #17755 ) ) REPRESENTATION_CONTEXT ( 'NONE', 'WORKASPACE' ) );
#27251 = DIRECTION ( 'NONE',  ( 0.000000000000000000, 0.9996898646859344595, 0.02490330187381124133 ) ) ;
#27252 = AXIS2_PLACEMENT_3D ( 'NONE', #16846, #12092, #18756 ) ;
#27254 = CARTESIAN_POINT ( 'NONE',  ( 58.50000000000001421, 0.8000000000000000444, -2.421260002560649660 ) ) ;
#27253 = CARTESIAN_POINT ( 'NONE',  ( -61.83175433005612120, -2.679521002368077998, 0.3417824691599675724 ) ) ;
#27255 = CARTESIAN_POINT ( 'NONE',  ( -62.08167832910348238, -2.517763198270825065, 0.1910326606448936038 ) ) ;
#27256 = CARTESIAN_POINT ( 'NONE',  ( 15.18463186935387377, -4.018128179617967533, 3.618665901676295427 ) ) ;
#27258 = DIRECTION ( 'NONE',  ( 0.000000000000000000, -2.168404344971008128E-16, -1.000000000000000000 ) ) ;
#27257 = DIRECTION ( 'NONE',  ( 0.000000000000000000, 0.000000000000000000, 1.000000000000000000 ) ) ;
#27259 = ORIENTED_EDGE ( 'NONE', *, *, #5571, .T. ) ;
#27260 = CARTESIAN_POINT ( 'NONE',  ( 50.40000000000001279, -0.7707709757764150682, -3.938803467580344719 ) ) ;
#27261 = DIRECTION ( 'NONE',  ( 0.000000000000000000, -1.000000000000000000, -4.336808689942015369E-15 ) ) ;
#27262 = CIRCLE ( 'NONE', #1982, 2.750000000000000444 ) ;
#27264 = CARTESIAN_POINT ( 'NONE',  ( -44.59999999999997300, 8.366749974758271452E-15, -1.593320673368357066E-13 ) ) ;
#27263 = CARTESIAN_POINT ( 'NONE',  ( 15.44259799936806132, 3.232943006030417621, -4.078682900256741739 ) ) ;
#27265 = CARTESIAN_POINT ( 'NONE',  ( 47.88166157169970916, -4.387164033828454102, 1.383037143493017984 ) ) ;
#27266 = EDGE_CURVE ( 'NONE', #16594, #16545, #29134, .T. ) ;
#27267 = ORIENTED_EDGE ( 'NONE', *, *, #25179, .T. ) ;
#27268 = FACE_OUTER_BOUND ( 'NONE', #5590, .T. ) ;
#27269 = LINE ( 'NONE', #5586, #26490 ) ;
#27270 = EDGE_CURVE ( 'NONE', #22178, #4534, #17019, .T. ) ;
#27271 = ORIENTED_EDGE ( 'NONE', *, *, #427, .F. ) ;
#27272 = EDGE_CURVE ( 'NONE', #10142, #20943, #9927, .T. ) ;
#27273 = DIRECTION ( 'NONE',  ( 0.000000000000000000, 0.000000000000000000, 1.000000000000000000 ) ) ;
#27274 = ORIENTED_EDGE ( 'NONE', *, *, #23992, .F. ) ;
#27275 = ORIENTED_EDGE ( 'NONE', *, *, #4003, .F. ) ;
#27276 = CARTESIAN_POINT ( 'NONE',  ( -74.39999999999997726, -2.588216748940040213E-15, 4.710014593512140639E-15 ) ) ;
#27277 = VERTEX_POINT ( 'NONE', #8739 ) ;
#27278 = DIRECTION ( 'NONE',  ( 0.000000000000000000, -0.9996898646859344595, -0.02490330187381124480 ) ) ;
#27279 = CIRCLE ( 'NONE', #25766, 4.835355339059328017 ) ;
#27280 = CARTESIAN_POINT ( 'NONE',  ( -55.26905989232413674, -2.944486372867088697, 1.699999999999792344 ) ) ;
#27281 = ORIENTED_EDGE ( 'NONE', *, *, #13473, .T. ) ;
#27282 = DIRECTION ( 'NONE',  ( -1.000000000000000000, 1.219044193948983948E-29, -3.491481338843133355E-15 ) ) ;
#27283 = ORIENTED_EDGE ( 'NONE', *, *, #21938, .F. ) ;
#27284 = DIRECTION ( 'NONE',  ( 1.000000000000000000, 1.047444401652940007E-14, 0.000000000000000000 ) ) ;
#27285 = CARTESIAN_POINT ( 'NONE',  ( 24.17629218419978798, 5.599093920765381149, 1.949999999999914468 ) ) ;
#27286 = ORIENTED_EDGE ( 'NONE', *, *, #16399, .T. ) ;
#27287 = VECTOR ( 'NONE', #1680, 1000.000000000000000 ) ;
#27288 = DIRECTION ( 'NONE',  ( -0.7313537016191670181, -0.6819983600625022513, 2.468850131082252327E-15 ) ) ;
#27289 = CARTESIAN_POINT ( 'NONE',  ( 60.75000000000002842, 0.5000000000006363798, 1.554802467931445165 ) ) ;
#27290 = CARTESIAN_POINT ( 'NONE',  ( 50.25000000000001421, 0.5380862305904824394, 2.008165151419250449 ) ) ;
#27291 = DIRECTION ( 'NONE',  ( 1.000000000000000000, 0.000000000000000000, 0.000000000000000000 ) ) ;
#27292 = CARTESIAN_POINT ( 'NONE',  ( 51.24366546300165481, 0.9939151496001219499, 1.410979063385805032 ) ) ;
#27294 = DIRECTION ( 'NONE',  ( 1.000000000000000000, 0.000000000000000000, -4.738179285253040686E-16 ) ) ;
#27293 = DIRECTION ( 'NONE',  ( 0.000000000000000000, 0.000000000000000000, 1.000000000000000000 ) ) ;
#27295 = DIRECTION ( 'NONE',  ( 1.000000000000000000, -0.000000000000000000, -1.047444401652940007E-14 ) ) ;
#27296 = DIRECTION ( 'NONE',  ( 1.000000000000000000, -0.000000000000000000, -0.000000000000000000 ) ) ;
#27297 = CIRCLE ( 'NONE', #17707, 0.1000000000000001443 ) ;
#27298 = CARTESIAN_POINT ( 'NONE',  ( 51.87416143049283335, 8.598705507415687066, -1.976179938780094680 ) ) ;
#27299 = AXIS2_PLACEMENT_3D ( 'NONE', #21904, #19675, #2575 ) ;
#27300 = CARTESIAN_POINT ( 'NONE',  ( 48.43454905095371998, -1.397701019745800854, 3.854421226863028238 ) ) ;
#27301 = VERTEX_POINT ( 'NONE', #20806 ) ;
#27302 = CARTESIAN_POINT ( 'NONE',  ( -59.69557399992023505, -2.421670674729428985, -1.235983257124811274 ) ) ;
#27303 = ADVANCED_FACE ( 'NONE', ( #20663 ), #9440, .F. ) ;
#27304 = TOROIDAL_SURFACE ( 'NONE', #523, 2.824999999999998845, 0.05000000000000000278 ) ;
#27305 = EDGE_CURVE ( 'NONE', #3096, #18872, #6378, .T. ) ;
#27306 = ORIENTED_EDGE ( 'NONE', *, *, #16330, .F. ) ;
#27307 = ORIENTED_EDGE ( 'NONE', *, *, #12120, .T. ) ;
#27308 = EDGE_CURVE ( 'NONE', #16066, #18954, #3858, .T. ) ;
#27309 = CARTESIAN_POINT ( 'NONE',  ( -62.07031753968892218, -2.504221380502570593, -0.3232671695957713975 ) ) ;
#27310 = CARTESIAN_POINT ( 'NONE',  ( -58.36042740578360366, -2.936324665650201116, -2.606018187048497747 ) ) ;
#27312 = CARTESIAN_POINT ( 'NONE',  ( -61.37941297909985394, -2.603941716553896946, 0.6968202940837837644 ) ) ;
#27311 = CARTESIAN_POINT ( 'NONE',  ( -35.85663232820584057, -4.804073783693461941, 2.042134687550347216 ) ) ;
#27313 = ORIENTED_EDGE ( 'NONE', *, *, #3436, .F. ) ;
#27314 = ORIENTED_EDGE ( 'NONE', *, *, #476, .T. ) ;
#27315 = CARTESIAN_POINT ( 'NONE',  ( 53.92227517398921322, 6.075005530725110958, -1.819853284099130386 ) ) ;
#27316 = ORIENTED_EDGE ( 'NONE', *, *, #13640, .T. ) ;
#27317 = CARTESIAN_POINT ( 'NONE',  ( 51.45655683570189609, 0.9591657938401607630, -1.468576096419531130 ) ) ;
#27318 = VERTEX_POINT ( 'NONE', #29977 ) ;
#27319 = CARTESIAN_POINT ( 'NONE',  ( 32.30803788440152857, 7.816246120666627384, -2.049999999999984723 ) ) ;
#27320 = CARTESIAN_POINT ( 'NONE',  ( -58.24999999999997158, 3.673546848079177085, 0.7533615035078238265 ) ) ;
#27321 = CARTESIAN_POINT ( 'NONE',  ( 48.00000000000002132, -3.908336260473453727, 1.238913909465751972 ) ) ;
#27322 = EDGE_CURVE ( 'NONE', #12623, #5273, #8288, .T. ) ;
#27323 = DIRECTION ( 'NONE',  ( 0.000000000000000000, -2.664535259100368992E-15, 1.000000000000000000 ) ) ;
#27324 = CARTESIAN_POINT ( 'NONE',  ( -57.01905989232412963, 2.944486372867092250, 1.699999999999808553 ) ) ;
#27325 = CARTESIAN_POINT ( 'NONE',  ( 53.60047708782973075, 7.640852521089409599, -2.050000000000185896 ) ) ;
#27326 = CARTESIAN_POINT ( 'NONE',  ( 51.80690729991166421, -4.271967808728815541, -0.9446991603439683916 ) ) ;
#27327 = CIRCLE ( 'NONE', #542, 0.1000000000000000472 ) ;
#27328 = CARTESIAN_POINT ( 'NONE',  ( -67.91948434493399134, 1.598692187574554335, 0.03982506530961366781 ) ) ;
#27329 = LINE ( 'NONE', #24796, #22088 ) ;
#27330 = DIRECTION ( 'NONE',  ( 0.000000000000000000, 0.8914544820238954337, -0.4531102586341524963 ) ) ;
#27331 = PRODUCT_DEFINITION ( 'UNKNOWN', '', #22751, #1238 ) ;
#27332 = CARTESIAN_POINT ( 'NONE',  ( -59.31739128601933686, -2.302762792303276296, 1.317912415714726393 ) ) ;
#27333 = CARTESIAN_POINT ( 'NONE',  ( -61.34138854390450035, -2.661151313430901943, 0.4599831919335348185 ) ) ;
#27334 =( BOUNDED_SURFACE ( )  B_SPLINE_SURFACE ( 2, 3, ( 
 ( #1204, #20552, #30183, #586, #10245, #19917, #27192, #5501, #15154, #24809, #6441, #25431, #23232, #28284, #8644, #14015, #6596, #23072 ),
 ( #4366, #23706, #13700, #4057, #28596, #30968, #11662, #15782, #3733, #30339, #1665, #8960, #30484, #30816, #13375, #25750, #18950, #23533 ),
 ( #1368, #1833, #8787, #11034, #13550, #1996, #25900, #6743, #21340, #18640, #1521, #16254, #16404, #11182, #11324, #6275, #21185, #20709 ),
 ( #28118, #4206, #13844, #30648, #11506, #20856, #21009, #18478, #18324, #23382, #27961, #9133, #18797, #16102, #28439, #26056, #9287, #15921 ),
 ( #3901, #25583, #24317, #7370, #4677, #16578, #14333, #14497, #2147, #19584, #24003, #2304, #12416, #16735, #29222, #28762, #7220, #12130 ) ),
 .UNSPECIFIED., .F., .F., .F. ) 
 B_SPLINE_SURFACE_WITH_KNOTS ( ( 3, 2, 3 ),
 ( 4, 2, 2, 2, 2, 2, 2, 2, 4 ),
 ( 0.000000000000000000, 1.000000000000000000, 1.010000000000000009 ),
 ( 1.413716694115406902, 1.826050729899067360, 2.238384765682727817, 2.650718801466387831, 3.063052837250048288, 3.475386873033708746, 3.887720908817368759, 4.300054944601029661, 4.712388980384689674 ),
 .UNSPECIFIED. ) 
 GEOMETRIC_REPRESENTATION_ITEM ( )  RATIONAL_B_SPLINE_SURFACE ( (
 ( 1.000000000000000000, 1.000000000000000000, 1.000000000000000000, 1.000000000000000000, 1.000000000000000000, 1.000000000000000000, 1.000000000000000000, 1.000000000000000000, 1.000000000000000000, 1.000000000000000000, 1.000000000000000000, 1.000000000000000000, 1.000000000000000000, 1.000000000000000000, 1.000000000000000000, 1.000000000000000000, 1.000000000000000000, 1.000000000000000000),
 ( 0.7071067811865476838, 0.7071067811865476838, 0.7071067811865473507, 0.7071067811865473507, 0.7071067811865476838, 0.7071067811865476838, 0.7071067811865476838, 0.7071067811865476838, 0.7071067811865473507, 0.7071067811865473507, 0.7071067811865476838, 0.7071067811865476838, 0.7071067811865480168, 0.7071067811865480168, 0.7071067811865450192, 0.7071067811865450192, 0.7071067811865467956, 0.7071067811865467956),
 ( 1.000000000000000000, 1.000000000000000000, 1.000000000000000000, 1.000000000000000000, 1.000000000000000000, 1.000000000000000000, 1.000000000000000000, 1.000000000000000000, 1.000000000000000000, 1.000000000000000000, 1.000000000000000000, 1.000000000000000000, 1.000000000000000000, 1.000000000000000000, 1.000000000000000000, 1.000000000000000000, 1.000000000000000000, 1.000000000000000000),
 ( 1.000000000000000000, 1.000000000000000000, 1.000000000000000000, 1.000000000000000000, 1.000000000000000000, 1.000000000000000000, 1.000000000000000000, 1.000000000000000000, 1.000000000000000000, 1.000000000000000000, 1.000000000000000000, 1.000000000000000000, 1.000000000000000000, 1.000000000000000000, 1.000000000000000000, 1.000000000000000000, 1.000000000000000000, 1.000000000000000000),
 ( 1.000000000000000000, 1.000000000000000000, 1.000000000000000000, 1.000000000000000000, 1.000000000000000000, 1.000000000000000000, 1.000000000000000000, 1.000000000000000000, 1.000000000000000000, 1.000000000000000000, 1.000000000000000000, 1.000000000000000000, 1.000000000000000000, 1.000000000000000000, 1.000000000000000000, 1.000000000000000000, 1.000000000000000000, 1.000000000000000000) ) ) 
 REPRESENTATION_ITEM ( '' )  SURFACE ( )  );
#27335 = EDGE_LOOP ( 'NONE', ( #11728, #7042, #9532, #27147 ) ) ;
#27336 = CARTESIAN_POINT ( 'NONE',  ( -59.29999999999997584, -2.208048483361063852, 2.585444235547710967 ) ) ;
#27337 = CARTESIAN_POINT ( 'NONE',  ( -36.31440869660545445, -3.012234853004159163, -4.239036759381638930 ) ) ;
#27338 = CARTESIAN_POINT ( 'NONE',  ( 54.27669070682345165, 6.362024491156814676, 2.049999999999809308 ) ) ;
#27339 = VERTEX_POINT ( 'NONE', #4158 ) ;
#27340 = EDGE_CURVE ( 'NONE', #7731, #8913, #27118, .T. ) ;
#27341 = CARTESIAN_POINT ( 'NONE',  ( 50.25000000000004263, -2.008165151418462191, -0.5380862305909229759 ) ) ;
#27342 = VERTEX_POINT ( 'NONE', #2252 ) ;
#27343 = ADVANCED_FACE ( 'NONE', ( #1616 ), #24101, .T. ) ;
#27344 = CARTESIAN_POINT ( 'NONE',  ( 51.70000000000002416, 4.174380580618757719, 1.932497546739255556 ) ) ;
#27345 = CARTESIAN_POINT ( 'NONE',  ( -36.43290890416664496, -5.277544294472357400, 1.204650266290678395 ) ) ;
#27346 = B_SPLINE_CURVE_WITH_KNOTS ( 'NONE', 3,
 ( #16722, #24303, #24153, #13998 ),
 .UNSPECIFIED., .F., .F.,
 ( 4, 4 ),
 ( 0.000000000000000000, 8.537476504122688803E-05 ),
 .UNSPECIFIED. ) ;
#27348 = CARTESIAN_POINT ( 'NONE',  ( 51.77061368361890459, -3.672971185000162730, -1.825899123715961414 ) ) ;
#27347 = CARTESIAN_POINT ( 'NONE',  ( 48.30000000000001847, -0.6462379109120514054, -4.048750000000023164 ) ) ;
#27349 = EDGE_LOOP ( 'NONE', ( #25587, #13056, #21733, #25823 ) ) ;
#27350 = DIRECTION ( 'NONE',  ( 0.000000000000000000, 0.000000000000000000, -1.000000000000000000 ) ) ;
#27351 = AXIS2_PLACEMENT_3D ( 'NONE', #25952, #11228, #13746 ) ;
#27352 = CARTESIAN_POINT ( 'NONE',  ( 57.00381193298470350, -0.7199075706197948232, -1.804244861858284255 ) ) ;
#27353 = EDGE_LOOP ( 'NONE', ( #23007, #1179, #11838, #6880, #9942 ) ) ;
#27355 = DIRECTION ( 'NONE',  ( 0.000000000000000000, 1.000000000000000000, 0.000000000000000000 ) ) ;
#27354 = CARTESIAN_POINT ( 'NONE',  ( 52.94611566430813809, 4.198287402864775864, 2.047134521670517682 ) ) ;
#27356 = DIRECTION ( 'NONE',  ( 0.000000000000000000, 0.000000000000000000, 1.000000000000000000 ) ) ;
#27357 = ORIENTED_EDGE ( 'NONE', *, *, #26969, .F. ) ;
#27358 = CARTESIAN_POINT ( 'NONE',  ( 52.20711756518983293, 0.5000000000005468959, 1.718465885608440491 ) ) ;
#27359 = CARTESIAN_POINT ( 'NONE',  ( 58.75000000000001421, 0.5000000000003640421, -1.863080903343440786 ) ) ;
#27360 = CARTESIAN_POINT ( 'NONE',  ( 58.75000000000000711, 1.760622601997809733, -0.8948927608024527247 ) ) ;
#27361 = ADVANCED_FACE ( 'NONE', ( #21293 ), #4630, .F. ) ;
#27362 = DIRECTION ( 'NONE',  ( 1.000000000000000000, 3.053848253006669023E-16, -2.042510438544995415E-16 ) ) ;
#27363 = DIRECTION ( 'NONE',  ( 0.000000000000000000, 6.217248937900896348E-15, 1.000000000000000000 ) ) ;
#27364 = CARTESIAN_POINT ( 'NONE',  ( -55.75952994616203995, 3.117691453623994580, -1.800000000000184563 ) ) ;
#27365 = ORIENTED_EDGE ( 'NONE', *, *, #3117, .F. ) ;
#27366 = AXIS2_PLACEMENT_3D ( 'NONE', #11064, #25623, #25785 ) ;
#27367 = CARTESIAN_POINT ( 'NONE',  ( 15.56274145962601629, 2.292272662152952112, 4.901537128432109647 ) ) ;
#27368 = CARTESIAN_POINT ( 'NONE',  ( -55.23542740578361077, 0.7887156198831712928, -3.845940847736172952 ) ) ;
#27369 =( BOUNDED_SURFACE ( )  B_SPLINE_SURFACE ( 3, 2, ( 
 ( #11084, #26282, #25806 ),
 ( #23603, #16313, #30721 ),
 ( #3957, #11568, #4262 ),
 ( #9343, #11392, #13907 ),
 ( #9026, #26119, #18378 ),
 ( #28663, #6979, #23136 ),
 ( #20765, #30874, #2054 ),
 ( #11717, #28185, #28014 ),
 ( #16644, #9193, #11232 ),
 ( #6801, #19012, #1904 ),
 ( #1721, #6650, #21244 ),
 ( #20908, #23437, #18855 ),
 ( #15985, #28497, #1424 ),
 ( #25647, #16463, #25957 ),
 ( #4435, #4588, #30540 ),
 ( #21077, #30390, #14083 ) ),
 .UNSPECIFIED., .F., .F., .T. ) 
 B_SPLINE_SURFACE_WITH_KNOTS ( ( 4, 2, 2, 2, 2, 2, 2, 4 ),
 ( 3, 3 ),
 ( 0.001780502285214230051, 0.002558945925323756823, 0.002753556835351138841, 0.002948167745378520426, 0.003337389565433284029, 0.003726611385488047632, 0.004115833205542811235, 0.004894276845652338441 ),
 ( 0.000000000000000000, 1.000000000000000000 ),
 .UNSPECIFIED. ) 
 GEOMETRIC_REPRESENTATION_ITEM ( )  RATIONAL_B_SPLINE_SURFACE ( (
 ( 1.000000000000000000, 0.9418517008537241608, 1.000000000000000000),
 ( 1.000000000000000000, 0.9417987965885392665, 1.000000000000000000),
 ( 1.000000000000000000, 0.9418198861733664273, 1.000000000000000000),
 ( 1.000000000000000000, 0.9434060303845691609, 1.000000000000000000),
 ( 1.000000000000000000, 0.9437939819947983588, 1.000000000000000000),
 ( 1.000000000000000000, 0.9445989566712983398, 1.000000000000000000),
 ( 1.000000000000000000, 0.9450169930049727718, 1.000000000000000000),
 ( 1.000000000000000000, 0.9461610507673836601, 1.000000000000000000),
 ( 1.000000000000000000, 0.9467217966425610642, 1.000000000000000000),
 ( 1.000000000000000000, 0.9467345476125937909, 1.000000000000000000),
 ( 1.000000000000000000, 0.9461964028053096998, 1.000000000000000000),
 ( 1.000000000000000000, 0.9446801822473712695, 1.000000000000000000),
 ( 1.000000000000000000, 0.9437582546537136574, 1.000000000000000000),
 ( 1.000000000000000000, 0.9418129560294529190, 1.000000000000000000),
 ( 1.000000000000000000, 0.9418016889778366707, 1.000000000000000000),
 ( 1.000000000000000000, 0.9418517008537241608, 1.000000000000000000) ) ) 
 REPRESENTATION_ITEM ( '' )  SURFACE ( )  );
#27370 = CARTESIAN_POINT ( 'NONE',  ( 68.00000000000000000, 0.7500000000000000000, -2.238246715074068582 ) ) ;
#27371 = CARTESIAN_POINT ( 'NONE',  ( -57.57202994616204705, -4.156921938165296204, -2.308488068846171547E-13 ) ) ;
#27372 = CARTESIAN_POINT ( 'NONE',  ( 33.47623932017462778, 2.199885893005997239, -4.939696249117661253 ) ) ;
#27373 = CARTESIAN_POINT ( 'NONE',  ( 48.45103168306561514, 1.383117500626982910, -3.859810431918025309 ) ) ;
#27374 = ORIENTED_EDGE ( 'NONE', *, *, #15150, .F. ) ;
#27375 = EDGE_CURVE ( 'NONE', #8120, #13995, #6695, .T. ) ;
#27376 = CARTESIAN_POINT ( 'NONE',  ( 58.75000000000002132, 6.153735859711025284E-13, 3.111507638930570854E-58 ) ) ;
#27377 = ORIENTED_EDGE ( 'NONE', *, *, #12889, .F. ) ;
#27378 = EDGE_CURVE ( 'NONE', #9785, #4498, #30136, .T. ) ;
#27379 = DIRECTION ( 'NONE',  ( 1.000000000000000000, 3.053848253006669023E-16, -2.042510438544995415E-16 ) ) ;
#27381 = CARTESIAN_POINT ( 'NONE',  ( 58.74999999999980105, -1.253243060178207413, 1.394635017527392495 ) ) ;
#27380 = CARTESIAN_POINT ( 'NONE',  ( 16.10705563471231017, -3.305069970238163179, -4.282766538619540597 ) ) ;
#27382 = EDGE_CURVE ( 'NONE', #11505, #17419, #16281, .T. ) ;
#27383 = EDGE_LOOP ( 'NONE', ( #22456, #15432, #15715, #2298 ) ) ;
#27384 = EDGE_LOOP ( 'NONE', ( #30182, #18316, #23067, #20684 ) ) ;
#27385 = CARTESIAN_POINT ( 'NONE',  ( -59.18749999999995737, -3.399999999999991029, -2.288065396424332102E-13 ) ) ;
#27386 = CIRCLE ( 'NONE', #13223, 0.05000000000000143219 ) ;
#27387 = CARTESIAN_POINT ( 'NONE',  ( 31.20024169076945242, 7.859880411735725048, -1.425000000000108402 ) ) ;
#27388 = ORIENTED_EDGE ( 'NONE', *, *, #10120, .T. ) ;
#27390 = CARTESIAN_POINT ( 'NONE',  ( 51.75086608074121841, -4.173104349845818462, 1.013903299540405145 ) ) ;
#27389 = CARTESIAN_POINT ( 'NONE',  ( -56.44702994616204705, 4.156921938165313080, -1.854183217685626176E-13 ) ) ;
#27391 = FACE_OUTER_BOUND ( 'NONE', #2226, .T. ) ;
#27392 = DIRECTION ( 'NONE',  ( 2.581436205204234006E-16, -0.9796124928211140670, -0.2008964009354148872 ) ) ;
#27393 = ADVANCED_FACE ( 'NONE', ( #28237 ), #29864, .T. ) ;
#27394 = CARTESIAN_POINT ( 'NONE',  ( -59.29999999999995453, -3.258916689102660857, -1.720755220692627097 ) ) ;
#27395 = APPLICATION_CONTEXT ( 'automotive_design' ) ;
#27396 = ORIENTED_EDGE ( 'NONE', *, *, #24412, .T. ) ;
#27397 = DIRECTION ( 'NONE',  ( -3.491481338843133355E-15, -3.491481338843133355E-15, 1.000000000000000000 ) ) ;
#27398 = CARTESIAN_POINT ( 'NONE',  ( 51.80000000000001137, 8.600000000000106226, -2.050000000000179678 ) ) ;
#27399 = CARTESIAN_POINT ( 'NONE',  ( 52.13000000000003098, -0.4999999999994542144, -1.996089927833914146 ) ) ;
#27400 = CIRCLE ( 'NONE', #13731, 2.000000000000000000 ) ;
#27401 = CARTESIAN_POINT ( 'NONE',  ( 15.57907767661755827, -0.5233326973447697261, 5.388419908789401802 ) ) ;
#27402 = ADVANCED_FACE ( 'NONE', ( #10311 ), #10440, .T. ) ;
#27403 = CARTESIAN_POINT ( 'NONE',  ( -59.69999999999998153, -2.268174980119396000, 1.538811659727345349 ) ) ;
#27404 = CIRCLE ( 'NONE', #6173, 2.525000000000001243 ) ;
#27406 = CARTESIAN_POINT ( 'NONE',  ( 58.73379417893121257, -1.830385781109359344, -0.4072049916502183398 ) ) ;
#27405 = CARTESIAN_POINT ( 'NONE',  ( 30.51261366513613993, 7.487866468533194819, -1.425000000000106404 ) ) ;
#27407 = CARTESIAN_POINT ( 'NONE',  ( 60.75000000000002842, -0.4999999999993638977, 1.863080903344643380 ) ) ;
#27408 = CARTESIAN_POINT ( 'NONE',  ( 52.42865501881644263, 4.000228981067450285, -2.045760679945879623 ) ) ;
#27410 = CARTESIAN_POINT ( 'NONE',  ( -59.68558439773848789, 2.070002566049753856, 1.729003918826550024 ) ) ;
#27409 = CARTESIAN_POINT ( 'NONE',  ( 64.94999999999997442, 1.401298464324817071E-42, -4.000000000000680345 ) ) ;
#27411 = EDGE_LOOP ( 'NONE', ( #18333, #4022, #6098, #21620 ) ) ;
#27412 = EDGE_CURVE ( 'NONE', #12164, #15114, #17520, .T. ) ;
#27413 = CARTESIAN_POINT ( 'NONE',  ( 58.50000000000001421, 0.8000000000000000444, 1.778341924377873751 ) ) ;
#27414 = ADVANCED_FACE ( 'NONE', ( #10161 ), #14606, .T. ) ;
#27415 = CARTESIAN_POINT ( 'NONE',  ( 51.45655683570189609, 0.9591657938401613182, 1.611094652690528317 ) ) ;
#27417 = CARTESIAN_POINT ( 'NONE',  ( 68.00000000000001421, -1.025519176787267142E-28, -7.122621931239990530E-13 ) ) ;
#27416 = CARTESIAN_POINT ( 'NONE',  ( 15.03925126672132606, 2.525801270006352350, -4.794550352686297146 ) ) ;
#27419 = EDGE_CURVE ( 'NONE', #27109, #18954, #11963, .T. ) ;
#27418 = DIRECTION ( 'NONE',  ( 0.000000000000000000, 1.000000000000000000, 1.532429380227459806E-15 ) ) ;
#27420 = ORIENTED_EDGE ( 'NONE', *, *, #24547, .T. ) ;
#27421 = CARTESIAN_POINT ( 'NONE',  ( -61.35067034588222867, -2.619031987328097610, 0.4612939446252454778 ) ) ;
#27422 = CARTESIAN_POINT ( 'NONE',  ( 31.30720621464601905, 7.411182539856417506, -1.550000000000108624 ) ) ;
#27423 = EDGE_LOOP ( 'NONE', ( #12500, #814, #2079, #21899 ) ) ;
#27424 = CARTESIAN_POINT ( 'NONE',  ( 15.59140265158956318, -5.360483378448148706, 0.7132926830812496011 ) ) ;
#27425 = ORIENTED_EDGE ( 'NONE', *, *, #13596, .F. ) ;
#27426 = ORIENTED_EDGE ( 'NONE', *, *, #21414, .T. ) ;
#27427 = CARTESIAN_POINT ( 'NONE',  ( 15.90468948301722740, 5.313409993919706586, -1.009519134730147316 ) ) ;
#27428 = CARTESIAN_POINT ( 'NONE',  ( -55.58155989232413674, 3.400000000000007461, -1.857527951337884861E-13 ) ) ;
#27429 = ORIENTED_EDGE ( 'NONE', *, *, #31055, .F. ) ;
#27430 = PRESENTATION_STYLE_ASSIGNMENT (( #522 ) ) ;
#27431 = DIRECTION ( 'NONE',  ( 0.000000000000000000, 0.000000000000000000, -1.000000000000000000 ) ) ;
#27432 = CARTESIAN_POINT ( 'NONE',  ( -54.83155989232412963, 3.925981830489463142, -1.806266843080172912E-13 ) ) ;
#27433 = ORIENTED_EDGE ( 'NONE', *, *, #11867, .F. ) ;
#27434 = DIRECTION ( 'NONE',  ( -2.459562394685754633E-16, 0.9510565162951565288, -0.3090169943749382919 ) ) ;
#27435 = CARTESIAN_POINT ( 'NONE',  ( -77.29999999999998295, -3.473832742311974792E-15, 5.302342620690189014E-15 ) ) ;
#27436 = CARTESIAN_POINT ( 'NONE',  ( 22.49391462655620444, 6.944224163294628660, 2.049999999999920774 ) ) ;
#27437 = EDGE_LOOP ( 'NONE', ( #7900, #26061, #154, #27887 ) ) ;
#27438 = CARTESIAN_POINT ( 'NONE',  ( -57.62499999999996447, -2.944486372867076707, -1.700000000000215117 ) ) ;
#27439 = FACE_OUTER_BOUND ( 'NONE', #9092, .T. ) ;
#27440 = CARTESIAN_POINT ( 'NONE',  ( 50.25000000000002842, -0.5380862305904318132, -1.858165151418244010 ) ) ;
#27441 = TOROIDAL_SURFACE ( 'NONE', #11785, 1.649144805949033898, 0.05000000000000000278 ) ;
#27442 = DIRECTION ( 'NONE',  ( 2.586136946169074517E-16, -1.000000000000000000, 0.000000000000000000 ) ) ;
#27443 = EDGE_CURVE ( 'NONE', #11715, #25939, #19832, .T. ) ;
#27444 = CARTESIAN_POINT ( 'NONE',  ( -77.29999999999998295, 0.4398635404618077005, 0.01095745282448230308 ) ) ;
#27445 = EDGE_CURVE ( 'NONE', #10332, #4498, #20046, .T. ) ;
#27447 = DIRECTION ( 'NONE',  ( 1.000000000000000000, -0.000000000000000000, -0.000000000000000000 ) ) ;
#27446 = CARTESIAN_POINT ( 'NONE',  ( -71.49999999999998579, -0.9743475445367636434, 4.751120590182405401 ) ) ;
#27448 = CARTESIAN_POINT ( 'NONE',  ( 51.45655683570189609, 0.9591657938401617622, 1.468576096419531352 ) ) ;
#27449 = CARTESIAN_POINT ( 'NONE',  ( 58.75000000000003553, -1.470078920827206925, -1.470078920827526892 ) ) ;
#27450 = CARTESIAN_POINT ( 'NONE',  ( 58.65844932252365851, 1.349094575299792043, -1.302247349114688424 ) ) ;
#27451 = CARTESIAN_POINT ( 'NONE',  ( 53.81456880582373259, 5.799118505022251568, 1.784642093723081357 ) ) ;
#27452 = ORIENTED_EDGE ( 'NONE', *, *, #28610, .T. ) ;
#27453 = CARTESIAN_POINT ( 'NONE',  ( -54.44999999999997442, 1.499999999999998890, 3.300094695611021756 ) ) ;
#27454 = ORIENTED_EDGE ( 'NONE', *, *, #24354, .T. ) ;
#27455 = VERTEX_POINT ( 'NONE', #26798 ) ;
#27456 = DIRECTION ( 'NONE',  ( 1.000000000000000000, 0.000000000000000000, -3.469446951951483476E-15 ) ) ;
#27457 = CARTESIAN_POINT ( 'NONE',  ( -58.23542740578360366, 0.7887156198831662968, -3.845940847736174284 ) ) ;
#27459 = CARTESIAN_POINT ( 'NONE',  ( -61.35508841351263953, -2.585893814015340020, 0.6744937573145690646 ) ) ;
#27458 = CARTESIAN_POINT ( 'NONE',  ( -55.43749999999997158, -3.925981830489445379, -2.111188856984502568E-13 ) ) ;
#27460 = VERTEX_POINT ( 'NONE', #7323 ) ;
#27461 = VERTEX_POINT ( 'NONE', #3512 ) ;
#27462 = CARTESIAN_POINT ( 'NONE',  ( 51.06312929986522420, -4.312041630646782586, -1.282098934413016700 ) ) ;
#27463 = VERTEX_POINT ( 'NONE', #13151 ) ;
#27464 = DIRECTION ( 'NONE',  ( -1.000000000000000000, -3.053848253006669023E-16, 2.042510438544995415E-16 ) ) ;
#27465 = ORIENTED_EDGE ( 'NONE', *, *, #28524, .F. ) ;
#27466 = CARTESIAN_POINT ( 'NONE',  ( 22.49391462655623997, 6.944224163294429708, -2.050000000000078426 ) ) ;
#27467 = CARTESIAN_POINT ( 'NONE',  ( 50.80000000000001137, -4.387164041431065975, -1.383037119376935742 ) ) ;
#27468 = CARTESIAN_POINT ( 'NONE',  ( -61.34999999999997300, -2.556251174960431971, 0.6635690258132532771 ) ) ;
#27469 = CARTESIAN_POINT ( 'NONE',  ( 15.48686146417452747, -4.979756346315167725, -1.501439362221205442 ) ) ;
#27470 = CARTESIAN_POINT ( 'NONE',  ( -58.14405989232411542, -2.944486372867076263, -1.700000000000216893 ) ) ;
#27471 = DIRECTION ( 'NONE',  ( 1.000000000000000000, 1.047444401652940007E-14, -0.000000000000000000 ) ) ;
#27472 = ADVANCED_FACE ( 'NONE', ( #7947 ), #28137, .T. ) ;
#27473 = CARTESIAN_POINT ( 'NONE',  ( 51.70000000000001705, -4.276948333784438283, -0.9210526315789475671 ) ) ;
#27474 = EDGE_CURVE ( 'NONE', #10684, #4543, #22593, .T. ) ;
#27475 = CARTESIAN_POINT ( 'NONE',  ( -59.69999999999997442, 8.366749974758454467E-15, -2.120534355533670266E-13 ) ) ;
#27476 = EDGE_CURVE ( 'NONE', #29070, #5429, #15840, .T. ) ;
#27477 = DIRECTION ( 'NONE',  ( 1.000000000000000000, -1.219044193948983948E-29, 3.491481338843133355E-15 ) ) ;
#27479 = CARTESIAN_POINT ( 'NONE',  ( 51.42173091724420431, -4.356630359622029047, 1.481809601934319209 ) ) ;
#27478 = CARTESIAN_POINT ( 'NONE',  ( -59.44986384413810043, 3.257863816608426166, 1.316887994369795978 ) ) ;
#27480 = CIRCLE ( 'NONE', #2211, 0.2500000000000000555 ) ;
#27481 = CARTESIAN_POINT ( 'NONE',  ( 60.67929986713517820, 1.401298464324817071E-42, 2.973495046502070860 ) ) ;
#27482 = PLANE ( 'NONE',  #7941 ) ;
#27483 = CARTESIAN_POINT ( 'NONE',  ( 51.02976068049119363, -1.019450805964126516, 1.268081568884226407 ) ) ;
#27484 = ORIENTED_EDGE ( 'NONE', *, *, #27047, .F. ) ;
#27485 = CARTESIAN_POINT ( 'NONE',  ( 15.03925126672132961, 2.686240680702102424, 4.475885388010754085 ) ) ;
#27486 = CARTESIAN_POINT ( 'NONE',  ( 54.44737856558258926, 6.357064942762717052, -1.856154119295183591E-13 ) ) ;
#27487 = ORIENTED_EDGE ( 'NONE', *, *, #6956, .F. ) ;
#27488 = EDGE_CURVE ( 'NONE', #17902, #6274, #27142, .T. ) ;
#27489 = DIRECTION ( 'NONE',  ( 0.000000000000000000, -0.9507508458640268056, 0.3099561728516426751 ) ) ;
#27490 = ORIENTED_EDGE ( 'NONE', *, *, #29506, .F. ) ;
#27491 = CARTESIAN_POINT ( 'NONE',  ( 15.41170998834775041, -0.6969927240735035445, -5.374332520738491326 ) ) ;
#27492 = CARTESIAN_POINT ( 'NONE',  ( -37.18272003341174781, 24.59258869922085111, 0.000000000000000000 ) ) ;
#27494 = DIRECTION ( 'NONE',  ( 1.000000000000000000, 5.172273892338151992E-16, 0.000000000000000000 ) ) ;
#27493 = CARTESIAN_POINT ( 'NONE',  ( 61.25000000000003553, -0.8666666666660258755, 1.374595900215366262 ) ) ;
#27495 = ORIENTED_EDGE ( 'NONE', *, *, #19683, .F. ) ;
#27496 = VERTEX_POINT ( 'NONE', #11093 ) ;
#27497 = DIRECTION ( 'NONE',  ( 0.000000000000000000, 0.2008964009354152203, -0.9796124928211138450 ) ) ;
#27498 = CARTESIAN_POINT ( 'NONE',  ( 57.03643325641707662, -0.7481242503215885797, -1.780024810282529790 ) ) ;
#27499 = CARTESIAN_POINT ( 'NONE',  ( -57.83155989232412253, 3.400000000000007905, -1.837192174579415376E-13 ) ) ;
#27500 = DIRECTION ( 'NONE',  ( 0.000000000000000000, 0.000000000000000000, 1.000000000000000000 ) ) ;
#27501 = ORIENTED_EDGE ( 'NONE', *, *, #12017, .T. ) ;
#27502 = DIRECTION ( 'NONE',  ( 0.000000000000000000, -0.2008964009354147484, 0.9796124928211140670 ) ) ;
#27503 = TOROIDAL_SURFACE ( 'NONE', #10302, 4.349999999999997868, 0.05000000000000000278 ) ;
#27504 = CARTESIAN_POINT ( 'NONE',  ( 51.80000000000002558, 3.850000000000016520, 1.678541033159270279 ) ) ;
#27505 = CARTESIAN_POINT ( 'NONE',  ( 51.25000000000001421, 1.163569835200988601E-28, -1.789384186157106949E-13 ) ) ;
#27506 = CARTESIAN_POINT ( 'NONE',  ( 22.04321716858595082, 7.679566743993206934, 1.549999999999923217 ) ) ;
#27507 = CARTESIAN_POINT ( 'NONE',  ( -55.82202994616203995, 2.078460969082674747, -3.600000000000189715 ) ) ;
#27508 = VERTEX_POINT ( 'NONE', #27409 ) ;
#27509 = EDGE_CURVE ( 'NONE', #25040, #21014, #340, .T. ) ;
#27510 = CARTESIAN_POINT ( 'NONE',  ( 15.68751737981905947, 2.884962146574134856, 4.577321775072962673 ) ) ;
#27511 = AXIS2_PLACEMENT_3D ( 'NONE', #25599, #11048, #9149 ) ;
#27512 = CARTESIAN_POINT ( 'NONE',  ( -73.89999999999997726, -0.4598573377555323360, -0.01145551886194856595 ) ) ;
#27513 = CARTESIAN_POINT ( 'NONE',  ( -59.29999999999997584, -0.7533615035078030653, 3.673546848079178417 ) ) ;
#27514 = VECTOR ( 'NONE', #2185, 1000.000000000000000 ) ;
#27515 = CARTESIAN_POINT ( 'NONE',  ( -58.50952994616205416, -2.184195341338215755E-14, 3.599999999999791367 ) ) ;
#27516 = CARTESIAN_POINT ( 'NONE',  ( 58.72419296898093677, -1.874576113083205486, -0.04475215827324158929 ) ) ;
#27517 = CARTESIAN_POINT ( 'NONE',  ( 58.72202590147342249, 0.4851612519499358678, 1.811144268316692729 ) ) ;
#27518 = VERTEX_POINT ( 'NONE', #5884 ) ;
#27519 = ADVANCED_FACE ( 'NONE', ( #24871 ), #30253, .T. ) ;
#27520 = DIRECTION ( 'NONE',  ( 2.581436205204234006E-16, -0.9796124928211140670, -0.2008964009354148872 ) ) ;
#27521 = VERTEX_POINT ( 'NONE', #20157 ) ;
#27522 = PRODUCT_DEFINITION_CONTEXT ( 'detailed design', #30215, 'design' ) ;
#27523 = CARTESIAN_POINT ( 'NONE',  ( 50.46977479615470230, -1.142230555601075004, 3.938343097974785767 ) ) ;
#27525 = CARTESIAN_POINT ( 'NONE',  ( 47.00000000000002132, -4.131056160354152240, 1.099999999999999867 ) ) ;
#27524 = CARTESIAN_POINT ( 'NONE',  ( -54.49626650188002941, -2.282174794334375534, -2.722251751099368011 ) ) ;
#27526 = ORIENTED_EDGE ( 'NONE', *, *, #7513, .F. ) ;
#27527 = EDGE_LOOP ( 'NONE', ( #11452, #16020 ) ) ;
#27528 = CARTESIAN_POINT ( 'NONE',  ( 58.75000000000002132, 6.153735859711025284E-13, 3.111507638930570854E-58 ) ) ;
#27529 = CYLINDRICAL_SURFACE ( 'NONE', #23240, 1.875000000000001776 ) ;
#27530 = ORIENTED_EDGE ( 'NONE', *, *, #26248, .T. ) ;
#27532 = DIRECTION ( 'NONE',  ( 1.000000000000000000, 3.054025858079668409E-16, -2.042474015755241579E-16 ) ) ;
#27531 = CARTESIAN_POINT ( 'NONE',  ( -59.69702994616202574, -2.078460969082631227, -3.600000000000218137 ) ) ;
#27533 = CARTESIAN_POINT ( 'NONE',  ( -57.48542740578361077, 0.7887156198831664078, -3.845940847736174284 ) ) ;
#27534 = AXIS2_PLACEMENT_3D ( 'NONE', #25075, #20206, #3411 ) ;
#27536 = EDGE_CURVE ( 'NONE', #13205, #26264, #1350, .T. ) ;
#27535 = CIRCLE ( 'NONE', #14386, 4.275000000000000355 ) ;
#27537 = DIRECTION ( 'NONE',  ( -1.000000000000000000, -3.054025858079668409E-16, 2.042474015755241579E-16 ) ) ;
#27538 = DIRECTION ( 'NONE',  ( 1.000000000000000000, 0.000000000000000000, 0.000000000000000000 ) ) ;
#27539 = CARTESIAN_POINT ( 'NONE',  ( 58.75000000000002132, 6.153735859711025284E-13, 3.111507638930570854E-58 ) ) ;
#27540 = VECTOR ( 'NONE', #14503, 1000.000000000000000 ) ;
#27541 = ORIENTED_EDGE ( 'NONE', *, *, #20362, .T. ) ;
#27542 = EDGE_CURVE ( 'NONE', #20590, #12071, #17769, .T. ) ;
#27543 = DIRECTION ( 'NONE',  ( -0.9993908270190957621, 0.03489949670250202390, 3.491481338843133355E-15 ) ) ;
#27544 = TOROIDAL_SURFACE ( 'NONE', #14911, 160.5997717543497743, 0.1000000000000000056 ) ;
#27545 = CARTESIAN_POINT ( 'NONE',  ( 52.80702527127468926, 4.040723488129245311, -2.050000000000183675 ) ) ;
#27546 = CARTESIAN_POINT ( 'NONE',  ( 48.40000000000002700, -0.7711297561635785947, -3.938774833552663335 ) ) ;
#27547 = CARTESIAN_POINT ( 'NONE',  ( 16.10705563471230661, 0.1565107631088668017, 5.407502298984289801 ) ) ;
#27548 = B_SPLINE_CURVE_WITH_KNOTS ( 'NONE', 3,
 ( #26401, #118, #11998, #18973 ),
 .UNSPECIFIED., .F., .F.,
 ( 4, 4 ),
 ( 0.0001159639600970536317, 0.0002000540139203089898 ),
 .UNSPECIFIED. ) ;
#27549 = DIRECTION ( 'NONE',  ( -2.614375865348240525E-16, 0.2008964009354147207, -0.9796124928211138450 ) ) ;
#27551 = DIRECTION ( 'NONE',  ( 2.457191765101193999E-12, 0.8381322357048476279, -0.5454670984325213912 ) ) ;
#27550 = DIRECTION ( 'NONE',  ( 1.000000000000000000, 3.053848253006669023E-16, -2.042510438544995415E-16 ) ) ;
#27552 = CIRCLE ( 'NONE', #22027, 0.09999999999999989453 ) ;
#27553 = CARTESIAN_POINT ( 'NONE',  ( 50.25000000000000000, 1.470078920828055358, -1.470078920826818125 ) ) ;
#27554 = LINE ( 'NONE', #22686, #16512 ) ;
#27556 = CARTESIAN_POINT ( 'NONE',  ( -54.49999999999997868, 0.2900967345938421649, -3.387601494358211340 ) ) ;
#27555 = DIRECTION ( 'NONE',  ( 1.000000000000000000, 0.000000000000000000, 0.000000000000000000 ) ) ;
#27557 = AXIS2_PLACEMENT_3D ( 'NONE', #6546, #2100, #11764 ) ;
#27558 = ORIENTED_EDGE ( 'NONE', *, *, #15191, .F. ) ;
#27559 = EDGE_CURVE ( 'NONE', #20392, #10836, #18928, .T. ) ;
#27560 = DIRECTION ( 'NONE',  ( -1.000000000000000000, -0.000000000000000000, -0.000000000000000000 ) ) ;
#27561 = CARTESIAN_POINT ( 'NONE',  ( -59.59999999999998010, 8.366749974758452890E-15, -2.117042874194827196E-13 ) ) ;
#27563 = PLANE ( 'NONE',  #22730 ) ;
#27562 = CARTESIAN_POINT ( 'NONE',  ( 15.81621483022862762, 3.777141534544376178, -3.869853550719620117 ) ) ;
#27564 = DIRECTION ( 'NONE',  ( 1.000000000000000000, -0.000000000000000000, -0.000000000000000000 ) ) ;
#27565 = VERTEX_POINT ( 'NONE', #18241 ) ;
#27566 = CARTESIAN_POINT ( 'NONE',  ( 53.60047708782973785, 7.640852521089409599, 2.049999999999813305 ) ) ;
#27567 = CARTESIAN_POINT ( 'NONE',  ( 29.25706191173315673, 5.994885333997870269, -1.550000000000101741 ) ) ;
#27568 = AXIS2_PLACEMENT_3D ( 'NONE', #19255, #1979, #11951 ) ;
#27569 = ORIENTED_EDGE ( 'NONE', *, *, #813, .T. ) ;
#27570 = AXIS2_PLACEMENT_3D ( 'NONE', #15051, #334, #14881 ) ;
#27571 = DIRECTION ( 'NONE',  ( -1.000000000000000000, -0.000000000000000000, -0.000000000000000000 ) ) ;
#27572 = ADVANCED_FACE ( 'NONE', ( #27730 ), #18050, .T. ) ;
#27573 = ORIENTED_EDGE ( 'NONE', *, *, #26313, .T. ) ;
#27574 = DIRECTION ( 'NONE',  ( -1.000000000000000000, -0.000000000000000000, 3.491481338843133355E-15 ) ) ;
#27575 = CARTESIAN_POINT ( 'NONE',  ( 51.25000000000002842, -1.099999999999462963, -1.196087371390569087 ) ) ;
#27576 = ORIENTED_EDGE ( 'NONE', *, *, #22498, .T. ) ;
#27577 = CARTESIAN_POINT ( 'NONE',  ( 34.27001433279279752, 8.197396758520717697, 1.949999999999880274 ) ) ;
#27578 = CARTESIAN_POINT ( 'NONE',  ( -54.95655989232411542, 1.962990915244748891, -3.400000000000186429 ) ) ;
#27579 = ORIENTED_EDGE ( 'NONE', *, *, #11207, .T. ) ;
#27580 = DIRECTION ( 'NONE',  ( 4.117859380279907901E-15, -0.9495137264943731559, -0.3137254901960768172 ) ) ;
#27581 = ORIENTED_EDGE ( 'NONE', *, *, #22376, .F. ) ;
#27582 = DIRECTION ( 'NONE',  ( 1.000000000000000000, 9.742518634745315608E-17, -4.338815227902241051E-17 ) ) ;
#27583 = CIRCLE ( 'NONE', #13916, 4.100000000000022737 ) ;
#27584 = AXIS2_PLACEMENT_3D ( 'NONE', #19187, #28827, #19480 ) ;
#27585 = CARTESIAN_POINT ( 'NONE',  ( 22.09542497983118281, 7.445411299649673964, 2.050000000000058886 ) ) ;
#27586 = ORIENTED_EDGE ( 'NONE', *, *, #515, .T. ) ;
#27587 = B_SPLINE_CURVE_WITH_KNOTS ( 'NONE', 3,
 ( #16992, #29322, #19372, #27089, #21912, #7322, #5412, #2723, #7634, #19979, #15223, #192, #29618, #24870 ),
 .UNSPECIFIED., .F., .F.,
 ( 4, 2, 2, 2, 2, 2, 4 ),
 ( 0.000000000000000000, 2.506106230924540920E-05, 5.012212461849081840E-05, 0.0001002442492369731529, 0.0002004884984739371985, 0.0004009769969478685966, 0.0008019539938957305795 ),
 .UNSPECIFIED. ) ;
#27588 = AXIS2_PLACEMENT_3D ( 'NONE', #29164, #2717, #19368 ) ;
#27589 = CARTESIAN_POINT ( 'NONE',  ( -57.31249999999997158, 3.925981830489463142, -1.892888403967549806E-13 ) ) ;
#27590 = CARTESIAN_POINT ( 'NONE',  ( 69.20000000000005969, 0.5000000000000000000, 1.988246715072633952 ) ) ;
#27591 = FACE_OUTER_BOUND ( 'NONE', #21526, .T. ) ;
#27593 = EDGE_CURVE ( 'NONE', #10800, #16137, #15505, .T. ) ;
#27592 = CARTESIAN_POINT ( 'NONE',  ( -62.04999999999998295, 1.183285843523195887E-15, 2.187514201909070562E-15 ) ) ;
#27594 = TOROIDAL_SURFACE ( 'NONE', #12421, 2.750000000000000000, 0.1000000000000000056 ) ;
#27595 = DIRECTION ( 'NONE',  ( -0.9993908270190956511, 0.03489949670250202390, 3.491481338843132961E-15 ) ) ;
#27596 = VECTOR ( 'NONE', #26166, 1000.000000000000000 ) ;
#27597 = AXIS2_PLACEMENT_3D ( 'NONE', #8456, #25392, #20670 ) ;
#27599 = DIRECTION ( 'NONE',  ( -3.002035892788117459E-16, 0.9996898646859344595, 0.02490330187381124133 ) ) ;
#27598 = DIRECTION ( 'NONE',  ( 3.491481338843133355E-15, -0.000000000000000000, 1.000000000000000000 ) ) ;
#27600 = B_SPLINE_CURVE_WITH_KNOTS ( 'NONE', 3,
 ( #21396, #6980, #16645, #15620, #17988, #25264, #10552, #20381, #20229, #15907, #1049, #29701, #5967, #8318 ),
 .UNSPECIFIED., .F., .F.,
 ( 4, 2, 2, 2, 2, 2, 4 ),
 ( 0.000000000000000000, 0.0003953907277084696219, 0.0005930860915627040805, 0.0006919337734898216080, 0.0007413576144533806428, 0.0007660695349351558233, 0.0007907814554169310039 ),
 .UNSPECIFIED. ) ;
#27601 = LINE ( 'NONE', #22255, #31178 ) ;
#27602 = CARTESIAN_POINT ( 'NONE',  ( 51.65293807187808994, 3.825852911387368493, -2.050000000000177902 ) ) ;
#27603 = CARTESIAN_POINT ( 'NONE',  ( 61.25000000000004263, -1.791164585742460735, -0.8897917884440847969 ) ) ;
#27604 = CARTESIAN_POINT ( 'NONE',  ( 58.74999981404332061, 1.321446761053438168, -1.441842230226794808 ) ) ;
#27605 = EDGE_CURVE ( 'NONE', #14413, #11810, #28861, .T. ) ;
#27606 = CARTESIAN_POINT ( 'NONE',  ( 53.56882961073743843, 7.945105661027664468, -2.050000000000185896 ) ) ;
#27607 = VERTEX_POINT ( 'NONE', #29940 ) ;
#27608 = DIRECTION ( 'NONE',  ( 1.000000000000000000, -0.000000000000000000, -0.000000000000000000 ) ) ;
#27609 = VECTOR ( 'NONE', #5104, 1000.000000000000227 ) ;
#27610 = CARTESIAN_POINT ( 'NONE',  ( 58.65000000000003411, -0.8799718970823581232, 1.656030381686199870 ) ) ;
#27611 = AXIS2_PLACEMENT_3D ( 'NONE', #8737, #17952, #25383 ) ;
#27612 = VERTEX_POINT ( 'NONE', #811 ) ;
#27613 = ORIENTED_EDGE ( 'NONE', *, *, #15805, .T. ) ;
#27614 = DIRECTION ( 'NONE',  ( 1.000000000000000000, 3.053848253006669023E-16, -2.042510438544995415E-16 ) ) ;
#27615 = CARTESIAN_POINT ( 'NONE',  ( -58.29792740578360366, -1.073804522883517132, -3.225979517392335350 ) ) ;
#27617 = CARTESIAN_POINT ( 'NONE',  ( 57.05000000000001847, 0.8000000000000000444, 2.421260002560649660 ) ) ;
#27616 = CARTESIAN_POINT ( 'NONE',  ( -58.31249999999995026, -1.962990915244707368, -3.400000000000213518 ) ) ;
#27618 = ORIENTED_EDGE ( 'NONE', *, *, #1272, .F. ) ;
#27619 = EDGE_CURVE ( 'NONE', #16975, #26152, #3376, .T. ) ;
#27620 = ORIENTED_EDGE ( 'NONE', *, *, #15083, .F. ) ;
#27621 = DIRECTION ( 'NONE',  ( 0.000000000000000000, 0.000000000000000000, 1.000000000000000000 ) ) ;
#27622 = ORIENTED_EDGE ( 'NONE', *, *, #2418, .F. ) ;
#27624 = FACE_OUTER_BOUND ( 'NONE', #24136, .T. ) ;
#27623 = AXIS2_PLACEMENT_3D ( 'NONE', #16517, #4308, #21292 ) ;
#27625 = ORIENTED_EDGE ( 'NONE', *, *, #29123, .T. ) ;
#27626 = CARTESIAN_POINT ( 'NONE',  ( 58.66054497607991891, 0.5000000000007229772, 1.807104036850091910 ) ) ;
#27627 = CIRCLE ( 'NONE', #327, 0.4999999999999996114 ) ;
#27628 = EDGE_CURVE ( 'NONE', #29888, #6920, #11401, .T. ) ;
#27629 = DIRECTION ( 'NONE',  ( 1.000000000000000000, -1.219044193948983948E-29, 3.491481338843133355E-15 ) ) ;
#27630 = CYLINDRICAL_SURFACE ( 'NONE', #4558, 0.2500000000000000000 ) ;
#27631 = CARTESIAN_POINT ( 'NONE',  ( 46.99423841112505329, -4.272136569073790469, -0.9439330974869863944 ) ) ;
#27632 = CIRCLE ( 'NONE', #29226, 0.1500000000000001887 ) ;
#27633 = EDGE_CURVE ( 'NONE', #25794, #11615, #19071, .T. ) ;
#27634 = CARTESIAN_POINT ( 'NONE',  ( -57.70655989232413674, 1.962990915244722245, 3.399999999999802291 ) ) ;
#27636 = EDGE_CURVE ( 'NONE', #4273, #16343, #28024, .T. ) ;
#27635 = CARTESIAN_POINT ( 'NONE',  ( -57.72085481156722864, 1.184343223768590914, 3.558065644182727194 ) ) ;
#27637 = AXIS2_PLACEMENT_3D ( 'NONE', #23919, #16167, #25815 ) ;
#27638 = CARTESIAN_POINT ( 'NONE',  ( 58.64999999999999858, 1.782657835994909901, 0.5811678240991515754 ) ) ;
#27639 = AXIS2_PLACEMENT_3D ( 'NONE', #20963, #20237, #29869 ) ;
#27640 = FACE_OUTER_BOUND ( 'NONE', #17348, .T. ) ;
#27641 = AXIS2_PLACEMENT_3D ( 'NONE', #31031, #18387, #23918 ) ;
#27642 = FACE_OUTER_BOUND ( 'NONE', #2474, .T. ) ;
#27644 = CARTESIAN_POINT ( 'NONE',  ( 50.93211418564875004, -4.319730106544481529, 1.256953381563011618 ) ) ;
#27643 = DIRECTION ( 'NONE',  ( 0.000000000000000000, 0.000000000000000000, 1.000000000000000000 ) ) ;
#27645 = AXIS2_PLACEMENT_3D ( 'NONE', #26329, #4628, #2250 ) ;
#27646 = CIRCLE ( 'NONE', #3889, 4.500000000000037303 ) ;
#27647 = CARTESIAN_POINT ( 'NONE',  ( -58.72085481156723574, 2.489203624310592389, -2.804704140674918911 ) ) ;
#27648 = DIRECTION ( 'NONE',  ( 1.282749433769087582E-30, 1.000000000000000000, 1.224646799147353207E-16 ) ) ;
#27649 = AXIS2_PLACEMENT_3D ( 'NONE', #25060, #15583, #13039 ) ;
#27650 = CARTESIAN_POINT ( 'NONE',  ( 56.95000000000001705, -0.6820512820512819596, 1.773360101234998210 ) ) ;
#27651 = AXIS2_PLACEMENT_3D ( 'NONE', #25381, #23326, #8281 ) ;
#27652 = ORIENTED_EDGE ( 'NONE', *, *, #13678, .F. ) ;
#27653 = DIRECTION ( 'NONE',  ( 1.000000000000000000, 1.047444401652940007E-14, 0.000000000000000000 ) ) ;
#27654 = CARTESIAN_POINT ( 'NONE',  ( 54.44724579895265748, 6.358489013468038742, 1.963089969304595783 ) ) ;
#27655 = ORIENTED_EDGE ( 'NONE', *, *, #20091, .F. ) ;
#27656 = ORIENTED_EDGE ( 'NONE', *, *, #8109, .T. ) ;
#27657 = CARTESIAN_POINT ( 'NONE',  ( 15.22842924604238135, -0.7747498452696431892, -5.363501451415723764 ) ) ;
#27658 = CARTESIAN_POINT ( 'NONE',  ( -54.53335481156723574, -4.108500314926510022, 1.367561758111406789 ) ) ;
#27660 = DIRECTION ( 'NONE',  ( -1.000000000000000000, 0.000000000000000000, 0.000000000000000000 ) ) ;
#27659 = CARTESIAN_POINT ( 'NONE',  ( 61.00000000000003553, -0.8666666666660277629, 1.374595900215364930 ) ) ;
#27661 = CIRCLE ( 'NONE', #26651, 0.2499999999999997780 ) ;
#27662 = VERTEX_POINT ( 'NONE', #1912 ) ;
#27663 = EDGE_CURVE ( 'NONE', #8534, #17883, #29669, .T. ) ;
#27664 = CARTESIAN_POINT ( 'NONE',  ( 51.87416143049283335, 8.598705507415685290, -1.950000000000180256 ) ) ;
#27665 = AXIS2_PLACEMENT_3D ( 'NONE', #22446, #26875, #26740 ) ;
#27666 = ADVANCED_FACE ( 'NONE', ( #18710 ), #22103, .T. ) ;
#27667 = CARTESIAN_POINT ( 'NONE',  ( -54.49999999999996447, 1.500000000000023759, -3.959797974644871044 ) ) ;
#27668 = VECTOR ( 'NONE', #1920, 1000.000000000000000 ) ;
#27669 = ORIENTED_EDGE ( 'NONE', *, *, #15906, .T. ) ;
#27671 = CARTESIAN_POINT ( 'NONE',  ( 64.00000000000001421, 1.163569835200988601E-28, -2.234548056859606357E-13 ) ) ;
#27670 = DIRECTION ( 'NONE',  ( 1.000000000000000000, 1.047444401652940007E-14, 0.000000000000000000 ) ) ;
#27672 = EDGE_CURVE ( 'NONE', #10954, #23278, #26631, .T. ) ;
#27673 = DIRECTION ( 'NONE',  ( -1.000000000000000000, -0.000000000000000000, -0.000000000000000000 ) ) ;
#27674 = EDGE_LOOP ( 'NONE', ( #22854, #13854, #21698, #12683 ) ) ;
#27675 = CARTESIAN_POINT ( 'NONE',  ( -36.43290890416757577, 5.277544294472448883, -1.204650266290766103 ) ) ;
#27676 = CARTESIAN_POINT ( 'NONE',  ( 58.64999999999999858, 1.671477153795419834, -0.8495817349390366591 ) ) ;
#27677 = AXIS2_PLACEMENT_3D ( 'NONE', #4880, #24210, #17095 ) ;
#27678 = CARTESIAN_POINT ( 'NONE',  ( -35.85663232820584057, -2.686240680702168593, 4.475885388010719446 ) ) ;
#27679 = DIRECTION ( 'NONE',  ( 1.000000000000000000, 0.000000000000000000, 0.000000000000000000 ) ) ;
#27680 = AXIS2_PLACEMENT_3D ( 'NONE', #3797, #9199, #6335 ) ;
#27681 = TOROIDAL_SURFACE ( 'NONE', #4421, 2.549999999999999822, 0.05000000000000000278 ) ;
#27682 = FACE_OUTER_BOUND ( 'NONE', #3948, .T. ) ;
#27683 = ORIENTED_EDGE ( 'NONE', *, *, #28217, .T. ) ;
#27684 = CARTESIAN_POINT ( 'NONE',  ( 15.81621483022873775, 2.513248512186213812, 4.788125582312069639 ) ) ;
#27685 = VECTOR ( 'NONE', #749, 1000.000000000000000 ) ;
#27686 = AXIS2_PLACEMENT_3D ( 'NONE', #21955, #17499, #26986 ) ;
#27687 = CARTESIAN_POINT ( 'NONE',  ( -60.61395381780661751, -2.505988366243331100, 0.9638607592909542721 ) ) ;
#27688 = AXIS2_PLACEMENT_3D ( 'NONE', #9157, #21509, #24025 ) ;
#27689 = CARTESIAN_POINT ( 'NONE',  ( 50.31971926781695004, 8.252744006147214151, 2.049999999999824407 ) ) ;
#27690 = CARTESIAN_POINT ( 'NONE',  ( -56.57202994616203995, 2.078460969082686294, -3.600000000000185718 ) ) ;
#27691 = CARTESIAN_POINT ( 'NONE',  ( 58.75000018595672913, -1.936190688449155317, 0.04992417795738181979 ) ) ;
#27692 = CARTESIAN_POINT ( 'NONE',  ( -67.99999999999995737, -0.5554785485864222050, 2.708628542650383331 ) ) ;
#27693 = VERTEX_POINT ( 'NONE', #6990 ) ;
#27694 = VECTOR ( 'NONE', #16743, 999.9999999999998863 ) ;
#27695 = CARTESIAN_POINT ( 'NONE',  ( 61.25000000000000711, 1.499837071478820505, -1.323060376180830833 ) ) ;
#27696 = ORIENTED_EDGE ( 'NONE', *, *, #15624, .F. ) ;
#27697 = FACE_OUTER_BOUND ( 'NONE', #8421, .T. ) ;
#27699 = DIRECTION ( 'NONE',  ( -3.489354422748178582E-15, 1.218509414717996338E-16, -1.000000000000000000 ) ) ;
#27698 = DIRECTION ( 'NONE',  ( 0.000000000000000000, 0.000000000000000000, 1.000000000000000000 ) ) ;
#27700 = VERTEX_POINT ( 'NONE', #9354 ) ;
#27701 = ORIENTED_EDGE ( 'NONE', *, *, #10888, .F. ) ;
#27702 = FACE_OUTER_BOUND ( 'NONE', #19348, .T. ) ;
#27703 = ADVANCED_FACE ( 'NONE', ( #11877 ), #10959, .T. ) ;
#27704 = FACE_BOUND ( 'NONE', #13979, .T. ) ;
#27705 = ORIENTED_EDGE ( 'NONE', *, *, #20198, .T. ) ;
#27707 = CARTESIAN_POINT ( 'NONE',  ( -61.34999999999997300, -2.661068980108069137, 0.4568499568858441773 ) ) ;
#27706 = CARTESIAN_POINT ( 'NONE',  ( -61.00952994616203284, 3.117691453623994580, -1.800000000000202993 ) ) ;
#27708 = EDGE_CURVE ( 'NONE', #2745, #5953, #13918, .T. ) ;
#27709 = CARTESIAN_POINT ( 'NONE',  ( -59.42292740578359656, 1.073804522883521351, 3.225979517392337126 ) ) ;
#27710 = AXIS2_PLACEMENT_3D ( 'NONE', #9066, #11752, #1608 ) ;
#27711 = LINE ( 'NONE', #10913, #4651 ) ;
#27712 = ITEM_DEFINED_TRANSFORMATION ( 'NONE', 'NONE', #30804,  #9018 ) ;
#27713 = CIRCLE ( 'NONE', #24192, 0.04999999999999988481 ) ;
#27714 = CARTESIAN_POINT ( 'NONE',  ( 53.30599709427681177, 4.975793220244357329, -1.612824162456762300 ) ) ;
#27715 = TOROIDAL_SURFACE ( 'NONE', #12462, 2.649999999999999911, 0.05000000000000000278 ) ;
#27716 =( BOUNDED_CURVE ( )  B_SPLINE_CURVE ( 3, ( #18846, #25796, #28653, #1712 ),
 .UNSPECIFIED., .F., .T. ) 
 B_SPLINE_CURVE_WITH_KNOTS ( ( 4, 4 ),
 ( 1.011983630320553299E-14, 1.570796326794897890 ),
 .UNSPECIFIED. ) 
 CURVE ( )  GEOMETRIC_REPRESENTATION_ITEM ( )  RATIONAL_B_SPLINE_CURVE ( ( 1.000000000000000000, 0.8047378541243670469, 0.8047378541243670469, 1.000000000000000000 ) ) 
 REPRESENTATION_ITEM ( '' )  );
#27717 = ORIENTED_EDGE ( 'NONE', *, *, #6112, .T. ) ;
#27718 = EDGE_CURVE ( 'NONE', #19839, #24615, #6810, .T. ) ;
#27719 = CARTESIAN_POINT ( 'NONE',  ( -59.59999999999998010, 8.366749974758452890E-15, -2.117042874194827196E-13 ) ) ;
#27720 = CARTESIAN_POINT ( 'NONE',  ( 53.34494210428217542, 4.987020249080358347, -1.614082030464848438 ) ) ;
#27721 = DIRECTION ( 'NONE',  ( -1.047444401652940007E-14, 0.000000000000000000, -1.000000000000000000 ) ) ;
#27722 = CARTESIAN_POINT ( 'NONE',  ( 15.44259799936806665, -0.2181161761757533513, 5.200000001420971962 ) ) ;
#27723 = DIRECTION ( 'NONE',  ( -1.040834085586084257E-14, 0.000000000000000000, -1.000000000000000000 ) ) ;
#27725 = CARTESIAN_POINT ( 'NONE',  ( 41.48619405471883681, -151.3359592902621955, -1.950000000000163380 ) ) ;
#27724 = CARTESIAN_POINT ( 'NONE',  ( -61.61493949811855231, -2.667984932540325094, 0.4224978793964678236 ) ) ;
#27726 = AXIS2_PLACEMENT_3D ( 'NONE', #16657, #28681, #25970 ) ;
#27727 = CIRCLE ( 'NONE', #22684, 0.04999999999999449329 ) ;
#27728 = CARTESIAN_POINT ( 'NONE',  ( -44.49999999999996447, 1.400000000000023670, -3.959797974644836405 ) ) ;
#27729 = DIRECTION ( 'NONE',  ( 1.000000000000000000, 1.047444401652940007E-14, 0.000000000000000000 ) ) ;
#27731 = CARTESIAN_POINT ( 'NONE',  ( 51.73328143279135105, 4.175271471638106746, -1.930573136446366300 ) ) ;
#27730 = FACE_OUTER_BOUND ( 'NONE', #13945, .T. ) ;
#27732 = ORIENTED_EDGE ( 'NONE', *, *, #23755, .F. ) ;
#27733 = CARTESIAN_POINT ( 'NONE',  ( 50.34896831693479413, -1.383117500627048635, -3.859810431918047957 ) ) ;
#27734 = DIRECTION ( 'NONE',  ( 1.000000000000000000, 1.047444401652940007E-14, 0.000000000000000000 ) ) ;
#27736 = DIRECTION ( 'NONE',  ( 0.000000000000000000, -1.000000000000000000, -4.379659758543256221E-15 ) ) ;
#27735 = CARTESIAN_POINT ( 'NONE',  ( 58.73371041428909933, 1.788808215312048588, 0.5624054559947927467 ) ) ;
#27737 = CARTESIAN_POINT ( 'NONE',  ( 59.00000000000002132, 1.401298464324817071E-42, -6.179921969752347932E-13 ) ) ;
#27738 = ORIENTED_EDGE ( 'NONE', *, *, #30350, .T. ) ;
#27739 = CARTESIAN_POINT ( 'NONE',  ( 54.23625105546378933, 6.534957249981562022, 2.049999999999810640 ) ) ;
#27740 = DIRECTION ( 'NONE',  ( 1.000000000000000000, 0.000000000000000000, 0.000000000000000000 ) ) ;
#27741 = EDGE_CURVE ( 'NONE', #19028, #28904, #15997, .T. ) ;
#27742 = ORIENTED_EDGE ( 'NONE', *, *, #29746, .T. ) ;
#27743 = ORIENTED_EDGE ( 'NONE', *, *, #16679, .T. ) ;
#27744 = DIRECTION ( 'NONE',  ( 2.581436205204234499E-16, -0.9796124928211140670, -0.2008964009354146651 ) ) ;
#27745 = CARTESIAN_POINT ( 'NONE',  ( 69.20000000000004547, 0.7500000000000000000, 1.988246715072631732 ) ) ;
#27746 = VERTEX_POINT ( 'NONE', #4443 ) ;
#27747 = B_SPLINE_CURVE_WITH_KNOTS ( 'NONE', 3,
 ( #18185, #27827, #6135, #15787, #13556, #25436, #18330, #3739, #6601, #20717, #13381, #30344, #23078, #1374, #11187, #8651, #27967, #6280, #15928, #30489, #25589, #6447, #3908, #23239, #16108, #23712, #31292, #17057, #4372, #9910, #28601, #11817, #6919, #24009, #26530, #2631 ),
 .UNSPECIFIED., .F., .F.,
 ( 4, 2, 2, 2, 2, 2, 2, 2, 2, 2, 2, 2, 2, 2, 2, 2, 2, 4 ),
 ( 0.000000000000000000, 0.001741378360725073316, 0.002612067541087599674, 0.003047412131268863178, 0.003482756721450126249, 0.004353445901812643716, 0.005224135082175161184, 0.006965513442900206527, 0.007836202623262724862, 0.008706891803625242329, 0.009577580983987759797, 0.01044827016435027900, 0.01131895934471279647, 0.01218964852507531393, 0.01262499311525657093, 0.01306033770543782620, 0.01349568229561908320, 0.01393102688580033846 ),
 .UNSPECIFIED. ) ;
#27748 = FACE_OUTER_BOUND ( 'NONE', #28435, .T. ) ;
#27749 = CARTESIAN_POINT ( 'NONE',  ( -59.08155989232413674, -1.962990915244731571, 3.399999999999781419 ) ) ;
#27750 = ORIENTED_EDGE ( 'NONE', *, *, #30930, .F. ) ;
#27751 = DIRECTION ( 'NONE',  ( 1.000000000000000000, 0.000000000000000000, 4.738179285253022937E-16 ) ) ;
#27752 = EDGE_LOOP ( 'NONE', ( #11331, #18145, #24010, #23006 ) ) ;
#27753 = ORIENTED_EDGE ( 'NONE', *, *, #8505, .F. ) ;
#27754 = STYLED_ITEM ( 'NONE', ( #1290 ), #10428 ) ;
#27755 = CIRCLE ( 'NONE', #29762, 0.05000000000000017625 ) ;
#27756 = EDGE_CURVE ( 'NONE', #12845, #10038, #5399, .T. ) ;
#27757 = CARTESIAN_POINT ( 'NONE',  ( -55.56249999999998579, -1.962990915244731793, 3.399999999999794742 ) ) ;
#27758 = CARTESIAN_POINT ( 'NONE',  ( 36.50000000000002132, 0.8000000000000000444, -1.778341924377873751 ) ) ;
#27759 = DIRECTION ( 'NONE',  ( 0.000000000000000000, 0.000000000000000000, 1.000000000000000000 ) ) ;
#27760 = FACE_OUTER_BOUND ( 'NONE', #28558, .T. ) ;
#27761 = CARTESIAN_POINT ( 'NONE',  ( -44.49999999999997868, -1.399999999999992806, -1.638709930773317737E-13 ) ) ;
#27763 = CARTESIAN_POINT ( 'NONE',  ( -54.62499999999997868, 2.489203624310591501, -2.804704140674918467 ) ) ;
#27762 = DIRECTION ( 'NONE',  ( 0.000000000000000000, -0.2008964009354148039, 0.9796124928211140670 ) ) ;
#27764 = CIRCLE ( 'NONE', #14108, 1.000000000000000000 ) ;
#27765 = DIRECTION ( 'NONE',  ( 1.000000000000000000, 0.000000000000000000, 0.000000000000000000 ) ) ;
#27766 = CYLINDRICAL_SURFACE ( 'NONE', #11450, 3.750000000000000444 ) ;
#27767 = LINE ( 'NONE', #1161, #3344 ) ;
#27768 = CARTESIAN_POINT ( 'NONE',  ( -54.49454330418567594, 1.526701536696945638, -3.317245250669464518 ) ) ;
#27769 = DIRECTION ( 'NONE',  ( 1.000000000000000000, 0.000000000000000000, -0.000000000000000000 ) ) ;
#27770 = EDGE_LOOP ( 'NONE', ( #9128, #2800, #19361, #3164 ) ) ;
#27771 = DIRECTION ( 'NONE',  ( 0.000000000000000000, 0.000000000000000000, -1.000000000000000000 ) ) ;
#27772 = PRESENTATION_STYLE_ASSIGNMENT (( #10990 ) ) ;
#27773 = AXIS2_PLACEMENT_3D ( 'NONE', #3496, #17899, #27538 ) ;
#27774 = ORIENTED_EDGE ( 'NONE', *, *, #19750, .T. ) ;
#27775 = AXIS2_PLACEMENT_3D ( 'NONE', #16172, #13765, #23451 ) ;
#27776 = ADVANCED_FACE ( 'NONE', ( #28507 ), #1581, .T. ) ;
#27777 = ORIENTED_EDGE ( 'NONE', *, *, #24895, .F. ) ;
#27778 = DIRECTION ( 'NONE',  ( 1.000000000000000000, 0.000000000000000000, 0.000000000000000000 ) ) ;
#27779 = PRODUCT_DEFINITION_SHAPE ( 'NONE', 'NONE',  #31336 ) ;
#27780 = CARTESIAN_POINT ( 'NONE',  ( 61.25000000000001421, 1.000000000000641709, -1.586072192556190474 ) ) ;
#27782 = CARTESIAN_POINT ( 'NONE',  ( -59.52159998169275923, 2.135188160778345612, 1.581460861012937924 ) ) ;
#27781 = CARTESIAN_POINT ( 'NONE',  ( -56.99999999999997158, -2.944486372867089141, 1.699999999999786571 ) ) ;
#27783 = EDGE_CURVE ( 'NONE', #9283, #23396, #23112, .T. ) ;
#27784 = ORIENTED_EDGE ( 'NONE', *, *, #20495, .T. ) ;
#27785 = ORIENTED_EDGE ( 'NONE', *, *, #25003, .T. ) ;
#27786 = DIRECTION ( 'NONE',  ( -0.000000000000000000, -0.000000000000000000, -1.000000000000000000 ) ) ;
#27787 = EDGE_LOOP ( 'NONE', ( #6550, #18436, #4993, #6704 ) ) ;
#27788 = CARTESIAN_POINT ( 'NONE',  ( 36.55000000000001847, 0.000000000000000000, -1.850000000000000089 ) ) ;
#27789 = ORIENTED_EDGE ( 'NONE', *, *, #28236, .F. ) ;
#27790 = CARTESIAN_POINT ( 'NONE',  ( 60.99723038499097783, 0.5606956656655598392, 1.857935671878364614 ) ) ;
#27791 = DIRECTION ( 'NONE',  ( 0.000000000000000000, -1.000000000000000000, -3.491481338843133355E-15 ) ) ;
#27792 = DIRECTION ( 'NONE',  ( 1.000000000000000000, 1.047444401652940007E-14, 0.000000000000000000 ) ) ;
#27793 = ORIENTED_EDGE ( 'NONE', *, *, #9024, .F. ) ;
#27794 = EDGE_CURVE ( 'NONE', #1478, #8275, #25102, .T. ) ;
#27795 = VECTOR ( 'NONE', #4417, 1000.000000000000000 ) ;
#27796 = CARTESIAN_POINT ( 'NONE',  ( 47.04662468001162523, -4.276948325786881888, -0.9210526687159725778 ) ) ;
#27797 = CARTESIAN_POINT ( 'NONE',  ( 58.75000000000000711, 1.470078920828144620, -1.470078920826818125 ) ) ;
#27798 = CARTESIAN_POINT ( 'NONE',  ( -60.39405989232410121, -2.944486372867076263, -1.700000000000224665 ) ) ;
#27799 = CARTESIAN_POINT ( 'NONE',  ( 47.00000000000002842, -3.700146292169669948, 1.985065161562699299 ) ) ;
#27800 = PRODUCT_DEFINITION_FORMATION_WITH_SPECIFIED_SOURCE ( 'ANY', '', #11652, .NOT_KNOWN. ) ;
#27801 = CARTESIAN_POINT ( 'NONE',  ( 58.65844932252339561, 1.302247349114951991, 1.349094575299514931 ) ) ;
#27802 = CIRCLE ( 'NONE', #25263, 159.6997717543496833 ) ;
#27803 = DIRECTION ( 'NONE',  ( -1.000000000000000000, -0.000000000000000000, -0.000000000000000000 ) ) ;
#27804 = VECTOR ( 'NONE', #29775, 1000.000000000000000 ) ;
#27805 = CARTESIAN_POINT ( 'NONE',  ( 53.97784470437120774, 5.744339954850582686, -2.010804190376556555 ) ) ;
#27807 = CARTESIAN_POINT ( 'NONE',  ( 51.80000000000003268, -4.020776289669856673, 2.234582293948397691 ) ) ;
#27806 = CARTESIAN_POINT ( 'NONE',  ( 61.25000000000002132, 6.415596960124259844E-13, 3.111507638930570854E-58 ) ) ;
#27808 = EDGE_CURVE ( 'NONE', #1827, #28152, #12962, .T. ) ;
#27809 = TOROIDAL_SURFACE ( 'NONE', #497, 4.500000000000037303, 0.1000000000000000056 ) ;
#27810 = DIRECTION ( 'NONE',  ( 0.000000000000000000, 0.000000000000000000, 1.000000000000000000 ) ) ;
#27811 = CYLINDRICAL_SURFACE ( 'NONE', #897, 160.6997717543497686 ) ;
#27812 = DIRECTION ( 'NONE',  ( 1.000000000000000000, 1.047444401652940007E-14, -0.000000000000000000 ) ) ;
#27813 = ORIENTED_EDGE ( 'NONE', *, *, #16946, .F. ) ;
#27814 = CARTESIAN_POINT ( 'NONE',  ( 54.31535763113295445, 6.000143968236459457, -2.050000000000189004 ) ) ;
#27815 = EDGE_LOOP ( 'NONE', ( #16866, #7851, #1549 ) ) ;
#27816 = EDGE_CURVE ( 'NONE', #18829, #779, #23298, .T. ) ;
#27817 = CARTESIAN_POINT ( 'NONE',  ( -59.19126343180466421, -2.406052454186071277, 1.245092465133171844 ) ) ;
#27818 = VERTEX_POINT ( 'NONE', #4121 ) ;
#27819 = EDGE_CURVE ( 'NONE', #31054, #24915, #20092, .T. ) ;
#27820 = DIRECTION ( 'NONE',  ( 1.000000000000000000, 3.053848253006669023E-16, -2.042510438544995415E-16 ) ) ;
#27821 = ADVANCED_BREP_SHAPE_REPRESENTATION ( '', ( #15127, #9018 ), #18147 ) ;
#27822 = CARTESIAN_POINT ( 'NONE',  ( -57.47085481156722864, -3.673546848079175753, -0.7533615035078066180 ) ) ;
#27824 = DIRECTION ( 'NONE',  ( 0.000000000000000000, 1.000000000000000000, 0.000000000000000000 ) ) ;
#27823 = CARTESIAN_POINT ( 'NONE',  ( 60.97860563121706434, -0.7618031158890644639, 1.436139941719672075 ) ) ;
#27825 = EDGE_CURVE ( 'NONE', #23465, #8800, #29161, .T. ) ;
#27826 = EDGE_LOOP ( 'NONE', ( #668, #23672 ) ) ;
#27827 = CARTESIAN_POINT ( 'NONE',  ( 33.97286272917381922, 8.288178785419178851, -2.050000000000117506 ) ) ;
#27828 = DIRECTION ( 'NONE',  ( 1.000000000000000000, 1.047444401652940007E-14, 0.000000000000000000 ) ) ;
#27829 = VERTEX_POINT ( 'NONE', #19338 ) ;
#27831 = CARTESIAN_POINT ( 'NONE',  ( -35.85663232820584057, -1.793057972834796621, -4.026191436120394762 ) ) ;
#27830 = SPHERICAL_SURFACE ( 'NONE', #8493, 0.2500000000000000000 ) ;
#27832 = DIRECTION ( 'NONE',  ( 0.000000000000000000, 0.000000000000000000, 1.000000000000000000 ) ) ;
#27833 = ORIENTED_EDGE ( 'NONE', *, *, #2782, .T. ) ;
#27834 = CARTESIAN_POINT ( 'NONE',  ( -36.89017861347081606, 5.034707333629178549, -1.977875755500439148 ) ) ;
#27835 = CARTESIAN_POINT ( 'NONE',  ( -62.29999999999998295, 1.106939637198029038E-15, 2.238576962872695299E-15 ) ) ;
#27836 = AXIS2_PLACEMENT_3D ( 'NONE', #16549, #9591, #19088 ) ;
#27837 = CARTESIAN_POINT ( 'NONE',  ( -36.52679053911622020, -3.858136107555833583, 3.790289750283442505 ) ) ;
#27838 = CARTESIAN_POINT ( 'NONE',  ( 56.99229849798533820, 0.7794861535680733811, 1.732743875013533108 ) ) ;
#27839 = CARTESIAN_POINT ( 'NONE',  ( -54.44702994616203995, -2.078460969082631227, -3.600000000000199485 ) ) ;
#27840 = VERTEX_POINT ( 'NONE', #17403 ) ;
#27841 =( BOUNDED_SURFACE ( )  B_SPLINE_SURFACE ( 3, 2, ( 
 ( #18785, #25889, #11649 ),
 ( #23993, #16564, #4192 ),
 ( #14320, #30961, #9276 ),
 ( #26211, #13829, #6732 ),
 ( #9602, #19262, #6426 ),
 ( #16086, #25738, #4046 ),
 ( #13689, #23370, #1650 ),
 ( #28428, #11309, #29494 ),
 ( #7667, #15102, #17326 ),
 ( #22397, #17485, #26832 ),
 ( #9891, #5134, #19406 ),
 ( #26972, #687, #29212 ),
 ( #21797, #21945, #12563 ),
 ( #12406, #3072, #7809 ),
 ( #17035, #7525, #27133 ),
 ( #14934, #12118, #5280 ) ),
 .UNSPECIFIED., .F., .F., .T. ) 
 B_SPLINE_SURFACE_WITH_KNOTS ( ( 4, 2, 2, 2, 2, 2, 2, 4 ),
 ( 3, 3 ),
 ( 0.001780502285214260842, 0.002558945925323795421, 0.002753556835351178740, 0.002948167745378562493, 0.003337389565433329999, 0.003726611385488097505, 0.004115833205542865011, 0.004894276845652399156 ),
 ( 0.000000000000000000, 1.000000000000000000 ),
 .UNSPECIFIED. ) 
 GEOMETRIC_REPRESENTATION_ITEM ( )  RATIONAL_B_SPLINE_SURFACE ( (
 ( 1.000000000000000000, 0.9418517008537223845, 1.000000000000000000),
 ( 1.000000000000000000, 0.9417987965885066259, 1.000000000000000000),
 ( 1.000000000000000000, 0.9418198861734071725, 1.000000000000000000),
 ( 1.000000000000000000, 0.9434060303845559492, 1.000000000000000000),
 ( 1.000000000000000000, 0.9437939819948627518, 1.000000000000000000),
 ( 1.000000000000000000, 0.9445989566712328367, 1.000000000000000000),
 ( 1.000000000000000000, 0.9450169930049197031, 1.000000000000000000),
 ( 1.000000000000000000, 0.9461610507674824699, 1.000000000000000000),
 ( 1.000000000000000000, 0.9467217966428496112, 1.000000000000000000),
 ( 1.000000000000000000, 0.9467345476123045778, 1.000000000000000000),
 ( 1.000000000000000000, 0.9461964028052702869, 1.000000000000000000),
 ( 1.000000000000000000, 0.9446801822474044652, 1.000000000000000000),
 ( 1.000000000000000000, 0.9437582546536025241, 1.000000000000000000),
 ( 1.000000000000000000, 0.9418129560296703007, 1.000000000000000000),
 ( 1.000000000000000000, 0.9418016889776684719, 1.000000000000000000),
 ( 1.000000000000000000, 0.9418517008537214963, 1.000000000000000000) ) ) 
 REPRESENTATION_ITEM ( '' )  SURFACE ( )  );
#27842 = CARTESIAN_POINT ( 'NONE',  ( 15.41586008885044912, 3.272294129011773745, 4.050092634494075305 ) ) ;
#27843 = EDGE_CURVE ( 'NONE', #28852, #1336, #13476, .T. ) ;
#27844 = CARTESIAN_POINT ( 'NONE',  ( -54.79792740578361077, -2.256877952708263191, 2.542931754211923856 ) ) ;
#27846 = ADVANCED_FACE ( 'NONE', ( #5365 ), #7932, .T. ) ;
#27845 = CARTESIAN_POINT ( 'NONE',  ( 51.75429853018303561, -4.276948333784438283, 0.9210526315789470120 ) ) ;
#27847 = B_SPLINE_CURVE_WITH_KNOTS ( 'NONE', 3,
 ( #9794, #3133, #17241, #26881, #10411, #12774, #22455, #19462, #26746, #14839, #7424, #20095, #4883, #14548, #24212, #24500, #2525, #5045, #12174 ),
 .UNSPECIFIED., .F., .F.,
 ( 4, 3, 3, 3, 3, 3, 4 ),
 ( 0.000000000000000000, 1.462084321540209121E-05, 2.917085440492037316E-05, 4.467649728434973632E-05, 6.285390091960512901E-05, 8.531547445983615763E-05, 8.677858956768834506E-05 ),
 .UNSPECIFIED. ) ;
#27848 = CARTESIAN_POINT ( 'NONE',  ( 60.97363240180333577, -0.7541976959271894376, -1.440084173506624765 ) ) ;
#27850 = AXIS2_PLACEMENT_3D ( 'NONE', #22084, #676, #27121 ) ;
#27849 = CARTESIAN_POINT ( 'NONE',  ( 58.75000000000004263, -1.972190280207122726, 0.1053114364788733381 ) ) ;
#27851 = CARTESIAN_POINT ( 'NONE',  ( 29.17657462828753268, 6.106387485306473906, 2.049999999999898570 ) ) ;
#27852 = VERTEX_POINT ( 'NONE', #26764 ) ;
#27853 = CARTESIAN_POINT ( 'NONE',  ( 58.64999999999999858, 1.671477153794443504, 0.8495817349409569008 ) ) ;
#27854 = ORIENTED_EDGE ( 'NONE', *, *, #19717, .F. ) ;
#27855 = DIRECTION ( 'NONE',  ( 0.000000000000000000, 0.9996898646859343485, 0.02490330187381123786 ) ) ;
#27857 = DIRECTION ( 'NONE',  ( -3.023770467182126270E-15, -0.4999707644721522182, -0.8660422822663637055 ) ) ;
#27856 = CARTESIAN_POINT ( 'NONE',  ( 57.00000000000001421, 0.6999999999999999556, -2.452039967047845437 ) ) ;
#27858 = EDGE_LOOP ( 'NONE', ( #14765, #29503 ) ) ;
#27859 = ORIENTED_EDGE ( 'NONE', *, *, #22069, .T. ) ;
#27860 = FACE_OUTER_BOUND ( 'NONE', #8933, .T. ) ;
#27862 = FACE_OUTER_BOUND ( 'NONE', #3439, .T. ) ;
#27861 = CARTESIAN_POINT ( 'NONE',  ( -44.59999999999996589, 1.557046979865791769, -3.273565289175096815 ) ) ;
#27863 = CARTESIAN_POINT ( 'NONE',  ( -56.29792740578360366, -2.256877952708263635, 2.542931754211924300 ) ) ;
#27864 = LINE ( 'NONE', #20757, #2588 ) ;
#27865 = DIRECTION ( 'NONE',  ( -9.754918421198722508E-16, 0.9601771338024398528, -0.2793919678926571337 ) ) ;
#27866 = ORIENTED_EDGE ( 'NONE', *, *, #3366, .T. ) ;
#27867 = B_SPLINE_CURVE_WITH_KNOTS ( 'NONE', 3,
 ( #22023, #22334, #4916, #17264, #10445, #15036, #9822, #26604, #24695, #316, #26909, #7907, #3159 ),
 .UNSPECIFIED., .F., .F.,
 ( 4, 3, 3, 3, 4 ),
 ( 0.000000000000000000, 3.315084464037111269E-05, 6.626473632988943725E-05, 9.991171812031440650E-05, 0.0001104636331259644592 ),
 .UNSPECIFIED. ) ;
#27868 = CARTESIAN_POINT ( 'NONE',  ( -60.38452994616202574, 2.093608279459374244E-14, -3.600000000000214140 ) ) ;
#27869 = CARTESIAN_POINT ( 'NONE',  ( 52.41186875581714588, 8.643425072357743488, -2.050000000000182343 ) ) ;
#27870 = CARTESIAN_POINT ( 'NONE',  ( 15.29449157529479031, 0.3981319440499709872, 5.199999999410283458 ) ) ;
#27871 = ADVANCED_FACE ( 'NONE', ( #15026 ), #5067, .T. ) ;
#27872 = EDGE_CURVE ( 'NONE', #14808, #28206, #16634, .T. ) ;
#27873 = CARTESIAN_POINT ( 'NONE',  ( -56.56249999999997158, -0.7533615035078050637, 3.673546848079176641 ) ) ;
#27876 = EDGE_CURVE ( 'NONE', #27852, #91, #23609, .T. ) ;
#27875 = FACE_OUTER_BOUND ( 'NONE', #990, .T. ) ;
#27874 = CARTESIAN_POINT ( 'NONE',  ( -56.59599364905386665, 3.400000000000011902, -0.9110272542659995088 ) ) ;
#27877 = CARTESIAN_POINT ( 'NONE',  ( 53.02518193390453405, 4.240975178678276336, -2.047385601739696082 ) ) ;
#27879 = CARTESIAN_POINT ( 'NONE',  ( -62.34999999999997300, 1.091670395932995432E-15, 2.248789515065420326E-15 ) ) ;
#27878 = CARTESIAN_POINT ( 'NONE',  ( 58.50000000000001421, -0.8000000000000000444, -1.745709025009608784 ) ) ;
#27880 = VERTEX_POINT ( 'NONE', #2690 ) ;
#27881 = AXIS2_PLACEMENT_3D ( 'NONE', #20730, #3610, #30358 ) ;
#27882 = LINE ( 'NONE', #20923, #30087 ) ;
#27883 = DIRECTION ( 'NONE',  ( 1.000000000000000000, 0.000000000000000000, 0.000000000000000000 ) ) ;
#27885 = CARTESIAN_POINT ( 'NONE',  ( 58.66133336607612137, -0.9657121834148485462, -1.607522887371789722 ) ) ;
#27884 = DIRECTION ( 'NONE',  ( 1.000000000000000000, 3.053848253006669023E-16, -2.042510438544995415E-16 ) ) ;
#27886 = DIRECTION ( 'NONE',  ( 0.000000000000000000, 0.000000000000000000, 1.000000000000000000 ) ) ;
#27887 = ORIENTED_EDGE ( 'NONE', *, *, #25639, .T. ) ;
#27888 = CARTESIAN_POINT ( 'NONE',  ( 54.24037840390755605, 6.535103219670295616, 2.049999999999810640 ) ) ;
#27889 = CARTESIAN_POINT ( 'NONE',  ( -60.60352959746391122, -2.443263361361769803, -1.074417906603847728 ) ) ;
#27890 = SHAPE_REPRESENTATION ( 'End Cap Ring', ( #9018 ), #25740 ) ;
#27891 = EDGE_CURVE ( 'NONE', #27064, #67, #12329, .T. ) ;
#27892 = EDGE_LOOP ( 'NONE', ( #11842, #19257, #22624, #17319 ) ) ;
#27893 =( BOUNDED_CURVE ( )  B_SPLINE_CURVE ( 2, ( #4038, #26034, #4512, #23214, #23690, #4185, #1807, #30796, #9107 ),
 .UNSPECIFIED., .F., .T. ) 
 B_SPLINE_CURVE_WITH_KNOTS ( ( 3, 2, 2, 2, 3 ),
 ( 0.08333333333333332871, 0.09259259259259258745, 0.1111111111111111049, 0.1296296296296296224, 0.1388888888888888951 ),
 .UNSPECIFIED. ) 
 CURVE ( )  GEOMETRIC_REPRESENTATION_ITEM ( )  RATIONAL_B_SPLINE_CURVE ( ( 0.9330127018922194093, 0.9330127018922194093, 1.000000000000000000, 0.8660254037844387076, 1.000000000000000000, 0.8660254037844387076, 1.000000000000000000, 0.9330127018922191873, 0.9330127018922192983 ) ) 
 REPRESENTATION_ITEM ( '' )  );
#27894 = CARTESIAN_POINT ( 'NONE',  ( 47.00000000000002132, -3.726179070414207928, -1.100000000000000089 ) ) ;
#27895 = ORIENTED_EDGE ( 'NONE', *, *, #399, .T. ) ;
#27896 = CARTESIAN_POINT ( 'NONE',  ( 51.25000000000002842, -1.487499999999464029, 1.821662113731689224E-16 ) ) ;
#27897 = DIRECTION ( 'NONE',  ( 0.000000000000000000, -1.224646799146977512E-16, 1.000000000000000000 ) ) ;
#27898 = ORIENTED_EDGE ( 'NONE', *, *, #8648, .T. ) ;
#27899 = CARTESIAN_POINT ( 'NONE',  ( -54.48926665517993229, -2.780759778332207777, -2.383582780284819513 ) ) ;
#27900 = CARTESIAN_POINT ( 'NONE',  ( -59.51905989232410121, 2.023778652682510314E-14, -3.400000000000210854 ) ) ;
#27901 = EDGE_LOOP ( 'NONE', ( #2471, #21405, #18979, #12241, #11300, #7703 ) ) ;
#27902 = CARTESIAN_POINT ( 'NONE',  ( 56.95000000000001705, 0.6820512820512819596, -1.773360101234998210 ) ) ;
#27903 = EDGE_LOOP ( 'NONE', ( #20755, #6681, #18838, #12431 ) ) ;
#27904 = VERTEX_POINT ( 'NONE', #3000 ) ;
#27905 = AXIS2_PLACEMENT_3D ( 'NONE', #11225, #20900, #30530 ) ;
#27906 = AXIS2_PLACEMENT_3D ( 'NONE', #15984, #17759, #27397 ) ;
#27907 = CARTESIAN_POINT ( 'NONE',  ( -56.06249999999995737, -1.962990915244707368, -3.400000000000206413 ) ) ;
#27908 = FACE_OUTER_BOUND ( 'NONE', #23076, .T. ) ;
#27909 = CARTESIAN_POINT ( 'NONE',  ( -62.06710100716625789, -2.517118187348250213, 0.1993515260053453086 ) ) ;
#27910 = DIRECTION ( 'NONE',  ( -0.5633368246415004776, -0.8262273428075539439, 0.000000000000000000 ) ) ;
#27911 = LINE ( 'NONE', #18421, #5442 ) ;
#27912 = EDGE_CURVE ( 'NONE', #16106, #13475, #22612, .T. ) ;
#27914 = DIRECTION ( 'NONE',  ( -1.000000000000000000, -0.000000000000000000, 3.491481338843133355E-15 ) ) ;
#27913 = CARTESIAN_POINT ( 'NONE',  ( 15.03925126672132784, 3.817150320980686296, -2.203324261490496205 ) ) ;
#27915 = CARTESIAN_POINT ( 'NONE',  ( -62.04999999999998295, -2.687391533643777919, 0.2606275981160458555 ) ) ;
#27916 = DIRECTION ( 'NONE',  ( 0.000000000000000000, 0.000000000000000000, -1.000000000000000000 ) ) ;
#27917 = CARTESIAN_POINT ( 'NONE',  ( 54.19028661868582475, 6.697846887293304796, 2.049999999999810640 ) ) ;
#27918 = CARTESIAN_POINT ( 'NONE',  ( 50.55258015808398397, -0.05185913279167173734, 1.177580158083963324 ) ) ;
#27919 = DIRECTION ( 'NONE',  ( 0.000000000000000000, 0.000000000000000000, 1.000000000000000000 ) ) ;
#27920 = ORIENTED_EDGE ( 'NONE', *, *, #20299, .T. ) ;
#27921 = FACE_OUTER_BOUND ( 'NONE', #25643, .T. ) ;
#27922 = CARTESIAN_POINT ( 'NONE',  ( -36.89831264271882105, -0.2888463313200454463, -5.401384060636567064 ) ) ;
#27923 = EDGE_CURVE ( 'NONE', #5901, #21780, #9678, .T. ) ;
#27924 = ORIENTED_EDGE ( 'NONE', *, *, #24504, .F. ) ;
#27925 = FACE_OUTER_BOUND ( 'NONE', #1100, .T. ) ;
#27926 = FACE_OUTER_BOUND ( 'NONE', #29142, .T. ) ;
#27928 = DIRECTION ( 'NONE',  ( 2.614375865348240525E-16, -0.2008964009354147762, 0.9796124928211140670 ) ) ;
#27927 = CARTESIAN_POINT ( 'NONE',  ( -58.56249999999997868, -1.962990915244731793, 3.399999999999783640 ) ) ;
#27929 = ORIENTED_EDGE ( 'NONE', *, *, #4581, .T. ) ;
#27930 = ORIENTED_EDGE ( 'NONE', *, *, #12922, .F. ) ;
#27931 = CARTESIAN_POINT ( 'NONE',  ( -59.29999999999997584, 2.330309927981285032E-15, 4.253626757584724400E-16 ) ) ;
#27932 = VERTEX_POINT ( 'NONE', #16802 ) ;
#27933 = CARTESIAN_POINT ( 'NONE',  ( 58.75000000000003553, -1.749295403804336013, 0.8980135333491227057 ) ) ;
#27934 = ORIENTED_EDGE ( 'NONE', *, *, #3153, .T. ) ;
#27935 = CARTESIAN_POINT ( 'NONE',  ( 22.32354329814768334, 7.018810584857617663, -1.950000000000043698 ) ) ;
#27936 = AXIS2_PLACEMENT_3D ( 'NONE', #5194, #7121, #12028 ) ;
#27937 = CARTESIAN_POINT ( 'NONE',  ( -59.18749999999996447, 0.7533615035078157218, -3.673546848079175309 ) ) ;
#27938 = DIRECTION ( 'NONE',  ( -1.000000000000000000, -3.053848253006669023E-16, 2.042510438544995169E-16 ) ) ;
#27939 = ORIENTED_EDGE ( 'NONE', *, *, #17070, .F. ) ;
#27940 = CARTESIAN_POINT ( 'NONE',  ( 47.10000000000002274, -4.276948333784442724, -0.9210526315789473450 ) ) ;
#27941 = DIRECTION ( 'NONE',  ( -0.9993908270190956511, 0.03489949670250089980, 3.469446951951485842E-15 ) ) ;
#27942 = CARTESIAN_POINT ( 'NONE',  ( 51.16322638839886849, -0.9520444587745244824, 1.480281041496170902 ) ) ;
#27943 = CARTESIAN_POINT ( 'NONE',  ( 52.98236138753792801, 8.264679131573696935, -1.919164453910518375 ) ) ;
#27944 = CARTESIAN_POINT ( 'NONE',  ( 15.70940947763170215, 3.858136107555762528, 3.790289750283494019 ) ) ;
#27945 = EDGE_CURVE ( 'NONE', #13205, #11230, #8943, .T. ) ;
#27946 = CARTESIAN_POINT ( 'NONE',  ( -59.19545262082412762, -2.415331713986693885, 1.247511094541249976 ) ) ;
#27947 = CARTESIAN_POINT ( 'NONE',  ( 58.65000000000004121, -1.972190280207337443, -0.1053114364790862928 ) ) ;
#27949 = DIRECTION ( 'NONE',  ( 1.000000000000000000, -1.219044193948983948E-29, 3.491481338843133355E-15 ) ) ;
#27948 = DIRECTION ( 'NONE',  ( 1.000000000000000000, 1.047444401652940007E-14, 0.000000000000000000 ) ) ;
#27950 = CARTESIAN_POINT ( 'NONE',  ( -54.49999999999997868, 3.796242339859525868E-15, -5.550248518040434488E-16 ) ) ;
#27951 = CARTESIAN_POINT ( 'NONE',  ( 58.65000000000000568, 1.394635017528131904, 1.253243060178682144 ) ) ;
#27952 = FACE_OUTER_BOUND ( 'NONE', #14290, .T. ) ;
#27953 = AXIS2_PLACEMENT_3D ( 'NONE', #3122, #27193, #7863 ) ;
#27954 = VERTEX_POINT ( 'NONE', #2385 ) ;
#27955 = CARTESIAN_POINT ( 'NONE',  ( 52.20711756518981872, -0.7499999999994703126, -1.718465885608432941 ) ) ;
#27956 = VERTEX_POINT ( 'NONE', #7447 ) ;
#27957 = ORIENTED_EDGE ( 'NONE', *, *, #25683, .F. ) ;
#27958 = EDGE_CURVE ( 'NONE', #590, #29022, #17041, .T. ) ;
#27959 = DIRECTION ( 'NONE',  ( 0.000000000000000000, 0.000000000000000000, 1.000000000000000000 ) ) ;
#27960 = ORIENTED_EDGE ( 'NONE', *, *, #28279, .F. ) ;
#27961 = CARTESIAN_POINT ( 'NONE',  ( 54.16371155698127637, 6.950779743548840983, 2.049999999999811973 ) ) ;
#27962 = CARTESIAN_POINT ( 'NONE',  ( -56.28335481156724285, 3.238593381231848145, 2.874284765127022467 ) ) ;
#27964 = DIRECTION ( 'NONE',  ( 0.000000000000000000, 0.000000000000000000, 1.000000000000000000 ) ) ;
#27963 = LINE ( 'NONE', #28120, #23634 ) ;
#27965 = ORIENTED_EDGE ( 'NONE', *, *, #19183, .F. ) ;
#27966 = ORIENTED_EDGE ( 'NONE', *, *, #1930, .F. ) ;
#27967 = CARTESIAN_POINT ( 'NONE',  ( 27.52372483455771857, 5.460843285065334562, -2.050000000000095746 ) ) ;
#27968 = DIRECTION ( 'NONE',  ( -1.000000000000000000, -3.053848253006669023E-16, 2.042510438544995415E-16 ) ) ;
#27969 = ORIENTED_EDGE ( 'NONE', *, *, #2726, .F. ) ;
#27971 = FACE_OUTER_BOUND ( 'NONE', #24697, .T. ) ;
#27970 = DIRECTION ( 'NONE',  ( -3.489354422748178188E-15, 1.218509414717996091E-16, -1.000000000000000000 ) ) ;
#27972 = CARTESIAN_POINT ( 'NONE',  ( -56.20655989232413674, 1.962990915244719359, 3.399999999999808509 ) ) ;
#27973 = ORIENTED_EDGE ( 'NONE', *, *, #22207, .F. ) ;
#27974 = CARTESIAN_POINT ( 'NONE',  ( -35.85663232820592583, 5.086913985776147840, -1.171642053949061291 ) ) ;
#27975 = EDGE_CURVE ( 'NONE', #29651, #15816, #21723, .T. ) ;
#27976 = CARTESIAN_POINT ( 'NONE',  ( 58.75000000000003553, -1.470078920827915470, 1.470078920827824209 ) ) ;
#27977 = CARTESIAN_POINT ( 'NONE',  ( 51.80000000000001137, 6.475000000000062705, -2.050000000000180123 ) ) ;
#27979 = CARTESIAN_POINT ( 'NONE',  ( 69.20000000000001705, 0.7500000000000000000, -2.238246715074081017 ) ) ;
#27978 = CIRCLE ( 'NONE', #9774, 0.1499999999999999667 ) ;
#27980 = AXIS2_PLACEMENT_3D ( 'NONE', #11097, #15230, #24875 ) ;
#27981 = ADVANCED_FACE ( 'NONE', ( #24069 ), #12656, .F. ) ;
#27982 = CARTESIAN_POINT ( 'NONE',  ( -58.43749999999997158, -3.399999999999991029, -2.253785087031484148E-13 ) ) ;
#27983 = ADVANCED_FACE ( 'NONE', ( #29751 ), #17733, .F. ) ;
#27984 = CARTESIAN_POINT ( 'NONE',  ( -58.67292740578360366, 1.073804522883500701, 3.225979517392344231 ) ) ;
#27985 = APPLICATION_CONTEXT ( 'automotive_design' ) ;
#27986 = CARTESIAN_POINT ( 'NONE',  ( -56.72085481156723574, -3.673546848079175753, -0.7533615035078068400 ) ) ;
#27987 = DIRECTION ( 'NONE',  ( -3.489354422748178582E-15, 1.218509414717996338E-16, -1.000000000000000000 ) ) ;
#27988 = CARTESIAN_POINT ( 'NONE',  ( 69.20000000000001705, -0.6617647058823530326, -1.754335336830158631 ) ) ;
#27989 = CARTESIAN_POINT ( 'NONE',  ( 56.95000000000001705, -0.6999999999999999556, 1.820027472320129736 ) ) ;
#27990 = ORIENTED_EDGE ( 'NONE', *, *, #17811, .T. ) ;
#27991 = EDGE_CURVE ( 'NONE', #25173, #737, #1445, .T. ) ;
#27992 = CARTESIAN_POINT ( 'NONE',  ( 58.74999999305994436, 1.683452862813316742, 0.9423072185569032477 ) ) ;
#27993 = ORIENTED_EDGE ( 'NONE', *, *, #25304, .F. ) ;
#27994 = CARTESIAN_POINT ( 'NONE',  ( 46.90000000000001279, -4.227689052994015206, -1.125730994152046804 ) ) ;
#27995 = AXIS2_PLACEMENT_3D ( 'NONE', #6670, #23308, #1745 ) ;
#27997 = CARTESIAN_POINT ( 'NONE',  ( 15.03925126672133139, -4.945493884734786683, -1.606888370749751882 ) ) ;
#27996 = CARTESIAN_POINT ( 'NONE',  ( 48.37881665787880081, 1.311095223031216284, 3.884869838566831657 ) ) ;
#27998 = EDGE_LOOP ( 'NONE', ( #18832, #17969, #28543, #30110 ) ) ;
#27999 = ORIENTED_EDGE ( 'NONE', *, *, #10907, .F. ) ;
#28000 = CARTESIAN_POINT ( 'NONE',  ( 53.91582462592158720, 6.672259099522137582, -2.142504121165067499E-08 ) ) ;
#28001 = CARTESIAN_POINT ( 'NONE',  ( 30.89639353480223960, 7.705332860780324644, -1.425000000000107514 ) ) ;
#28003 = CARTESIAN_POINT ( 'NONE',  ( 50.25000000000003553, -1.499837071478530071, 1.323060376181713016 ) ) ;
#28002 = CARTESIAN_POINT ( 'NONE',  ( 51.77425608051891004, -4.052343190076493684, -1.949685991417844155 ) ) ;
#28004 = VERTEX_POINT ( 'NONE', #27692 ) ;
#28005 = CARTESIAN_POINT ( 'NONE',  ( -57.86042740578360366, -0.7887156198831604126, 3.845940847736174284 ) ) ;
#28006 = ADVANCED_FACE ( 'NONE', ( #6012 ), #15893, .T. ) ;
#28007 = CARTESIAN_POINT ( 'NONE',  ( 49.00000000000002132, 1.401298464324817071E-42, -5.132477568099407673E-13 ) ) ;
#28008 = CONTEXT_DEPENDENT_SHAPE_REPRESENTATION ( #7385, #1220 ) ;
#28009 = DIRECTION ( 'NONE',  ( -1.000000000000000000, 0.000000000000000000, 1.047444401652940007E-14 ) ) ;
#28010 =( BOUNDED_CURVE ( )  B_SPLINE_CURVE ( 2, ( #9536, #21880, #14257, #12201, #21730 ),
 .UNSPECIFIED., .F., .T. ) 
 B_SPLINE_CURVE_WITH_KNOTS ( ( 3, 2, 3 ),
 ( 0.7500000000000000000, 0.7592592592592593004, 0.7708295755062543053 ),
 .UNSPECIFIED. ) 
 CURVE ( )  GEOMETRIC_REPRESENTATION_ITEM ( )  RATIONAL_B_SPLINE_CURVE ( ( 0.9330127018922194093, 0.9330127018922194093, 1.000000000000000000, 0.9162930638470145883, 0.9371858258165919331 ) ) 
 REPRESENTATION_ITEM ( '' )  );
#28011 = ADVANCED_FACE ( 'NONE', ( #6304 ), #28631, .T. ) ;
#28012 = VERTEX_POINT ( 'NONE', #13727 ) ;
#28013 = CARTESIAN_POINT ( 'NONE',  ( 69.20000000000001705, 0.7500000000000000000, -1.988246715074081017 ) ) ;
#28014 = CARTESIAN_POINT ( 'NONE',  ( -36.30347965937281174, 2.964363692626830638, -4.273817190665726962 ) ) ;
#28015 = EDGE_CURVE ( 'NONE', #12844, #12135, #18669, .T. ) ;
#28016 = DIRECTION ( 'NONE',  ( -1.000000000000000000, 0.000000000000000000, -8.673617379883787770E-15 ) ) ;
#28017 = CIRCLE ( 'NONE', #2255, 0.04999999999999991257 ) ;
#28018 = DIRECTION ( 'NONE',  ( 0.000000000000000000, 0.000000000000000000, -1.000000000000000000 ) ) ;
#28019 = EDGE_CURVE ( 'NONE', #30275, #1323, #19601, .T. ) ;
#28021 = DIRECTION ( 'NONE',  ( 0.9994629430332293563, -0.03275911391080271046, -0.0008160631928541098616 ) ) ;
#28020 = DIRECTION ( 'NONE',  ( 3.002035892788117459E-16, -0.9996898646859344595, -0.02490330187381124133 ) ) ;
#28022 = AXIS2_PLACEMENT_3D ( 'NONE', #605, #2822, #15014 ) ;
#28023 = CARTESIAN_POINT ( 'NONE',  ( 49.05000000000002558, 1.401298464324817071E-42, -5.137714790107672405E-13 ) ) ;
#28025 = CARTESIAN_POINT ( 'NONE',  ( -62.09999999999997300, -2.700242798440558367, -0.3182811450455869662 ) ) ;
#28024 = LINE ( 'NONE', #30550, #3885 ) ;
#28026 = VERTEX_POINT ( 'NONE', #21048 ) ;
#28027 = CARTESIAN_POINT ( 'NONE',  ( -62.04999999999998295, -2.671081280896084653, -0.3941126626315437642 ) ) ;
#28028 = DIRECTION ( 'NONE',  ( 0.000000000000000000, 0.000000000000000000, 1.000000000000000000 ) ) ;
#28029 = CARTESIAN_POINT ( 'NONE',  ( 47.00000000000001421, -3.637377585518695611, -2.099877210783201331 ) ) ;
#28030 = CARTESIAN_POINT ( 'NONE',  ( 15.17214319754856966, -5.086913993735587169, 1.171642046065942910 ) ) ;
#28031 = COLOUR_RGB ( '', 0.40784314, 0.44705882, 0.49803922) ;
#28032 = EDGE_LOOP ( 'NONE', ( #822, #14119, #1660, #401 ) ) ;
#28033 = CARTESIAN_POINT ( 'NONE',  ( 52.72145679358934700, 4.007061708474140005, 2.049999999999815969 ) ) ;
#28034 = CARTESIAN_POINT ( 'NONE',  ( -59.29999999999997584, 2.330309927981284638E-15, 4.253626757584726372E-16 ) ) ;
#28035 = ORIENTED_EDGE ( 'NONE', *, *, #21348, .F. ) ;
#28036 = CIRCLE ( 'NONE', #740, 3.299999999999999822 ) ;
#28037 = CARTESIAN_POINT ( 'NONE',  ( -60.59999999999997300, -2.532112727260102947, 0.9372327013327054201 ) ) ;
#28038 = ORIENTED_EDGE ( 'NONE', *, *, #18457, .F. ) ;
#28039 = EDGE_CURVE ( 'NONE', #19112, #13995, #8972, .T. ) ;
#28040 = DIRECTION ( 'NONE',  ( -1.000000000000000000, -3.054025858079668409E-16, 2.042474015755241579E-16 ) ) ;
#28041 = CARTESIAN_POINT ( 'NONE',  ( 47.10000000000000853, -4.079448311123454296, -2.129011300494398018 ) ) ;
#28042 = ORIENTED_EDGE ( 'NONE', *, *, #16973, .F. ) ;
#28043 = SHAPE_REPRESENTATION_RELATIONSHIP ( 'NONE' , 'NONE' ,  #29923, #10428 ) ;
#28044 = EDGE_CURVE ( 'NONE', #29648, #31291, #20738, .T. ) ;
#28045 = CARTESIAN_POINT ( 'NONE',  ( 22.10406324885627782, 7.468725723506255854, 1.949999999999923128 ) ) ;
#28046 = CARTESIAN_POINT ( 'NONE',  ( -58.64405989232411542, 2.944486372867106461, -1.700000000000195577 ) ) ;
#28047 = ORIENTED_EDGE ( 'NONE', *, *, #21290, .T. ) ;
#28048 = DIRECTION ( 'NONE',  ( 3.491481338843133355E-15, 3.491481338843133355E-15, -1.000000000000000000 ) ) ;
#28049 = CIRCLE ( 'NONE', #6308, 4.299999999999998046 ) ;
#28050 = EDGE_CURVE ( 'NONE', #2387, #27521, #23135, .T. ) ;
#28051 = VERTEX_POINT ( 'NONE', #11542 ) ;
#28052 = VERTEX_POINT ( 'NONE', #9000 ) ;
#28053 = CARTESIAN_POINT ( 'NONE',  ( -57.74999999999997158, -2.944486372867089141, 1.699999999999783906 ) ) ;
#28054 = CARTESIAN_POINT ( 'NONE',  ( 46.90000000000001279, 1.734723475976807094E-15, 0.000000000000000000 ) ) ;
#28055 = DIRECTION ( 'NONE',  ( 0.000000000000000000, 0.000000000000000000, 1.000000000000000000 ) ) ;
#28056 = DIRECTION ( 'NONE',  ( 1.000000000000000000, 1.047444401652940007E-14, 0.000000000000000000 ) ) ;
#28057 = AXIS2_PLACEMENT_3D ( 'NONE', #1467, #27914, #16039 ) ;
#28058 = CARTESIAN_POINT ( 'NONE',  ( 57.04126813003668417, 0.7492316407094400388, 2.421767203557310122 ) ) ;
#28060 = CARTESIAN_POINT ( 'NONE',  ( -62.09999999999997300, 0.005353951483536216298, -0.2149229472152333620 ) ) ;
#28059 = CARTESIAN_POINT ( 'NONE',  ( -36.52757395963740095, 4.797343084509227751, -2.497389432263917186 ) ) ;
#28061 = AXIS2_PLACEMENT_3D ( 'NONE', #30145, #15750, #18291 ) ;
#28062 = FILL_AREA_STYLE_COLOUR ( '', #27122 ) ;
#28063 = DIRECTION ( 'NONE',  ( 0.000000000000000000, 0.9996898646859343485, 0.02490330187381123439 ) ) ;
#28064 = CARTESIAN_POINT ( 'NONE',  ( 58.75000000000002842, -1.039502773796971091, 1.800471618824829756 ) ) ;
#28065 = CARTESIAN_POINT ( 'NONE',  ( -59.68658240507107138, -2.223882124562203799, 1.531065007683262591 ) ) ;
#28066 = CARTESIAN_POINT ( 'NONE',  ( -61.34999999999997300, -2.581364933566181019, -0.7915523228156536861 ) ) ;
#28067 = AXIS2_PLACEMENT_3D ( 'NONE', #10916, #3787, #23283 ) ;
#28068 = DIRECTION ( 'NONE',  ( 0.000000000000000000, 0.000000000000000000, 1.000000000000000000 ) ) ;
#28069 = ORIENTED_EDGE ( 'NONE', *, *, #20283, .F. ) ;
#28070 = CARTESIAN_POINT ( 'NONE',  ( 69.25000000000000000, -0.7500000000000000000, -1.988246715074081905 ) ) ;
#28071 = CARTESIAN_POINT ( 'NONE',  ( -36.72207054450174724, -0.6818242347930901781, -5.365311767243446717 ) ) ;
#28072 = VERTEX_POINT ( 'NONE', #2027 ) ;
#28073 = DIRECTION ( 'NONE',  ( 0.000000000000000000, 0.000000000000000000, 1.000000000000000000 ) ) ;
#28074 = CARTESIAN_POINT ( 'NONE',  ( 51.80000000000001137, 6.475000000000062705, -2.050000000000180123 ) ) ;
#28076 = DIRECTION ( 'NONE',  ( 0.000000000000000000, 0.000000000000000000, 1.000000000000000000 ) ) ;
#28075 = CARTESIAN_POINT ( 'NONE',  ( -57.31249999999997158, 3.925981830489463142, -1.892888403967549806E-13 ) ) ;
#28077 = EDGE_LOOP ( 'NONE', ( #30642, #24046, #7049, #26951, #21272 ) ) ;
#28078 = ORIENTED_EDGE ( 'NONE', *, *, #21332, .T. ) ;
#28079 = VECTOR ( 'NONE', #806, 1000.000000000000000 ) ;
#28080 = CARTESIAN_POINT ( 'NONE',  ( 58.65000000000001990, 6.143261415694495821E-13, 3.111507638930570854E-58 ) ) ;
#28081 = EDGE_LOOP ( 'NONE', ( #9271, #12735, #13266, #27526 ) ) ;
#28082 = EDGE_CURVE ( 'NONE', #1571, #15671, #22128, .T. ) ;
#28083 = CIRCLE ( 'NONE', #1791, 4.600000000000000533 ) ;
#28084 = CARTESIAN_POINT ( 'NONE',  ( 51.31757909864145972, 1.004435980686513963, -1.391945786376508343 ) ) ;
#28085 = CARTESIAN_POINT ( 'NONE',  ( 51.80000000000001847, 2.428612866367529932E-14, -1.808587333520743709E-13 ) ) ;
#28086 = VERTEX_POINT ( 'NONE', #30513 ) ;
#28087 = CARTESIAN_POINT ( 'NONE',  ( 22.72181155399563224, 6.520914524688375735, -1.950000000000079670 ) ) ;
#28088 = CARTESIAN_POINT ( 'NONE',  ( -44.49999999999997868, 8.366749974758269874E-15, -1.589829192029513996E-13 ) ) ;
#28089 = MECHANICAL_DESIGN_GEOMETRIC_PRESENTATION_REPRESENTATION (  '', ( #21567 ), #296 ) ;
#28090 = CARTESIAN_POINT ( 'NONE',  ( -54.49150557875106671, -3.119347353020518465, -1.738776940373585767 ) ) ;
#28091 = ORIENTED_EDGE ( 'NONE', *, *, #15470, .T. ) ;
#28092 = ORIENTED_EDGE ( 'NONE', *, *, #14666, .F. ) ;
#28093 = AXIS2_PLACEMENT_3D ( 'NONE', #12559, #24300, #5275 ) ;
#28094 = DIRECTION ( 'NONE',  ( -2.581436205204234499E-16, 0.9796124928211140670, 0.2008964009354147762 ) ) ;
#28095 = AXIS2_PLACEMENT_3D ( 'NONE', #9470, #7088, #6611 ) ;
#28096 = CARTESIAN_POINT ( 'NONE',  ( 16.10667815269233216, -0.1434351685890333516, 5.407416993630366875 ) ) ;
#28097 = CARTESIAN_POINT ( 'NONE',  ( 56.95000000000001705, -0.7137254901960785602, -2.500119182087999548 ) ) ;
#28098 = CARTESIAN_POINT ( 'NONE',  ( -59.69999999999997442, -2.473915798711235237, -1.238538609462283446 ) ) ;
#28099 = CARTESIAN_POINT ( 'NONE',  ( -57.22499999999997300, -1.024571644770612577, 4.996023713387681475 ) ) ;
#28100 = EDGE_CURVE ( 'NONE', #27455, #14166, #21116, .T. ) ;
#28101 = DIRECTION ( 'NONE',  ( -0.000000000000000000, 1.000000000000000000, 0.000000000000000000 ) ) ;
#28102 = CARTESIAN_POINT ( 'NONE',  ( 57.02118883257515591, 0.7413508443325595998, -1.786034507790101866 ) ) ;
#28104 = SPHERICAL_SURFACE ( 'NONE', #11887, 0.1000000000000000056 ) ;
#28103 = CARTESIAN_POINT ( 'NONE',  ( 47.00000000000002132, -3.726179070414207928, 1.041421356237309803 ) ) ;
#28105 = AXIS2_PLACEMENT_3D ( 'NONE', #4083, #28467, #13723 ) ;
#28106 = CARTESIAN_POINT ( 'NONE',  ( -53.99999999999997868, 0.000000000000000000, 0.000000000000000000 ) ) ;
#28107 = AXIS2_PLACEMENT_3D ( 'NONE', #14890, #19821, #10154 ) ;
#28108 = DIRECTION ( 'NONE',  ( 3.489354422748178582E-15, -1.218509414717996338E-16, 1.000000000000000000 ) ) ;
#28109 = CARTESIAN_POINT ( 'NONE',  ( -74.38999999999998636, -1.249612330857420739, -0.03112912734225924821 ) ) ;
#28110 = CARTESIAN_POINT ( 'NONE',  ( -56.72499999999997300, 3.116721586436802063E-15, -1.005743832985040150E-16 ) ) ;
#28111 = EDGE_LOOP ( 'NONE', ( #14303, #11139 ) ) ;
#28112 = CIRCLE ( 'NONE', #20041, 2.000000000000000000 ) ;
#28113 = VERTEX_POINT ( 'NONE', #8819 ) ;
#28114 = VECTOR ( 'NONE', #18087, 1000.000000000000000 ) ;
#28115 = CARTESIAN_POINT ( 'NONE',  ( 61.25000000000002132, 6.415596960124259844E-13, 3.111507638930570854E-58 ) ) ;
#28116 = EDGE_LOOP ( 'NONE', ( #21469, #26845, #31272, #2635 ) ) ;
#28117 = VECTOR ( 'NONE', #26184, 1000.000000000000000 ) ;
#28118 = CARTESIAN_POINT ( 'NONE',  ( 51.38880644991420610, 3.878826100321112413, 2.049999999999820410 ) ) ;
#28119 = CARTESIAN_POINT ( 'NONE',  ( -57.40835481156724285, -3.238593381231841928, -2.874284765127022023 ) ) ;
#28121 = CARTESIAN_POINT ( 'NONE',  ( 51.41512632536708338, -3.877460150898793145, -1.337636034594305245 ) ) ;
#28120 = CARTESIAN_POINT ( 'NONE',  ( 22.04321716858593661, 7.679566743993218481, -2.050000000000076650 ) ) ;
#28122 = ORIENTED_EDGE ( 'NONE', *, *, #25214, .T. ) ;
#28123 = ORIENTED_EDGE ( 'NONE', *, *, #21039, .T. ) ;
#28124 = LINE ( 'NONE', #25287, #5811 ) ;
#28125 = ADVANCED_FACE ( 'NONE', ( #21217 ), #1873, .T. ) ;
#28126 = DIRECTION ( 'NONE',  ( -2.117927888850090838E-16, 0.02490330187381123786, -0.9996898646859343485 ) ) ;
#28127 = VECTOR ( 'NONE', #6159, 1000.000000000000000 ) ;
#28128 = ORIENTED_EDGE ( 'NONE', *, *, #5393, .F. ) ;
#28130 = CARTESIAN_POINT ( 'NONE',  ( 15.03925126672132961, 0.4576450603547064788, -5.200000000000000178 ) ) ;
#28129 = CYLINDRICAL_SURFACE ( 'NONE', #19145, 0.1500000000000001887 ) ;
#28131 = EDGE_CURVE ( 'NONE', #27840, #16066, #10985, .T. ) ;
#28132 = CARTESIAN_POINT ( 'NONE',  ( 61.09423418604154676, -0.6373668173473425735, 1.895722432253304168 ) ) ;
#28133 = ORIENTED_EDGE ( 'NONE', *, *, #22207, .T. ) ;
#28134 = DIRECTION ( 'NONE',  ( 0.000000000000000000, 0.000000000000000000, 1.000000000000000000 ) ) ;
#28135 = AXIS2_PLACEMENT_3D ( 'NONE', #16841, #30809, #51 ) ;
#28136 = CARTESIAN_POINT ( 'NONE',  ( 51.17950113889409636, -0.9670426259150803894, -1.523577707254206715 ) ) ;
#28137 = TOROIDAL_SURFACE ( 'NONE', #4881, -24.59258869922086888, 30.00000000000000000 ) ;
#28138 = DIRECTION ( 'NONE',  ( 3.489354422748178582E-15, -1.218509414717996338E-16, 1.000000000000000000 ) ) ;
#28139 = CARTESIAN_POINT ( 'NONE',  ( -58.82202994616202574, 2.078460969082674747, -3.600000000000199929 ) ) ;
#28140 = AXIS2_PLACEMENT_3D ( 'NONE', #17521, #1050, #10381 ) ;
#28141 = EDGE_CURVE ( 'NONE', #21323, #26979, #26687, .T. ) ;
#28142 = TOROIDAL_SURFACE ( 'NONE', #16002, 4.600000000000000533, 0.5000000000000013323 ) ;
#28143 = CARTESIAN_POINT ( 'NONE',  ( -59.19999999999997442, -3.382957286162487698, 0.3399999999999019917 ) ) ;
#28144 = CARTESIAN_POINT ( 'NONE',  ( -57.98542740578360366, 2.936324665650198007, 2.606018187048509294 ) ) ;
#28145 = CARTESIAN_POINT ( 'NONE',  ( 65.05000000000001137, -1.025519176787267142E-28, -6.813625832752373386E-13 ) ) ;
#28146 = AXIS2_PLACEMENT_3D ( 'NONE', #24045, #28807, #2356 ) ;
#28147 = EDGE_CURVE ( 'NONE', #23567, #21339, #11210, .T. ) ;
#28148 = DIRECTION ( 'NONE',  ( 1.000000000000000000, 0.000000000000000000, 0.000000000000000000 ) ) ;
#28149 = AXIS2_PLACEMENT_3D ( 'NONE', #14335, #1998, #13846 ) ;
#28150 = CARTESIAN_POINT ( 'NONE',  ( 53.12794425116820207, 4.814976926303064175, 1.597382792423633902 ) ) ;
#28151 = DIRECTION ( 'NONE',  ( 4.670714851210922627E-16, -0.9333474217026305197, -0.3589743589743593088 ) ) ;
#28152 = VERTEX_POINT ( 'NONE', #16130 ) ;
#28153 = CARTESIAN_POINT ( 'NONE',  ( 58.65000045311410304, 1.580645149931350080, 1.008695754911069331 ) ) ;
#28154 = VECTOR ( 'NONE', #21558, 1000.000000000000000 ) ;
#28155 = ORIENTED_EDGE ( 'NONE', *, *, #27808, .F. ) ;
#28156 = CARTESIAN_POINT ( 'NONE',  ( 58.65000000000002700, -0.5811678240976775323, -1.782657835994575724 ) ) ;
#28158 = DIRECTION ( 'NONE',  ( 0.000000000000000000, 0.000000000000000000, 1.000000000000000000 ) ) ;
#28157 = CARTESIAN_POINT ( 'NONE',  ( 48.30000000000002558, 0.6462379109120998111, 4.048750000000022276 ) ) ;
#28159 = ORIENTED_EDGE ( 'NONE', *, *, #4744, .F. ) ;
#28160 = ORIENTED_EDGE ( 'NONE', *, *, #11356, .T. ) ;
#28161 = LINE ( 'NONE', #18839, #8291 ) ;
#28162 = EDGE_CURVE ( 'NONE', #14417, #6108, #12485, .T. ) ;
#28163 = DIRECTION ( 'NONE',  ( 0.7071067811865539010, -0.1420552074174017965, 0.6926906366088616540 ) ) ;
#28164 = AXIS2_PLACEMENT_3D ( 'NONE', #21554, #29533, #8025 ) ;
#28166 = CARTESIAN_POINT ( 'NONE',  ( 54.50000000000002132, -0.2842225609755594795, -1.577752156565102655E-15 ) ) ;
#28165 = DIRECTION ( 'NONE',  ( 0.000000000000000000, -1.000000000000000000, -3.491481338843132961E-15 ) ) ;
#28167 = AXIS2_PLACEMENT_3D ( 'NONE', #3683, #16037, #16198 ) ;
#28168 = ADVANCED_FACE ( 'NONE', ( #21843 ), #28938, .F. ) ;
#28169 = ORIENTED_EDGE ( 'NONE', *, *, #16041, .T. ) ;
#28170 = CARTESIAN_POINT ( 'NONE',  ( -55.92292740578360366, 2.256877952708269408, -2.542931754211925632 ) ) ;
#28171 = EDGE_CURVE ( 'NONE', #12544, #29950, #10495, .T. ) ;
#28172 = CARTESIAN_POINT ( 'NONE',  ( 58.75000000000000711, 0.8897917884447026360, -1.791164585742097914 ) ) ;
#28173 = SHAPE_DEFINITION_REPRESENTATION ( #28327, #3777 ) ;
#28174 = B_SPLINE_CURVE_WITH_KNOTS ( 'NONE', 3,
 ( #2741, #17311, #5263, #22233 ),
 .UNSPECIFIED., .F., .F.,
 ( 4, 4 ),
 ( 0.0001159639600966503627, 0.0002000540139215557138 ),
 .UNSPECIFIED. ) ;
#28175 = CARTESIAN_POINT ( 'NONE',  ( 53.61897490378053277, 5.359699723822127559, -1.649481177327357662 ) ) ;
#28176 = CARTESIAN_POINT ( 'NONE',  ( -35.85663232820584057, 1.793057972832144520, 4.026191436122060097 ) ) ;
#28177 = CARTESIAN_POINT ( 'NONE',  ( -62.09999999999998010, -2.637337459618612101, 0.1843787714682001699 ) ) ;
#28178 = CIRCLE ( 'NONE', #1899, 0.05000000000000009298 ) ;
#28179 = ORIENTED_EDGE ( 'NONE', *, *, #27819, .T. ) ;
#28180 = AXIS2_PLACEMENT_3D ( 'NONE', #10210, #12733, #29224 ) ;
#28181 = EDGE_CURVE ( 'NONE', #21603, #17195, #14537, .T. ) ;
#28182 = CARTESIAN_POINT ( 'NONE',  ( 57.03052440771394060, -0.7462437932013319397, 1.781707539322121336 ) ) ;
#28183 = VECTOR ( 'NONE', #13296, 1000.000000000000000 ) ;
#28184 = VERTEX_POINT ( 'NONE', #9938 ) ;
#28185 = CARTESIAN_POINT ( 'NONE',  ( -36.56242893520638404, 3.003531019938693536, -4.498666779076329725 ) ) ;
#28186 = DIRECTION ( 'NONE',  ( -0.000000000000000000, 0.000000000000000000, 1.000000000000000000 ) ) ;
#28187 = DIRECTION ( 'NONE',  ( 9.754918421198724481E-16, -0.9601771338024399638, 0.2793919678926571892 ) ) ;
#28188 = CARTESIAN_POINT ( 'NONE',  ( 15.32752150720753725, -1.093737229520474363, -5.295968199484771155 ) ) ;
#28189 = AXIS2_PLACEMENT_3D ( 'NONE', #28294, #2156, #6751 ) ;
#28190 = CIRCLE ( 'NONE', #7477, 4.199999999999954881 ) ;
#28192 = CARTESIAN_POINT ( 'NONE',  ( -77.29999999999998295, -0.4498604391086740151, -0.01120648584320970212 ) ) ;
#28191 = CARTESIAN_POINT ( 'NONE',  ( -44.49999999999997868, 0.000000000000000000, 0.000000000000000000 ) ) ;
#28193 = AXIS2_PLACEMENT_3D ( 'NONE', #14379, #14227, #26574 ) ;
#28194 = ADVANCED_FACE ( 'NONE', ( #10093 ), #2507, .F. ) ;
#28195 = CARTESIAN_POINT ( 'NONE',  ( 46.99711047134479713, -4.086537470741383515, -2.116255473935157561 ) ) ;
#28197 = CARTESIAN_POINT ( 'NONE',  ( 50.30848954602731737, -1.391941090707485396, -3.850000000000024070 ) ) ;
#28196 = DIRECTION ( 'NONE',  ( -2.095850865446309212E-30, -1.000000000000000000, -2.891205793294679411E-15 ) ) ;
#28198 = ORIENTED_EDGE ( 'NONE', *, *, #26442, .T. ) ;
#28199 = DIRECTION ( 'NONE',  ( -1.000000000000000000, 1.219044193948983948E-29, -3.491481338843133355E-15 ) ) ;
#28200 = B_SPLINE_CURVE_WITH_KNOTS ( 'NONE', 3,
 ( #18063, #1247, #8539, #3946, #18224, #16301, #21229, #28002, #1887, #13418 ),
 .UNSPECIFIED., .F., .F.,
 ( 4, 2, 2, 2, 4 ),
 ( 0.000000000000000000, 0.0003923015305839677226, 0.0007846030611679354451, 0.001176904591751903222, 0.001569206122335870890 ),
 .UNSPECIFIED. ) ;
#28201 = CARTESIAN_POINT ( 'NONE',  ( 58.75000000000000711, 1.106298139390812452, -1.666164585742097914 ) ) ;
#28202 = CIRCLE ( 'NONE', #17034, 0.2500000000000000000 ) ;
#28204 = DIRECTION ( 'NONE',  ( -1.000000000000000000, -3.054025858079668409E-16, 2.042474015755241579E-16 ) ) ;
#28203 = CARTESIAN_POINT ( 'NONE',  ( 58.73379417893117704, 1.830385781110580590, 0.4072049916502743505 ) ) ;
#28205 = CARTESIAN_POINT ( 'NONE',  ( 15.95705409078442649, -4.926689578693679294, 2.233438676318023397 ) ) ;
#28206 = VERTEX_POINT ( 'NONE', #31313 ) ;
#28207 = CARTESIAN_POINT ( 'NONE',  ( 53.31680359303815919, 8.198234760421843959, 2.049999999999814193 ) ) ;
#28208 = CARTESIAN_POINT ( 'NONE',  ( 50.39884346364544854, -0.8930148142854128501, 3.925689827643444652 ) ) ;
#28209 = AXIS2_PLACEMENT_3D ( 'NONE', #22925, #23392, #1379 ) ;
#28210 = ADVANCED_FACE ( 'NONE', ( #5027 ), #9377, .T. ) ;
#28211 =( BOUNDED_CURVE ( )  B_SPLINE_CURVE ( 3, ( #19868, #24909, #8138, #15585 ),
 .UNSPECIFIED., .F., .T. ) 
 B_SPLINE_CURVE_WITH_KNOTS ( ( 4, 4 ),
 ( 5.004453192798488104, 5.119588733684844684 ),
 .UNSPECIFIED. ) 
 CURVE ( )  GEOMETRIC_REPRESENTATION_ITEM ( )  RATIONAL_B_SPLINE_CURVE ( ( 1.000000000000000000, 0.9988956223160183612, 0.9988956223160183612, 1.000000000000000000 ) ) 
 REPRESENTATION_ITEM ( '' )  );
#28212 = AXIS2_PLACEMENT_3D ( 'NONE', #17688, #2788, #29705 ) ;
#28213 = ORIENTED_EDGE ( 'NONE', *, *, #12959, .F. ) ;
#28214 = EDGE_CURVE ( 'NONE', #21983, #28408, #25646, .T. ) ;
#28215 = DIRECTION ( 'NONE',  ( 1.000000000000000000, 0.000000000000000000, -1.047444401652940007E-14 ) ) ;
#28216 = ORIENTED_EDGE ( 'NONE', *, *, #19183, .T. ) ;
#28217 = EDGE_CURVE ( 'NONE', #9091, #7150, #19350, .T. ) ;
#28218 = DIRECTION ( 'NONE',  ( -1.387778780781445676E-14, 1.000000000000000000, 0.000000000000000000 ) ) ;
#28219 = VERTEX_POINT ( 'NONE', #28724 ) ;
#28220 = CARTESIAN_POINT ( 'NONE',  ( -55.00952994616204705, 3.117691453623994580, -1.800000000000181899 ) ) ;
#28221 = CARTESIAN_POINT ( 'NONE',  ( -58.26905989232412253, -2.944486372867088697, 1.699999999999781686 ) ) ;
#28222 = ORIENTED_EDGE ( 'NONE', *, *, #12565, .F. ) ;
#28223 = EDGE_LOOP ( 'NONE', ( #12973, #20355, #16940, #19581 ) ) ;
#28224 = ORIENTED_EDGE ( 'NONE', *, *, #29700, .F. ) ;
#28225 = CARTESIAN_POINT ( 'NONE',  ( -55.63452994616205416, 3.117691453623979481, 1.799999999999814415 ) ) ;
#28226 = CARTESIAN_POINT ( 'NONE',  ( -35.85663232820584057, -4.018128179617557194, 3.618665901676652918 ) ) ;
#28227 = CARTESIAN_POINT ( 'NONE',  ( 29.64923672893718276, 6.300449151053643781, -1.425000000000103739 ) ) ;
#28228 = DIRECTION ( 'NONE',  ( 1.000000000000000000, 3.053848253006669023E-16, -2.042510438544995415E-16 ) ) ;
#28229 = CARTESIAN_POINT ( 'NONE',  ( -59.27299602954527558, -2.279082375080590417, 1.356559916049900005 ) ) ;
#28230 = AXIS2_PLACEMENT_3D ( 'NONE', #9734, #29345, #10333 ) ;
#28232 = DIRECTION ( 'NONE',  ( 0.7313537016191670181, 0.6819983600625022513, -2.468850131082252327E-15 ) ) ;
#28231 = DIRECTION ( 'NONE',  ( 0.000000000000000000, 0.2008964009354147762, -0.9796124928211140670 ) ) ;
#28233 = EDGE_CURVE ( 'NONE', #27954, #21815, #9492, .T. ) ;
#28234 = SURFACE_STYLE_USAGE ( .BOTH. , #30763 ) ;
#28235 = DIRECTION ( 'NONE',  ( -1.520093157366848107E-16, 0.5877852522924625900, 0.8090169943749551118 ) ) ;
#28236 = EDGE_CURVE ( 'NONE', #23320, #27840, #12011, .T. ) ;
#28237 = FACE_OUTER_BOUND ( 'NONE', #5734, .T. ) ;
#28238 = CARTESIAN_POINT ( 'NONE',  ( 58.65266784251146959, -1.589569034372440459, -0.9945725797246820488 ) ) ;
#28239 = DIRECTION ( 'NONE',  ( 0.000000000000000000, 0.2008964009354147484, -0.9796124928211138450 ) ) ;
#28240 = EDGE_CURVE ( 'NONE', #26143, #5179, #9765, .T. ) ;
#28241 = CARTESIAN_POINT ( 'NONE',  ( 50.36024759664407213, 1.282505688586122572, -3.869483523004607406 ) ) ;
#28242 = ORIENTED_EDGE ( 'NONE', *, *, #9550, .F. ) ;
#28244 = CARTESIAN_POINT ( 'NONE',  ( 50.50000000000001421, -0.6462379109120508502, 4.048750000000023164 ) ) ;
#28243 = DIRECTION ( 'NONE',  ( 0.000000000000000000, -1.000000000000000000, 0.000000000000000000 ) ) ;
#28245 = DIRECTION ( 'NONE',  ( -1.000000000000000000, 0.000000000000000000, 1.047444401652940007E-14 ) ) ;
#28246 = ORIENTED_EDGE ( 'NONE', *, *, #20116, .T. ) ;
#28247 = DIRECTION ( 'NONE',  ( 1.000000000000000000, 0.000000000000000000, -1.047444401652940007E-14 ) ) ;
#28248 = CARTESIAN_POINT ( 'NONE',  ( -61.24999999999995026, 2.023778652682512839E-14, -3.400000000000217515 ) ) ;
#28249 = ORIENTED_EDGE ( 'NONE', *, *, #24728, .F. ) ;
#28250 = EDGE_LOOP ( 'NONE', ( #9896, #27259, #4135, #30423, #18634, #19529 ) ) ;
#28251 = CARTESIAN_POINT ( 'NONE',  ( 50.59602332238209499, 0.1408342061609077767, 0.7375000000000033751 ) ) ;
#28252 = STYLED_ITEM ( 'NONE', ( #24255 ), #2132 ) ;
#28253 = ORIENTED_EDGE ( 'NONE', *, *, #6511, .T. ) ;
#28254 = CARTESIAN_POINT ( 'NONE',  ( 58.75000000000003553, -1.760622601995820657, 0.8948927608039445314 ) ) ;
#28255 = VECTOR ( 'NONE', #23964, 1000.000000000000000 ) ;
#28256 = FACE_OUTER_BOUND ( 'NONE', #16311, .T. ) ;
#28257 = ORIENTED_EDGE ( 'NONE', *, *, #5592, .F. ) ;
#28258 = DIRECTION ( 'NONE',  ( 2.117927888850091331E-16, -0.02490330187381135929, 0.9996898646859343485 ) ) ;
#28259 = DIRECTION ( 'NONE',  ( 1.047444401652940007E-14, 0.000000000000000000, 1.000000000000000000 ) ) ;
#28260 = CARTESIAN_POINT ( 'NONE',  ( -54.49999999999997868, -3.396648781713578202, -1.005585003271797007 ) ) ;
#28261 = ORIENTED_EDGE ( 'NONE', *, *, #4272, .F. ) ;
#28262 = ORIENTED_EDGE ( 'NONE', *, *, #6548, .F. ) ;
#28263 = CARTESIAN_POINT ( 'NONE',  ( 46.99978405390194780, -4.243814194680251006, -1.064485530476996455 ) ) ;
#28264 = CARTESIAN_POINT ( 'NONE',  ( -62.09999999999997300, -2.704716430269783700, 0.1751800441595645352 ) ) ;
#28265 = CARTESIAN_POINT ( 'NONE',  ( -61.01905989232410121, 2.023778652682512207E-14, -3.400000000000216183 ) ) ;
#28266 = CARTESIAN_POINT ( 'NONE',  ( 61.25000000000002842, -0.4999999999993586797, -1.807104036850122109 ) ) ;
#28267 = CARTESIAN_POINT ( 'NONE',  ( 58.66118217212500952, 1.337770226786352046, 1.313877211063982253 ) ) ;
#28268 = CARTESIAN_POINT ( 'NONE',  ( 61.25000000000000711, 1.323060376180939413, 1.499837071478648420 ) ) ;
#28269 = CARTESIAN_POINT ( 'NONE',  ( 58.75000000000002132, -0.5811678240974700316, 1.782657835994650775 ) ) ;
#28270 = CARTESIAN_POINT ( 'NONE',  ( 58.66107449606948876, -1.802323084877160086, -0.5180360531255027157 ) ) ;
#28271 = EDGE_CURVE ( 'NONE', #8618, #67, #19100, .T. ) ;
#28272 = COLOUR_RGB ( '', 0.08235294, 0.09019608, 0.10196078) ;
#28273 = DIRECTION ( 'NONE',  ( 0.000000000000000000, -0.2008964009354147484, 0.9796124928211138450 ) ) ;
#28274 = EDGE_CURVE ( 'NONE', #22777, #30315, #30720, .T. ) ;
#28275 = CARTESIAN_POINT ( 'NONE',  ( -55.87499999999997158, 1.184343223768590025, 3.558065644182724974 ) ) ;
#28276 = AXIS2_PLACEMENT_3D ( 'NONE', #17619, #7497, #12538 ) ;
#28277 = DIRECTION ( 'NONE',  ( 9.329605248950888974E-15, -1.000000000000000000, 0.000000000000000000 ) ) ;
#28278 = CARTESIAN_POINT ( 'NONE',  ( 51.32030452908213647, -1.012971576473159718, 1.577980961882171185 ) ) ;
#28279 = EDGE_CURVE ( 'NONE', #10060, #15811, #12831, .T. ) ;
#28280 = EDGE_LOOP ( 'NONE', ( #1000, #7311, #21951, #18802 ) ) ;
#28281 = ORIENTED_EDGE ( 'NONE', *, *, #22298, .T. ) ;
#28282 = DIRECTION ( 'NONE',  ( 1.000000000000000000, 1.047444401652940007E-14, 0.000000000000000000 ) ) ;
#28283 = ORIENTED_EDGE ( 'NONE', *, *, #26349, .T. ) ;
#28284 = CARTESIAN_POINT ( 'NONE',  ( 53.16217804548193016, 8.131925109091586279, 1.902110155464532104 ) ) ;
#28285 = CARTESIAN_POINT ( 'NONE',  ( -55.90835481156724285, -3.238593381231841928, -2.874284765127022467 ) ) ;
#28286 = AXIS2_PLACEMENT_3D ( 'NONE', #8485, #20533, #23053 ) ;
#28288 = DIRECTION ( 'NONE',  ( 0.000000000000000000, -0.9996898646859343485, -0.02490330187381143562 ) ) ;
#28287 = SPHERICAL_SURFACE ( 'NONE', #1375, 0.1000000000000000056 ) ;
#28289 = ORIENTED_EDGE ( 'NONE', *, *, #713, .F. ) ;
#28290 = ORIENTED_EDGE ( 'NONE', *, *, #27605, .F. ) ;
#28291 = CARTESIAN_POINT ( 'NONE',  ( 47.00000000000002132, 2.428612866367529932E-14, 0.000000000000000000 ) ) ;
#28292 = ORIENTED_EDGE ( 'NONE', *, *, #12745, .T. ) ;
#28293 = ADVANCED_FACE ( 'NONE', ( #22065 ), #23594, .T. ) ;
#28294 = CARTESIAN_POINT ( 'NONE',  ( 58.75000000000000711, 1.470078920827434965, 1.470078920828533420 ) ) ;
#28295 = AXIS2_PLACEMENT_3D ( 'NONE', #784, #20132, #5696 ) ;
#28296 = ORIENTED_EDGE ( 'NONE', *, *, #14247, .T. ) ;
#28298 = CARTESIAN_POINT ( 'NONE',  ( -35.85663232820584057, -4.945493884734804446, -1.606888370749739448 ) ) ;
#28297 = DIRECTION ( 'NONE',  ( 1.000000000000000000, -0.000000000000000000, -0.000000000000000000 ) ) ;
#28299 = DIRECTION ( 'NONE',  ( 0.000000000000000000, 0.000000000000000000, 1.000000000000000000 ) ) ;
#28300 = ORIENTED_EDGE ( 'NONE', *, *, #4075, .T. ) ;
#28301 = CARTESIAN_POINT ( 'NONE',  ( -36.26369610968575330, 5.012449653004628303, -1.400819699605756696 ) ) ;
#28302 = B_SPLINE_CURVE_WITH_KNOTS ( 'NONE', 3,
 ( #30960, #9275, #17288, #346, #6894, #16563 ),
 .UNSPECIFIED., .F., .F.,
 ( 4, 2, 4 ),
 ( 0.000000000000000000, 0.0001000270069599285065, 0.0002000540139198570130 ),
 .UNSPECIFIED. ) ;
#28303 = FACE_OUTER_BOUND ( 'NONE', #26522, .T. ) ;
#28304 = VECTOR ( 'NONE', #19160, 1000.000000000000000 ) ;
#28305 = DIRECTION ( 'NONE',  ( 0.000000000000000000, 0.9663289263986323263, -0.2573099415204678220 ) ) ;
#28306 = CARTESIAN_POINT ( 'NONE',  ( 57.00000000000001421, -0.6999999999999999556, 2.452039967047845437 ) ) ;
#28307 = CARTESIAN_POINT ( 'NONE',  ( -56.82202994616205416, -4.156921938165296204, -2.167734102480683039E-13 ) ) ;
#28308 = CARTESIAN_POINT ( 'NONE',  ( -59.31366000257239790, 3.244990441519633784, -1.015485107948731702 ) ) ;
#28309 = CIRCLE ( 'NONE', #17689, 1.250000000000000222 ) ;
#28310 = DIRECTION ( 'NONE',  ( 3.489354422748178582E-15, -1.218509414717996338E-16, 1.000000000000000000 ) ) ;
#28311 = CARTESIAN_POINT ( 'NONE',  ( 50.42115343657336268, 0.9200365198983971871, -3.998286360709619736 ) ) ;
#28312 = CARTESIAN_POINT ( 'NONE',  ( -55.54792740578360366, -2.256877952708265411, 2.542931754211921191 ) ) ;
#28313 = ADVANCED_FACE ( 'NONE', ( #4959, #26654 ), #512, .T. ) ;
#28314 = DIRECTION ( 'NONE',  ( -1.000000000000000000, 1.219044193948983948E-29, -3.491481338843133355E-15 ) ) ;
#28315 = VERTEX_POINT ( 'NONE', #12237 ) ;
#28316 = FACE_OUTER_BOUND ( 'NONE', #5443, .T. ) ;
#28317 = CARTESIAN_POINT ( 'NONE',  ( -59.50952994616202574, 3.117691453624007014, -1.800000000000176570 ) ) ;
#28318 = CARTESIAN_POINT ( 'NONE',  ( -36.76447480099743359, 0.6031025731809287471, 5.374022845360671319 ) ) ;
#28319 = DIRECTION ( 'NONE',  ( 0.000000000000000000, 0.9996898646859343485, 0.02490330187381123786 ) ) ;
#28320 = VERTEX_POINT ( 'NONE', #21921 ) ;
#28321 = AXIS2_PLACEMENT_3D ( 'NONE', #8790, #30819, #28288 ) ;
#28322 = CARTESIAN_POINT ( 'NONE',  ( 58.66118217212510189, 1.632243256843118884, 0.9228675180760285146 ) ) ;
#28323 = ORIENTED_EDGE ( 'NONE', *, *, #15229, .F. ) ;
#28324 = DIRECTION ( 'NONE',  ( -1.000000000000000000, -0.000000000000000000, 3.491481338843133355E-15 ) ) ;
#28326 = CARTESIAN_POINT ( 'NONE',  ( 58.65266784251147669, -1.372094080475589228, 1.277991457600579528 ) ) ;
#28325 = CARTESIAN_POINT ( 'NONE',  ( 48.50000000000002132, 1.391941090707540685, 3.850000000000022293 ) ) ;
#28327 = PRODUCT_DEFINITION_SHAPE ( 'NONE', 'NONE',  #6239 ) ;
#28328 = ORIENTED_EDGE ( 'NONE', *, *, #12507, .T. ) ;
#28329 = CARTESIAN_POINT ( 'NONE',  ( 58.75000000000000711, 1.666164585742715420, 1.106298139391201030 ) ) ;
#28330 = AXIS2_PLACEMENT_3D ( 'NONE', #15438, #25091, #13063 ) ;
#28331 = FACE_OUTER_BOUND ( 'NONE', #21105, .T. ) ;
#28333 = LINE ( 'NONE', #1708, #24121 ) ;
#28332 = FACE_OUTER_BOUND ( 'NONE', #8679, .T. ) ;
#28334 = ORIENTED_EDGE ( 'NONE', *, *, #29897, .F. ) ;
#28335 = CARTESIAN_POINT ( 'NONE',  ( -54.68749999999998579, 0.8699069336946692044, -4.241846523238429256 ) ) ;
#28336 = DIRECTION ( 'NONE',  ( -0.9993908270190958731, 0.03489949670250085123, 3.435095992031088928E-15 ) ) ;
#28337 = PRODUCT_CONTEXT ( 'NONE', #24304, 'mechanical' ) ;
#28338 = CARTESIAN_POINT ( 'NONE',  ( -61.35349513024766566, -2.601746391104207135, -0.5952655458314711767 ) ) ;
#28339 = CARTESIAN_POINT ( 'NONE',  ( -56.93749999999996447, -3.399999999999991473, -2.119568960425587465E-13 ) ) ;
#28340 = DIRECTION ( 'NONE',  ( 2.459562394685743786E-16, -0.9510565162951521989, -0.3090169943749515591 ) ) ;
#28342 = VERTEX_POINT ( 'NONE', #3519 ) ;
#28341 = ADVANCED_FACE ( 'NONE', ( #15076 ), #30239, .T. ) ;
#28343 = DIRECTION ( 'NONE',  ( -1.000000000000000000, -0.000000000000000000, -0.000000000000000000 ) ) ;
#28344 = DIRECTION ( 'NONE',  ( -2.117927888850090838E-16, 0.02490330187381123786, -0.9996898646859343485 ) ) ;
#28345 = CARTESIAN_POINT ( 'NONE',  ( 58.65000000000003411, -1.571497941946114363, -1.022750809560766694 ) ) ;
#28346 = DIRECTION ( 'NONE',  ( 0.000000000000000000, -1.000000000000000000, 0.000000000000000000 ) ) ;
#28347 = CIRCLE ( 'NONE', #1048, 0.1499999999999999667 ) ;
#28348 = CARTESIAN_POINT ( 'NONE',  ( 57.01182421275571954, -0.7322894606377696736, -2.432677346698721266 ) ) ;
#28349 = EDGE_CURVE ( 'NONE', #23465, #29446, #20164, .T. ) ;
#28351 = DIRECTION ( 'NONE',  ( 0.000000000000000000, -1.000000000000000000, 0.000000000000000000 ) ) ;
#28350 = CARTESIAN_POINT ( 'NONE',  ( 58.75000000000000711, 1.895722432253174938, -0.6373668173460090847 ) ) ;
#28352 = CARTESIAN_POINT ( 'NONE',  ( -62.09999999999998010, -2.624885808681706845, -0.3154661608747524326 ) ) ;
#28354 = LINE ( 'NONE', #18711, #15498 ) ;
#28353 = DIRECTION ( 'NONE',  ( 1.000000000000000000, -0.000000000000000000, -1.047444401652940007E-14 ) ) ;
#28355 = ORIENTED_EDGE ( 'NONE', *, *, #14663, .T. ) ;
#28356 = CARTESIAN_POINT ( 'NONE',  ( 61.19881854997409221, -0.7436933986905437388, -1.660788881864677435 ) ) ;
#28357 =( BOUNDED_CURVE ( )  B_SPLINE_CURVE ( 3, ( #31065, #2097, #9239, #14130 ),
 .UNSPECIFIED., .F., .T. ) 
 B_SPLINE_CURVE_WITH_KNOTS ( ( 4, 4 ),
 ( 1.163596573494744213, 1.278732114381100571 ),
 .UNSPECIFIED. ) 
 CURVE ( )  GEOMETRIC_REPRESENTATION_ITEM ( )  RATIONAL_B_SPLINE_CURVE ( ( 1.000000000000000000, 0.9988956223160183612, 0.9988956223160183612, 1.000000000000000000 ) ) 
 REPRESENTATION_ITEM ( '' )  );
#28358 = CARTESIAN_POINT ( 'NONE',  ( -44.49999999999997868, 1.499999999999999556, 4.029888335921975262 ) ) ;
#28360 = CARTESIAN_POINT ( 'NONE',  ( -36.30347965937241383, 4.980680447166604630, 1.498595263773591757 ) ) ;
#28359 = DIRECTION ( 'NONE',  ( 0.7071067811865466846, -0.7068874824028871240, -0.01760929362890767402 ) ) ;
#28361 = FACE_OUTER_BOUND ( 'NONE', #23070, .T. ) ;
#28362 = ORIENTED_EDGE ( 'NONE', *, *, #11318, .T. ) ;
#28363 = VERTEX_POINT ( 'NONE', #10489 ) ;
#28364 = CARTESIAN_POINT ( 'NONE',  ( -36.77443515226921278, -5.298557911012516719, 1.088945631943563752 ) ) ;
#28365 = CARTESIAN_POINT ( 'NONE',  ( -35.85663232820584767, 4.817150320980633005, 2.203324261490556157 ) ) ;
#28366 = EDGE_CURVE ( 'NONE', #20869, #9056, #5426, .T. ) ;
#28367 = EDGE_LOOP ( 'NONE', ( #18061, #20087, #4380, #14449, #4445 ) ) ;
#28368 = CARTESIAN_POINT ( 'NONE',  ( 58.70362814788219907, 0.5000000000006148415, 1.816403611747777980 ) ) ;
#28369 = AXIS2_PLACEMENT_3D ( 'NONE', #8687, #11076, #1416 ) ;
#28370 = VERTEX_POINT ( 'NONE', #15379 ) ;
#28371 = CARTESIAN_POINT ( 'NONE',  ( 58.74154451056408988, 1.872697749444274029, 0.09314201707211816617 ) ) ;
#28372 = ORIENTED_EDGE ( 'NONE', *, *, #27636, .F. ) ;
#28373 = CARTESIAN_POINT ( 'NONE',  ( -56.64405989232412253, -2.944486372867076263, -1.700000000000211786 ) ) ;
#28374 = ORIENTED_EDGE ( 'NONE', *, *, #12289, .F. ) ;
#28375 = ORIENTED_EDGE ( 'NONE', *, *, #12639, .T. ) ;
#28376 = ADVANCED_FACE ( 'NONE', ( #15708 ), #8108, .F. ) ;
#28377 = ORIENTED_EDGE ( 'NONE', *, *, #30832, .F. ) ;
#28378 = CARTESIAN_POINT ( 'NONE',  ( -61.18749999999995737, 1.962990915244749557, -3.400000000000207745 ) ) ;
#28379 = CARTESIAN_POINT ( 'NONE',  ( -57.37499999999997158, 1.184343223768581366, 3.558065644182728082 ) ) ;
#28380 = CARTESIAN_POINT ( 'NONE',  ( 22.07284336892448096, 7.567314370317723693, -1.425000000000076428 ) ) ;
#28381 = CARTESIAN_POINT ( 'NONE',  ( 50.25000000000000711, 0.8897917884446137071, -1.791164585742097914 ) ) ;
#28382 = VECTOR ( 'NONE', #28476, 1000.000000000000000 ) ;
#28383 = CARTESIAN_POINT ( 'NONE',  ( 22.07280086217095061, 8.086143481909148889, 1.949999999999923128 ) ) ;
#28384 = EDGE_CURVE ( 'NONE', #26849, #236, #29187, .T. ) ;
#28386 = DIRECTION ( 'NONE',  ( -1.016952486242704214E-14, 0.000000000000000000, -1.000000000000000000 ) ) ;
#28385 = DIRECTION ( 'NONE',  ( 1.000000000000000000, 1.047444401652940007E-14, 0.000000000000000000 ) ) ;
#28387 = ADVANCED_FACE ( 'NONE', ( #30407 ), #20318, .T. ) ;
#28388 = EDGE_CURVE ( 'NONE', #4931, #17369, #23156, .T. ) ;
#28389 = SURFACE_STYLE_FILL_AREA ( #23656 ) ;
#28390 = CARTESIAN_POINT ( 'NONE',  ( 51.18410987668590195, -1.003361152472067586, -1.282358977530923871 ) ) ;
#28391 = CARTESIAN_POINT ( 'NONE',  ( 50.50000000000002132, 2.428612866367529932E-14, -4.000000000000022204 ) ) ;
#28392 = CARTESIAN_POINT ( 'NONE',  ( 58.65844932252336008, -1.607045716458009865, -0.9660788770022267213 ) ) ;
#28393 =( BOUNDED_CURVE ( )  B_SPLINE_CURVE ( 2, ( #15835, #29779, #25013, #22504, #8096, #8553, #25188, #3343, #18237 ),
 .UNSPECIFIED., .F., .T. ) 
 B_SPLINE_CURVE_WITH_KNOTS ( ( 3, 2, 2, 2, 3 ),
 ( 0.02777777777777778317, 0.03703703703703703498, 0.05555555555555555247, 0.07407407407407406996, 0.08333333333333332871 ),
 .UNSPECIFIED. ) 
 CURVE ( )  GEOMETRIC_REPRESENTATION_ITEM ( )  RATIONAL_B_SPLINE_CURVE ( ( 0.9330127018922194093, 0.9330127018922194093, 1.000000000000000000, 0.8660254037844387076, 1.000000000000000000, 0.8660254037844387076, 1.000000000000000000, 0.9330127018922194093, 0.9330127018922194093 ) ) 
 REPRESENTATION_ITEM ( '' )  );
#28394 = CARTESIAN_POINT ( 'NONE',  ( -54.39999999999996305, 1.600000000000021627, -3.363870538531679610 ) ) ;
#28395 = CARTESIAN_POINT ( 'NONE',  ( 50.33036399986576015, 1.366688880095624503, -3.854642372925540350 ) ) ;
#28396 = EDGE_LOOP ( 'NONE', ( #11737, #954, #2223, #26360, #26201, #1551 ) ) ;
#28398 = DIRECTION ( 'NONE',  ( -1.000000000000000000, 1.219044193948983948E-29, -3.491481338843133355E-15 ) ) ;
#28397 = CARTESIAN_POINT ( 'NONE',  ( 51.31943556899496173, -1.088761256243092612, -1.206353010735627729 ) ) ;
#28399 = LINE ( 'NONE', #11772, #12446 ) ;
#28400 = AXIS2_PLACEMENT_3D ( 'NONE', #18120, #15254, #2916 ) ;
#28401 = VERTEX_POINT ( 'NONE', #1276 ) ;
#28402 = DIRECTION ( 'NONE',  ( 1.000000000000000000, 1.047444401652940007E-14, 0.000000000000000000 ) ) ;
#28403 = FACE_OUTER_BOUND ( 'NONE', #26309, .T. ) ;
#28404 = CARTESIAN_POINT ( 'NONE',  ( -59.24999999999997158, -2.944486372867089141, 1.699999999999778799 ) ) ;
#28405 = VERTEX_POINT ( 'NONE', #17924 ) ;
#28406 = ORIENTED_EDGE ( 'NONE', *, *, #19474, .T. ) ;
#28407 = CARTESIAN_POINT ( 'NONE',  ( 16.07279755198631577, 5.034707333629180326, 1.977875755500474231 ) ) ;
#28408 = VERTEX_POINT ( 'NONE', #22694 ) ;
#28409 = CARTESIAN_POINT ( 'NONE',  ( 58.65844932252308297, -1.640171707772328347, 0.9087029769947272406 ) ) ;
#28410 = VECTOR ( 'NONE', #22586, 1000.000000000000114 ) ;
#28411 = CARTESIAN_POINT ( 'NONE',  ( -35.85663232820584057, -1.123735532908286316, 5.289358697221548944 ) ) ;
#28412 = VERTEX_POINT ( 'NONE', #3661 ) ;
#28413 = CARTESIAN_POINT ( 'NONE',  ( -62.39999999999998437, 2.749147127886321318, 0.06848408015298351748 ) ) ;
#28414 = CARTESIAN_POINT ( 'NONE',  ( -59.69142724121850563, -2.412383461849193278, -1.233589124872107146 ) ) ;
#28415 = ADVANCED_FACE ( 'NONE', ( #1440 ), #8711, .F. ) ;
#28416 = LINE ( 'NONE', #23044, #30854 ) ;
#28417 = ORIENTED_EDGE ( 'NONE', *, *, #19908, .T. ) ;
#28418 = EDGE_LOOP ( 'NONE', ( #10058, #11969, #24702, #1455 ) ) ;
#28419 = DIRECTION ( 'NONE',  ( 1.000000000000000000, 1.047444401652940007E-14, 0.000000000000000000 ) ) ;
#28420 = EDGE_CURVE ( 'NONE', #5818, #5953, #4932, .T. ) ;
#28421 = DIRECTION ( 'NONE',  ( -1.000000000000000000, -3.054025858079668409E-16, 2.042474015755241579E-16 ) ) ;
#28422 = CARTESIAN_POINT ( 'NONE',  ( 56.97364842551142061, -0.7795706648299629560, -2.480376902516343129 ) ) ;
#28423 = ORIENTED_EDGE ( 'NONE', *, *, #5976, .T. ) ;
#28424 = CARTESIAN_POINT ( 'NONE',  ( -57.99986116251333357, 1.737685414808516793, -3.471684241605569099 ) ) ;
#28425 = CARTESIAN_POINT ( 'NONE',  ( 58.50000000000001421, -0.8000000000000000444, 2.471260002560649927 ) ) ;
#28426 = DIRECTION ( 'NONE',  ( 9.754918421198724481E-16, 0.9601771338024399638, 0.2793919678926571892 ) ) ;
#28427 = DIRECTION ( 'NONE',  ( -1.000000000000000000, 0.000000000000000000, 0.000000000000000000 ) ) ;
#28429 = CARTESIAN_POINT ( 'NONE',  ( 58.66122797211809115, -0.9517229765811608955, 1.615588400946835534 ) ) ;
#28428 = CARTESIAN_POINT ( 'NONE',  ( -36.89017861346991367, -2.910597594660151000, 4.559461819278090466 ) ) ;
#28430 = AXIS2_PLACEMENT_3D ( 'NONE', #12433, #22125, #112 ) ;
#28431 = EDGE_CURVE ( 'NONE', #2309, #15602, #17087, .T. ) ;
#28432 = DIRECTION ( 'NONE',  ( 0.000000000000000000, 1.000000000000000000, 0.000000000000000000 ) ) ;
#28433 = LINE ( 'NONE', #7066, #2412 ) ;
#28434 = DIRECTION ( 'NONE',  ( 1.000000000000000000, 1.047444401652940007E-14, 0.000000000000000000 ) ) ;
#28435 = EDGE_LOOP ( 'NONE', ( #14410, #18510, #20676, #5430 ) ) ;
#28436 = ORIENTED_EDGE ( 'NONE', *, *, #9443, .T. ) ;
#28437 = CARTESIAN_POINT ( 'NONE',  ( -59.16550086808892672, -2.368432354959790320, 1.240591571384440872 ) ) ;
#28438 = ORIENTED_EDGE ( 'NONE', *, *, #10014, .T. ) ;
#28439 = CARTESIAN_POINT ( 'NONE',  ( 52.98705886115022423, 8.418976914897422503, 2.049999999999815081 ) ) ;
#28440 = AXIS2_PLACEMENT_3D ( 'NONE', #11656, #26370, #4671 ) ;
#28441 = CARTESIAN_POINT ( 'NONE',  ( -56.97085481156723574, 1.184343223768591136, 3.558065644182727194 ) ) ;
#28443 = DIRECTION ( 'NONE',  ( -1.000000000000000000, 0.000000000000000000, 0.000000000000000000 ) ) ;
#28442 = DIRECTION ( 'NONE',  ( 0.000000000000000000, 0.000000000000000000, 1.000000000000000000 ) ) ;
#28444 = EDGE_LOOP ( 'NONE', ( #16922, #6958, #21481, #10606 ) ) ;
#28445 = ORIENTED_EDGE ( 'NONE', *, *, #26516, .T. ) ;
#28446 = CARTESIAN_POINT ( 'NONE',  ( 51.70000000000001705, -4.276948333784438283, 0.9210526315789470120 ) ) ;
#28447 = EDGE_LOOP ( 'NONE', ( #2024, #19874, #25460, #7382 ) ) ;
#28448 = DIRECTION ( 'NONE',  ( 0.000000000000000000, 0.2008964009354147484, -0.9796124928211139560 ) ) ;
#28449 = ORIENTED_EDGE ( 'NONE', *, *, #23497, .T. ) ;
#28451 = CARTESIAN_POINT ( 'NONE',  ( -54.39999999999997726, 1.400000000000009681, -1.886605105831180521E-13 ) ) ;
#28450 = CARTESIAN_POINT ( 'NONE',  ( -36.52679053911622731, 4.797009389500119347, 2.498041539401855360 ) ) ;
#28452 = ORIENTED_EDGE ( 'NONE', *, *, #24799, .F. ) ;
#28453 = CARTESIAN_POINT ( 'NONE',  ( 57.00000000000001421, -0.6999999999999996225, 1.820027472320129736 ) ) ;
#28454 = EDGE_CURVE ( 'NONE', #6920, #23306, #16562, .T. ) ;
#28455 = CARTESIAN_POINT ( 'NONE',  ( 58.74999999305993725, 1.856692759305444529, -0.5240691109005866100 ) ) ;
#28456 = EDGE_CURVE ( 'NONE', #25278, #14364, #1877, .T. ) ;
#28457 = CARTESIAN_POINT ( 'NONE',  ( 47.10000000000001563, -4.079459090034584179, 2.128991905553722308 ) ) ;
#28458 = CARTESIAN_POINT ( 'NONE',  ( 51.12687253673779253, 0.9194130538826112975, -1.491219977510798378 ) ) ;
#28459 = EDGE_CURVE ( 'NONE', #12772, #23943, #1133, .T. ) ;
#28460 = CARTESIAN_POINT ( 'NONE',  ( -58.00952994616203284, 3.117691453623994580, -1.800000000000192557 ) ) ;
#28461 = CARTESIAN_POINT ( 'NONE',  ( -59.11985793442325843, -2.471172619865210862, -0.9613403835037039880 ) ) ;
#28462 = FACE_OUTER_BOUND ( 'NONE', #19310, .T. ) ;
#28463 = DIRECTION ( 'NONE',  ( 0.000000000000000000, -1.000000000000000000, -3.613946018757958434E-15 ) ) ;
#28464 = CIRCLE ( 'NONE', #4177, 0.01000000000000001929 ) ;
#28465 = CARTESIAN_POINT ( 'NONE',  ( -57.23542740578360366, 2.936324665650198895, 2.606018187048508850 ) ) ;
#28466 = ADVANCED_FACE ( 'NONE', ( #3975 ), #22579, .T. ) ;
#28467 = DIRECTION ( 'NONE',  ( 8.860386339788720432E-15, -0.8459051693633012903, -0.5333333333333335480 ) ) ;
#28468 = ORIENTED_EDGE ( 'NONE', *, *, #18757, .T. ) ;
#28469 = FACE_OUTER_BOUND ( 'NONE', #21458, .T. ) ;
#28470 = CARTESIAN_POINT ( 'NONE',  ( 58.75000000000002132, 6.153735859711025284E-13, 3.111507638930570854E-58 ) ) ;
#28471 = CARTESIAN_POINT ( 'NONE',  ( -36.92443669619682112, -0.1565107631087878926, 5.407502298984291578 ) ) ;
#28472 = CARTESIAN_POINT ( 'NONE',  ( -44.59999999999996589, 1.600000000000021627, -3.363870538531645416 ) ) ;
#28473 = VERTEX_POINT ( 'NONE', #18557 ) ;
#28474 = CARTESIAN_POINT ( 'NONE',  ( -54.46439202372638277, 1.502116081466616793, 4.031358338852112588 ) ) ;
#28475 = ORIENTED_EDGE ( 'NONE', *, *, #7687, .F. ) ;
#28476 = DIRECTION ( 'NONE',  ( -0.000000000000000000, 0.000000000000000000, 1.000000000000000000 ) ) ;
#28478 = CARTESIAN_POINT ( 'NONE',  ( -64.32138495697122949, 2.298612619042725846, 0.05726080253995516345 ) ) ;
#28477 = CARTESIAN_POINT ( 'NONE',  ( 50.50000000000002132, 5.291762632692320630E-13, 3.111507638930570854E-58 ) ) ;
#28479 = EDGE_LOOP ( 'NONE', ( #14328, #27120, #19076, #14686, #19954, #7650, #14914, #15461, #18445, #11635 ) ) ;
#28480 = EDGE_LOOP ( 'NONE', ( #29760, #19430, #14120, #23168 ) ) ;
#28481 = CARTESIAN_POINT ( 'NONE',  ( 61.25000000000001421, 1.039502773797226221, -1.800471618823823450 ) ) ;
#28482 = CARTESIAN_POINT ( 'NONE',  ( 22.06071280439820015, 8.185410187602871090, -1.425000000000076650 ) ) ;
#28484 = CARTESIAN_POINT ( 'NONE',  ( -44.59999999999999432, -1.500000000000006883, 4.029888335921774534 ) ) ;
#28483 = DIRECTION ( 'NONE',  ( 6.938893903907228378E-15, 8.673617379884035472E-16, 1.000000000000000000 ) ) ;
#28485 = ORIENTED_EDGE ( 'NONE', *, *, #24721, .F. ) ;
#28486 = CARTESIAN_POINT ( 'NONE',  ( -55.18749999999997158, 3.238593381231846369, 2.874284765127020691 ) ) ;
#28487 = AXIS2_PLACEMENT_3D ( 'NONE', #12051, #16955, #27222 ) ;
#28488 = DIRECTION ( 'NONE',  ( -1.000000000000000000, -2.586136946169074517E-16, 0.000000000000000000 ) ) ;
#28489 = CIRCLE ( 'NONE', #4722, 0.05000000000000002359 ) ;
#28490 = CARTESIAN_POINT ( 'NONE',  ( -35.85663232820584057, 3.275050215670975540, -2.949461045525604508 ) ) ;
#28491 = EDGE_CURVE ( 'NONE', #9827, #6367, #21897, .T. ) ;
#28492 = DIRECTION ( 'NONE',  ( 1.000000000000000000, 0.000000000000000000, 0.000000000000000000 ) ) ;
#28493 = DIRECTION ( 'NONE',  ( -1.000000000000000000, 0.000000000000000000, 1.047444401652940007E-14 ) ) ;
#28494 = CARTESIAN_POINT ( 'NONE',  ( -54.49983703358571319, 1.542636180423123449, -4.059406436927352146 ) ) ;
#28495 = ORIENTED_EDGE ( 'NONE', *, *, #16679, .F. ) ;
#28496 = CARTESIAN_POINT ( 'NONE',  ( 57.00000000000001421, -0.6999999999999999556, 1.820027472320129736 ) ) ;
#28497 = CARTESIAN_POINT ( 'NONE',  ( -36.43290890416709971, 3.561547362098881120, -4.076645242318375217 ) ) ;
#28498 = CARTESIAN_POINT ( 'NONE',  ( 58.75000000000002132, 6.153735859711025284E-13, 3.111507638930570854E-58 ) ) ;
#28499 = CARTESIAN_POINT ( 'NONE',  ( -54.39999999999999147, -1.600000000000004530, 3.363870538531237742 ) ) ;
#28500 = CARTESIAN_POINT ( 'NONE',  ( 15.70940947763170925, -0.8934212604923321699, -5.334164326942877565 ) ) ;
#28501 = ADVANCED_FACE ( 'NONE', ( #16482 ), #9975, .T. ) ;
#28503 = CARTESIAN_POINT ( 'NONE',  ( 58.72419296898095098, -1.799118770101062026, -0.5284032650186377689 ) ) ;
#28502 = CARTESIAN_POINT ( 'NONE',  ( 51.64333574538936489, -0.8318165372340007302, 1.569663068107119974 ) ) ;
#28504 = CIRCLE ( 'NONE', #29027, 0.4576450603546982632 ) ;
#28505 = CIRCLE ( 'NONE', #19862, 2.000000000000000000 ) ;
#28506 = FACE_OUTER_BOUND ( 'NONE', #16259, .T. ) ;
#28508 = CARTESIAN_POINT ( 'NONE',  ( -57.28335481156723574, 0.7533615035078095046, -3.673546848079178861 ) ) ;
#28507 = FACE_OUTER_BOUND ( 'NONE', #25867, .T. ) ;
#28509 = ORIENTED_EDGE ( 'NONE', *, *, #12165, .F. ) ;
#28510 = DIRECTION ( 'NONE',  ( 1.000000000000000000, 1.047444401652940007E-14, 0.000000000000000000 ) ) ;
#28511 = DIRECTION ( 'NONE',  ( 0.000000000000000000, 0.000000000000000000, 1.000000000000000000 ) ) ;
#28513 = CARTESIAN_POINT ( 'NONE',  ( -36.04518387042686101, 5.340403875751171370, 0.9205822004573066542 ) ) ;
#28512 = DIRECTION ( 'NONE',  ( -3.002035892788117459E-16, 0.9996898646859344595, 0.02490330187381124133 ) ) ;
#28514 = CARTESIAN_POINT ( 'NONE',  ( 51.31572262954152563, 1.002608958138273554, -1.584424273060082378 ) ) ;
#28515 = ORIENTED_EDGE ( 'NONE', *, *, #4583, .T. ) ;
#28516 = VERTEX_POINT ( 'NONE', #18718 ) ;
#28517 = CARTESIAN_POINT ( 'NONE',  ( -35.98952425903308949, -4.804073785499180183, 2.042134698606323351 ) ) ;
#28518 = CARTESIAN_POINT ( 'NONE',  ( -35.85663232820584057, 4.945493884734773360, 1.606888370749773864 ) ) ;
#28519 = VERTEX_POINT ( 'NONE', #25973 ) ;
#28520 = CARTESIAN_POINT ( 'NONE',  ( 58.71354657862811166, 0.5000000000006149525, 1.821913688936171116 ) ) ;
#28521 = EDGE_LOOP ( 'NONE', ( #27966, #1583, #28160, #5090, #7071, #8011, #9378, #17234 ) ) ;
#28522 = CARTESIAN_POINT ( 'NONE',  ( 58.74999999305994436, 1.929066554548210410, -0.02566444196698207739 ) ) ;
#28523 = VERTEX_POINT ( 'NONE', #2071 ) ;
#28524 = EDGE_CURVE ( 'NONE', #19651, #21736, #26141, .T. ) ;
#28525 = CARTESIAN_POINT ( 'NONE',  ( -60.76905989232411542, 2.944486372867092250, 1.699999999999795675 ) ) ;
#28526 = SURFACE_SIDE_STYLE ('',( #20942 ) ) ;
#28527 = ORIENTED_EDGE ( 'NONE', *, *, #4331, .T. ) ;
#28528 = AXIS2_PLACEMENT_3D ( 'NONE', #15346, #15677, #13267 ) ;
#28529 = EDGE_LOOP ( 'NONE', ( #22026, #22732, #24897, #21166 ) ) ;
#28530 = CARTESIAN_POINT ( 'NONE',  ( -60.56249999999995026, -1.962990915244707368, -3.400000000000221956 ) ) ;
#28531 = CARTESIAN_POINT ( 'NONE',  ( -67.98046642889043767, -3.207269654211098678E-16, 2.198325388322918801E-15 ) ) ;
#28532 = CARTESIAN_POINT ( 'NONE',  ( 29.45665666413593087, 6.177494273110403000, -1.425000000000101963 ) ) ;
#28533 = FACE_OUTER_BOUND ( 'NONE', #18946, .T. ) ;
#28534 = VECTOR ( 'NONE', #12293, 1000.000000000000000 ) ;
#28535 = CARTESIAN_POINT ( 'NONE',  ( 61.25000000000001421, 1.000000000000641709, 1.586072192556190252 ) ) ;
#28536 = ADVANCED_FACE ( 'NONE', ( #28361 ), #2894, .F. ) ;
#28538 = CARTESIAN_POINT ( 'NONE',  ( -57.99999999999997158, -2.489203624310590612, 2.804704140674912693 ) ) ;
#28537 = CARTESIAN_POINT ( 'NONE',  ( -35.85663232820584767, 5.377732432866631385, -0.5657657256215208319 ) ) ;
#28539 =( BOUNDED_SURFACE ( )  B_SPLINE_SURFACE ( 3, 2, ( 
 ( #8909, #18596, #28244 ),
 ( #13330, #16212, #25861 ),
 ( #4163, #5934, #15591 ),
 ( #23028, #25237, #3556 ),
 ( #13193, #2258, #9246 ),
 ( #9399, #4635, #23813 ),
 ( #21608, #14138, #4789 ),
 ( #7033, #2105, #11769 ),
 ( #13966, #30772, #28873 ),
 ( #21444, #2432, #7331 ) ),
 .UNSPECIFIED., .F., .F., .F. ) 
 B_SPLINE_SURFACE_WITH_KNOTS ( ( 4, 2, 2, 2, 4 ),
 ( 3, 3 ),
 ( 0.0004005301535625021940, 0.0008279283193725978313, 0.001041627402277645704, 0.001148476943730169586, 0.001255326485182693469 ),
 ( 0.000000000000000000, 1.000000000000000000 ),
 .UNSPECIFIED. ) 
 GEOMETRIC_REPRESENTATION_ITEM ( )  RATIONAL_B_SPLINE_SURFACE ( (
 ( 1.000000000000000000, 0.7071067811865475727, 1.000000000000000000),
 ( 1.000000000000000000, 0.7463463187144472322, 1.000000000000000000),
 ( 1.000000000000000000, 0.7946150999565784190, 1.000000000000000000),
 ( 1.000000000000000000, 0.8720431506958271628, 1.000000000000000000),
 ( 1.000000000000000000, 0.8987780092779085184, 1.000000000000000000),
 ( 1.000000000000000000, 0.9375340664365013899, 1.000000000000000000),
 ( 1.000000000000000000, 0.9504270566176250545, 1.000000000000000000),
 ( 1.000000000000000000, 0.9732249474031241521, 1.000000000000000000),
 ( 1.000000000000000000, 0.9839441327696755168, 1.000000000000000000),
 ( 1.000000000000000000, 0.9842509842514762797, 1.000000000000000000) ) ) 
 REPRESENTATION_ITEM ( '' )  SURFACE ( )  );
#28540 = CARTESIAN_POINT ( 'NONE',  ( 46.92078115823489526, -4.254539148539595139, 1.020319270753726082 ) ) ;
#28541 = DIRECTION ( 'NONE',  ( 0.000000000000000000, 0.000000000000000000, 1.000000000000000000 ) ) ;
#28542 = CARTESIAN_POINT ( 'NONE',  ( 15.56274145962646394, 5.369990034204301210, -0.6654225812208519608 ) ) ;
#28543 = ORIENTED_EDGE ( 'NONE', *, *, #20843, .T. ) ;
#28544 = DIRECTION ( 'NONE',  ( 0.000000000000000000, -1.000000000000000000, -3.491481338843129805E-15 ) ) ;
#28545 = TOROIDAL_SURFACE ( 'NONE', #1229, 1.524417381223824197, 0.05000000000000000278 ) ;
#28546 = CARTESIAN_POINT ( 'NONE',  ( 51.87765138016309407, 8.698644590117595499, 2.049999999999819522 ) ) ;
#28547 = ORIENTED_EDGE ( 'NONE', *, *, #20025, .T. ) ;
#28549 = CARTESIAN_POINT ( 'NONE',  ( 48.47377487419020525, -1.373801017329605134, -3.853344662332955473 ) ) ;
#28548 = CARTESIAN_POINT ( 'NONE',  ( -54.49999999999999289, 1.557046979865768899, 3.273565289174698467 ) ) ;
#28550 = EDGE_CURVE ( 'NONE', #17250, #14688, #9361, .T. ) ;
#28551 = CARTESIAN_POINT ( 'NONE',  ( 54.29335997410981207, 6.002961067146851626, -2.050000000000190781 ) ) ;
#28552 = DIRECTION ( 'NONE',  ( 1.000000000000000000, 1.047444401652940007E-14, 0.000000000000000000 ) ) ;
#28553 = ORIENTED_EDGE ( 'NONE', *, *, #26122, .T. ) ;
#28554 = CARTESIAN_POINT ( 'NONE',  ( 22.58314801556728568, 7.622751244490449274, -1.425000000000078426 ) ) ;
#28555 = CARTESIAN_POINT ( 'NONE',  ( 60.89332643996548455, 0.5000000000006328271, -1.718465855720773483 ) ) ;
#28556 = CARTESIAN_POINT ( 'NONE',  ( -55.50952994616206126, -4.643455692769921685E-15, 3.599999999999801581 ) ) ;
#28557 = VERTEX_POINT ( 'NONE', #7291 ) ;
#28558 = EDGE_LOOP ( 'NONE', ( #10182, #3825, #183, #1414, #18837, #25119, #3514, #17280, #20564 ) ) ;
#28559 = CARTESIAN_POINT ( 'NONE',  ( 16.07512358269905306, 5.233646053067070980, 1.367284724151327513 ) ) ;
#28560 = ORIENTED_EDGE ( 'NONE', *, *, #13848, .T. ) ;
#28561 = CARTESIAN_POINT ( 'NONE',  ( 58.73371041428940487, -1.662559130997790513, 0.8671977075801986512 ) ) ;
#28562 = ADVANCED_FACE ( 'NONE', ( #5220 ), #7471, .T. ) ;
#28563 = CARTESIAN_POINT ( 'NONE',  ( -57.57202994616204705, -4.156921938165296204, -2.193920212522006445E-13 ) ) ;
#28564 = ORIENTED_EDGE ( 'NONE', *, *, #27876, .F. ) ;
#28565 = CARTESIAN_POINT ( 'NONE',  ( 58.45000000000001705, 0.8000000000000000444, 2.421260002560649660 ) ) ;
#28566 = EDGE_CURVE ( 'NONE', #26219, #14020, #16960, .T. ) ;
#28567 = FACE_OUTER_BOUND ( 'NONE', #10033, .T. ) ;
#28568 = EDGE_CURVE ( 'NONE', #6093, #30315, #7747, .T. ) ;
#28569 = VECTOR ( 'NONE', #21551, 1000.000000000000000 ) ;
#28570 = CARTESIAN_POINT ( 'NONE',  ( 33.98208436309214164, 8.188484713949170768, 2.049999999999878586 ) ) ;
#28571 = VERTEX_POINT ( 'NONE', #7610 ) ;
#28572 = VERTEX_POINT ( 'NONE', #26773 ) ;
#28573 = FACE_OUTER_BOUND ( 'NONE', #23318, .T. ) ;
#28575 = CARTESIAN_POINT ( 'NONE',  ( 56.96603746669009638, -0.7703957983921196906, -2.483260519405945388 ) ) ;
#28574 = CIRCLE ( 'NONE', #21514, 0.04999999999999969746 ) ;
#28576 = ORIENTED_EDGE ( 'NONE', *, *, #1669, .F. ) ;
#28577 = CARTESIAN_POINT ( 'NONE',  ( 61.25000000000003553, -0.9999999999993586242, -1.546164609606622831 ) ) ;
#28578 = CARTESIAN_POINT ( 'NONE',  ( -44.59999999999996589, 1.514093959731561467, -3.183260039818548659 ) ) ;
#28579 = ADVANCED_FACE ( 'NONE', ( #12203 ), #24079, .T. ) ;
#28580 = DIRECTION ( 'NONE',  ( 0.000000000000000000, -1.000000000000000000, 0.000000000000000000 ) ) ;
#28581 = CIRCLE ( 'NONE', #18986, 3.020710678118645909 ) ;
#28582 = CARTESIAN_POINT ( 'NONE',  ( -58.92306624327022746, -3.399999999999988365, -0.9110272542660498019 ) ) ;
#28584 = CARTESIAN_POINT ( 'NONE',  ( 58.73371041428940487, -1.006219588947987686, 1.582294810367148363 ) ) ;
#28583 = CARTESIAN_POINT ( 'NONE',  ( 50.50000000000002132, 0.6462379109121000331, -4.048750000000023164 ) ) ;
#28585 = CYLINDRICAL_SURFACE ( 'NONE', #12442, 4.700000000000000178 ) ;
#28586 = CARTESIAN_POINT ( 'NONE',  ( -55.93749999999997868, 3.238593381231842816, 2.874284765127024688 ) ) ;
#28587 = DIRECTION ( 'NONE',  ( 1.000000000000000000, 0.000000000000000000, 0.000000000000000000 ) ) ;
#28588 = ORIENTED_EDGE ( 'NONE', *, *, #10469, .F. ) ;
#28589 = EDGE_CURVE ( 'NONE', #24526, #24661, #8478, .T. ) ;
#28590 = CIRCLE ( 'NONE', #27059, 4.099999999999992539 ) ;
#28591 = TOROIDAL_SURFACE ( 'NONE', #23039, 3.524999999999996358, 0.1000000000000000056 ) ;
#28592 = ORIENTED_EDGE ( 'NONE', *, *, #26901, .F. ) ;
#28593 = CARTESIAN_POINT ( 'NONE',  ( 51.50000000000001421, 1.990051048615613918E-16, -1.625000000000181188 ) ) ;
#28594 = ORIENTED_EDGE ( 'NONE', *, *, #2080, .F. ) ;
#28595 = EDGE_CURVE ( 'NONE', #6234, #17704, #21732, .T. ) ;
#28596 = CARTESIAN_POINT ( 'NONE',  ( 52.88620718028473533, 4.625382794676503373, 2.049999999999815081 ) ) ;
#28597 = CARTESIAN_POINT ( 'NONE',  ( -54.73542740578361077, -3.725040285533364859, 1.239922660687674760 ) ) ;
#28599 = CARTESIAN_POINT ( 'NONE',  ( -36.76447480099743359, 3.646691605040315309, 3.993181011920730050 ) ) ;
#28598 = DIRECTION ( 'NONE',  ( 0.000000000000000000, 0.000000000000000000, 1.000000000000000000 ) ) ;
#28600 = ORIENTED_EDGE ( 'NONE', *, *, #27270, .F. ) ;
#28601 = CARTESIAN_POINT ( 'NONE',  ( 22.40895431619513900, 7.071232237904418128, -2.050000000000078870 ) ) ;
#28602 = ORIENTED_EDGE ( 'NONE', *, *, #6084, .T. ) ;
#28603 = CIRCLE ( 'NONE', #29599, 0.1000000000000000472 ) ;
#28604 = DIRECTION ( 'NONE',  ( -0.9993908270190957621, 0.03489949670250098307, 3.491481338843133355E-15 ) ) ;
#28605 = ORIENTED_EDGE ( 'NONE', *, *, #18193, .F. ) ;
#28607 = FACE_OUTER_BOUND ( 'NONE', #28869, .T. ) ;
#28606 = DIRECTION ( 'NONE',  ( -3.491481338843133355E-15, 5.182136041040898961E-15, 1.000000000000000000 ) ) ;
#28608 = AXIS2_PLACEMENT_3D ( 'NONE', #21277, #30907, #7306 ) ;
#28609 =( REPRESENTATION_RELATIONSHIP ('NONE','NONE', #7047, #9258 ) REPRESENTATION_RELATIONSHIP_WITH_TRANSFORMATION ( #10914 )SHAPE_REPRESENTATION_RELATIONSHIP( ) );
#28610 = EDGE_CURVE ( 'NONE', #30315, #13545, #14578, .T. ) ;
#28611 = ORIENTED_EDGE ( 'NONE', *, *, #28851, .F. ) ;
#28612 = DIRECTION ( 'NONE',  ( -1.015447888376667464E-14, 0.000000000000000000, -1.000000000000000000 ) ) ;
#28613 = EDGE_CURVE ( 'NONE', #24288, #21815, #23, .T. ) ;
#28614 = DIRECTION ( 'NONE',  ( 1.000000000000000000, 1.047444401652940007E-14, 0.000000000000000000 ) ) ;
#28615 = CARTESIAN_POINT ( 'NONE',  ( -56.67499999999996874, 0.9743475445367648646, -4.751120590182402736 ) ) ;
#28616 = PLANE ( 'NONE',  #4624 ) ;
#28617 = CARTESIAN_POINT ( 'NONE',  ( -57.75952994616205416, -4.643455692769894075E-15, 3.599999999999794031 ) ) ;
#28618 = LINE ( 'NONE', #21507, #13466 ) ;
#28619 = VECTOR ( 'NONE', #12187, 1000.000000000000000 ) ;
#28620 = CARTESIAN_POINT ( 'NONE',  ( 29.25706191173316739, 5.994885333997870269, 1.549999999999897904 ) ) ;
#28621 = CARTESIAN_POINT ( 'NONE',  ( -56.67499999999996874, -0.9643027244899884387, 4.702139965541347166 ) ) ;
#28622 = VECTOR ( 'NONE', #29862, 1000.000000000000000 ) ;
#28623 = AXIS2_PLACEMENT_3D ( 'NONE', #21428, #26324, #31060 ) ;
#28624 = CARTESIAN_POINT ( 'NONE',  ( -57.11042740578360366, -0.7887156198831699605, 3.845940847736171619 ) ) ;
#28625 = DIRECTION ( 'NONE',  ( 1.000000000000000000, 1.047444401652940007E-14, 0.000000000000000000 ) ) ;
#28626 = ORIENTED_EDGE ( 'NONE', *, *, #2294, .F. ) ;
#28627 = B_SPLINE_CURVE_WITH_KNOTS ( 'NONE', 3,
 ( #4521, #14173, #9438, #28752, #7065, #21647, #16728, #31276, #10813, #12870, #2924, #22554, #12566 ),
 .UNSPECIFIED., .F., .F.,
 ( 4, 3, 3, 3, 4 ),
 ( 0.000000000000000000, 3.429247765842821492E-05, 6.861252194980687496E-05, 0.0001025118211733554781, 0.0001105094600589149093 ),
 .UNSPECIFIED. ) ;
#28628 = EDGE_CURVE ( 'NONE', #7995, #20300, #18621, .T. ) ;
#28629 = DIRECTION ( 'NONE',  ( 0.000000000000000000, 0.000000000000000000, 1.000000000000000000 ) ) ;
#28630 = CARTESIAN_POINT ( 'NONE',  ( -36.11780688638206982, -1.123735543662337300, 5.289358694936827199 ) ) ;
#28631 = CYLINDRICAL_SURFACE ( 'NONE', #26157, 0.4500000000000001221 ) ;
#28632 = ADVANCED_FACE ( 'NONE', ( #170 ), #29297, .T. ) ;
#28633 = ORIENTED_EDGE ( 'NONE', *, *, #13438, .T. ) ;
#28634 = CONICAL_SURFACE ( 'NONE', #12434, 2.750000000000000000, 0.7853981633974466137 ) ;
#28635 = CARTESIAN_POINT ( 'NONE',  ( -35.85663232820583346, -5.377732432866661583, 0.5657657256215455899 ) ) ;
#28636 = ORIENTED_EDGE ( 'NONE', *, *, #24908, .T. ) ;
#28637 = EDGE_CURVE ( 'NONE', #14166, #12730, #5076, .T. ) ;
#28638 =( NAMED_UNIT ( * ) SI_UNIT ( $, .STERADIAN. ) SOLID_ANGLE_UNIT ( ) );
#28640 = CARTESIAN_POINT ( 'NONE',  ( 65.00000000000001421, -1.025519176787267142E-28, -6.808388610744108654E-13 ) ) ;
#28639 = CARTESIAN_POINT ( 'NONE',  ( 58.75000000000001421, 1.022750809562429142, -1.571497941946046417 ) ) ;
#28641 = ORIENTED_EDGE ( 'NONE', *, *, #26550, .F. ) ;
#28642 = ORIENTED_EDGE ( 'NONE', *, *, #5008, .F. ) ;
#28643 = DIRECTION ( 'NONE',  ( 1.000000000000000000, 0.000000000000000000, -0.000000000000000000 ) ) ;
#28644 = LINE ( 'NONE', #19165, #17679 ) ;
#28645 = AXIS2_PLACEMENT_3D ( 'NONE', #13497, #6229, #15587 ) ;
#28647 = CARTESIAN_POINT ( 'NONE',  ( 58.65000000000003411, -1.253243060178072188, 1.394635017527513510 ) ) ;
#28646 = LINE ( 'NONE', #16776, #26172 ) ;
#28648 = ORIENTED_EDGE ( 'NONE', *, *, #22571, .T. ) ;
#28649 = CARTESIAN_POINT ( 'NONE',  ( -60.42292740578359656, 2.256877952708268520, -2.542931754211924300 ) ) ;
#28650 = DIRECTION ( 'NONE',  ( 0.000000000000000000, 0.000000000000000000, 1.000000000000000000 ) ) ;
#28651 = CARTESIAN_POINT ( 'NONE',  ( -74.38999999999998636, -2.585162900687033808E-15, 4.707972083073595634E-15 ) ) ;
#28652 = AXIS2_PLACEMENT_3D ( 'NONE', #21800, #19105, #14645 ) ;
#28653 = CARTESIAN_POINT ( 'NONE',  ( 50.34192419032898158, 8.193354243125561709, 2.049999999999823963 ) ) ;
#28654 = CIRCLE ( 'NONE', #18033, 4.314644660940672338 ) ;
#28655 = CONICAL_SURFACE ( 'NONE', #14979, 2.750000000000000000, 0.7853981633974466137 ) ;
#28656 = DIRECTION ( 'NONE',  ( -0.9956821769042226711, -0.09282781153979745292, 3.494196887668849000E-15 ) ) ;
#28657 = CARTESIAN_POINT ( 'NONE',  ( 54.15673930838963912, 5.684321142249388892, 2.049999999999811529 ) ) ;
#28658 = CIRCLE ( 'NONE', #26614, 0.1500000000000000777 ) ;
#28659 = DIRECTION ( 'NONE',  ( 0.000000000000000000, 0.000000000000000000, 1.000000000000000000 ) ) ;
#28660 = ORIENTED_EDGE ( 'NONE', *, *, #29021, .F. ) ;
#28661 = CARTESIAN_POINT ( 'NONE',  ( 69.20000000000005969, -0.8558823529411765385, 2.268940368965341126 ) ) ;
#28662 = AXIS2_PLACEMENT_3D ( 'NONE', #16738, #2307, #11974 ) ;
#28663 = CARTESIAN_POINT ( 'NONE',  ( -36.76447480099743359, 2.670851142931450539, -4.702170608191241108 ) ) ;
#28664 = CARTESIAN_POINT ( 'NONE',  ( -54.49999999999996447, 1.600000000000021627, -3.363870538531680054 ) ) ;
#28665 = CARTESIAN_POINT ( 'NONE',  ( -59.09999999999997300, 2.465712773623992327, -0.9709585562669131864 ) ) ;
#28666 = CIRCLE ( 'NONE', #11455, 2.729289321881338548 ) ;
#28667 = CIRCLE ( 'NONE', #27639, 2.000000000000000000 ) ;
#28668 = CARTESIAN_POINT ( 'NONE',  ( -62.34999999999997300, 1.091670395932995432E-15, 2.248789515065420326E-15 ) ) ;
#28669 = VECTOR ( 'NONE', #6505, 1000.000000000000000 ) ;
#28671 = DIRECTION ( 'NONE',  ( -1.000000000000000000, -3.054025858079668409E-16, 2.042474015755241579E-16 ) ) ;
#28670 = CARTESIAN_POINT ( 'NONE',  ( -55.37486116251335488, -1.737685414808514350, 3.471684241605565990 ) ) ;
#28672 = CIRCLE ( 'NONE', #21619, 4.600000000000036948 ) ;
#28673 = CARTESIAN_POINT ( 'NONE',  ( 47.00000000000000711, -4.020776289669854897, -2.234582293948742304 ) ) ;
#28674 = AXIS2_PLACEMENT_3D ( 'NONE', #20305, #15535, #1427 ) ;
#28676 = DIRECTION ( 'NONE',  ( 1.000000000000000000, 3.053848253006669023E-16, -2.042510438544995415E-16 ) ) ;
#28675 = DIRECTION ( 'NONE',  ( 1.000000000000000000, 2.586136946169074517E-16, -0.000000000000000000 ) ) ;
#28677 = EDGE_CURVE ( 'NONE', #17963, #18266, #4954, .T. ) ;
#28678 = VERTEX_POINT ( 'NONE', #24530 ) ;
#28679 = CIRCLE ( 'NONE', #21095, 1.625000000000000222 ) ;
#28680 = AXIS2_PLACEMENT_3D ( 'NONE', #28578, #19259, #26208 ) ;
#28681 = DIRECTION ( 'NONE',  ( -1.000000000000000000, 0.000000000000000000, 3.491481338843133355E-15 ) ) ;
#28683 = CARTESIAN_POINT ( 'NONE',  ( -36.68133364217572989, 5.320649567603461527, 0.9667173501064365571 ) ) ;
#28682 = CARTESIAN_POINT ( 'NONE',  ( 15.74504787372211645, -3.003531019938647795, -4.498666779076351929 ) ) ;
#28684 = CARTESIAN_POINT ( 'NONE',  ( 15.41217651307628600, -5.027944117023993797, 1.353132643598594864 ) ) ;
#28685 = ORIENTED_EDGE ( 'NONE', *, *, #4355, .T. ) ;
#28686 = ORIENTED_EDGE ( 'NONE', *, *, #14110, .T. ) ;
#28687 = CARTESIAN_POINT ( 'NONE',  ( 69.20000000000000284, 0.8382352941176473005, -2.222158093318006067 ) ) ;
#28688 = ORIENTED_EDGE ( 'NONE', *, *, #15293, .F. ) ;
#28689 = DIRECTION ( 'NONE',  ( -1.000000000000000000, -3.053848253006669023E-16, 2.042510438544995415E-16 ) ) ;
#28690 = CARTESIAN_POINT ( 'NONE',  ( -56.56249999999997158, -0.7533615035078050637, 3.673546848079176197 ) ) ;
#28691 = AXIS2_PLACEMENT_3D ( 'NONE', #20818, #31216, #30448 ) ;
#28692 = EDGE_LOOP ( 'NONE', ( #25974, #11502, #21734, #3248 ) ) ;
#28693 = DIRECTION ( 'NONE',  ( 1.009293658750142281E-14, 0.000000000000000000, 1.000000000000000000 ) ) ;
#28694 = ORIENTED_EDGE ( 'NONE', *, *, #4275, .F. ) ;
#28695 =( NAMED_UNIT ( * ) SI_UNIT ( $, .STERADIAN. ) SOLID_ANGLE_UNIT ( ) );
#28696 = ADVANCED_FACE ( 'NONE', ( #2845 ), #17413, .T. ) ;
#28697 = CARTESIAN_POINT ( 'NONE',  ( -54.44999999999997442, 1.499999999999998890, 3.300094695611021756 ) ) ;
#28698 = ORIENTED_EDGE ( 'NONE', *, *, #2186, .T. ) ;
#28699 = AXIS2_PLACEMENT_3D ( 'NONE', #16613, #4406, #23263 ) ;
#28700 = ORIENTED_EDGE ( 'NONE', *, *, #3638, .F. ) ;
#28701 = ORIENTED_EDGE ( 'NONE', *, *, #19113, .T. ) ;
#28702 = VECTOR ( 'NONE', #592, 1000.000000000000000 ) ;
#28703 = CARTESIAN_POINT ( 'NONE',  ( -60.49999999999995737, 2.023778652682511576E-14, -3.400000000000214850 ) ) ;
#28704 = AXIS2_PLACEMENT_3D ( 'NONE', #13692, #13367, #4050 ) ;
#28705 = CIRCLE ( 'NONE', #31231, 2.374999999999998668 ) ;
#28706 = DIRECTION ( 'NONE',  ( -1.000000000000000000, 0.000000000000000000, 0.000000000000000000 ) ) ;
#28707 = CARTESIAN_POINT ( 'NONE',  ( -35.85663232820584057, 4.945493884734773360, 1.606888370749773864 ) ) ;
#28708 = DIRECTION ( 'NONE',  ( 0.000000000000000000, 0.000000000000000000, -1.000000000000000000 ) ) ;
#28709 = DIRECTION ( 'NONE',  ( -1.000000000000000000, -0.000000000000000000, -0.000000000000000000 ) ) ;
#28710 = DIRECTION ( 'NONE',  ( -1.000000000000000000, 0.000000000000000000, 0.000000000000000000 ) ) ;
#28711 = VECTOR ( 'NONE', #11337, 1000.000000000000000 ) ;
#28712 = AXIS2_PLACEMENT_3D ( 'NONE', #11553, #18364, #23585 ) ;
#28713 = CARTESIAN_POINT ( 'NONE',  ( 47.10000000000002984, -4.259946800035232073, 0.9999999999999998890 ) ) ;
#28714 = CARTESIAN_POINT ( 'NONE',  ( 51.23644008536124517, -1.080112125195908490, -1.214076932077872817 ) ) ;
#28715 = CARTESIAN_POINT ( 'NONE',  ( 15.74504787372188552, 5.206628483174362998, -1.466363261642694704 ) ) ;
#28716 = EDGE_CURVE ( 'NONE', #11715, #20935, #1903, .T. ) ;
#28717 = ORIENTED_EDGE ( 'NONE', *, *, #11304, .T. ) ;
#28719 = CARTESIAN_POINT ( 'NONE',  ( 61.00000000000003553, -0.9999999999993611777, 1.586072192556190252 ) ) ;
#28718 = AXIS2_PLACEMENT_3D ( 'NONE', #4555, #4395, #23879 ) ;
#28720 = CARTESIAN_POINT ( 'NONE',  ( 61.09423418604154676, -0.6373668173473425735, 1.895722432253304168 ) ) ;
#28721 = VERTEX_POINT ( 'NONE', #6940 ) ;
#28723 = CARTESIAN_POINT ( 'NONE',  ( 48.40000000000001990, -0.6304760106459033064, -3.950000000000022826 ) ) ;
#28722 = CARTESIAN_POINT ( 'NONE',  ( -35.85663232820584767, -4.383220986680273157, 0.4611378927884406398 ) ) ;
#28724 = CARTESIAN_POINT ( 'NONE',  ( 56.95000000000001705, 2.326828918379971365E-16, 1.899999999999999911 ) ) ;
#28725 = CARTESIAN_POINT ( 'NONE',  ( 51.51923570830314247, -3.793498434807317743, -1.557570148623113937 ) ) ;
#28726 = AXIS2_PLACEMENT_3D ( 'NONE', #4538, #18959, #28604 ) ;
#28727 = EDGE_LOOP ( 'NONE', ( #2403, #22565, #18566, #15561 ) ) ;
#28728 = CYLINDRICAL_SURFACE ( 'NONE', #7569, 1.899999999999999911 ) ;
#28729 = CARTESIAN_POINT ( 'NONE',  ( 51.30583474879431094, -4.280467579807392120, 1.378329539256710312 ) ) ;
#28730 = CARTESIAN_POINT ( 'NONE',  ( -55.00952994616204705, 3.117691453623994580, -1.800000000000181899 ) ) ;
#28731 = VERTEX_POINT ( 'NONE', #19295 ) ;
#28732 = ORIENTED_EDGE ( 'NONE', *, *, #19865, .F. ) ;
#28733 = CARTESIAN_POINT ( 'NONE',  ( -59.51599740598381771, 3.364165731847367447, -1.132304662275449569 ) ) ;
#28734 = ORIENTED_EDGE ( 'NONE', *, *, #20532, .T. ) ;
#28735 = CARTESIAN_POINT ( 'NONE',  ( 48.41845806530709240, -1.153441674035701636, 3.890342980189690270 ) ) ;
#28736 = CARTESIAN_POINT ( 'NONE',  ( -58.19702994616203284, -2.078460969082631227, -3.600000000000212363 ) ) ;
#28737 = ORIENTED_EDGE ( 'NONE', *, *, #4673, .F. ) ;
#28738 = DIRECTION ( 'NONE',  ( 1.000000000000000000, -0.000000000000000000, -0.000000000000000000 ) ) ;
#28739 = CARTESIAN_POINT ( 'NONE',  ( 48.40000000000001990, 1.391941090707534245, -3.850000000000022737 ) ) ;
#28740 = ORIENTED_EDGE ( 'NONE', *, *, #27093, .T. ) ;
#28741 = AXIS2_PLACEMENT_3D ( 'NONE', #6605, #18334, #23242 ) ;
#28742 = DIRECTION ( 'NONE',  ( 0.000000000000000000, -0.9996898646859344595, -0.02490330187381123786 ) ) ;
#28743 =( BOUNDED_CURVE ( )  B_SPLINE_CURVE ( 3, ( #13902, #18536, #26115, #9515 ),
 .UNSPECIFIED., .F., .T. ) 
 B_SPLINE_CURVE_WITH_KNOTS ( ( 4, 4 ),
 ( 5.439460278842602747, 5.455963239578336399 ),
 .UNSPECIFIED. ) 
 CURVE ( )  GEOMETRIC_REPRESENTATION_ITEM ( )  RATIONAL_B_SPLINE_CURVE ( ( 1.000000000000000000, 0.9999773044860189586, 0.9999773044860189586, 1.000000000000000000 ) ) 
 REPRESENTATION_ITEM ( '' )  );
#28744 = DIRECTION ( 'NONE',  ( 3.491481338843133355E-15, -0.000000000000000000, 1.000000000000000000 ) ) ;
#28745 = B_SPLINE_CURVE_WITH_KNOTS ( 'NONE', 3,
 ( #23411, #8669, #27848, #30846, #9315, #25457 ),
 .UNSPECIFIED., .F., .F.,
 ( 4, 2, 4 ),
 ( 0.000000000000000000, 0.0001939776071359000566, 0.0003879552142718001133 ),
 .UNSPECIFIED. ) ;
#28746 = ORIENTED_EDGE ( 'NONE', *, *, #29707, .T. ) ;
#28747 = FACE_OUTER_BOUND ( 'NONE', #28692, .T. ) ;
#28748 = LINE ( 'NONE', #28425, #19087 ) ;
#28749 = FACE_OUTER_BOUND ( 'NONE', #7340, .T. ) ;
#28751 = DIRECTION ( 'NONE',  ( 0.000000000000000000, 1.224646799147353454E-16, 1.000000000000000000 ) ) ;
#28750 = CARTESIAN_POINT ( 'NONE',  ( 58.75000000000000711, -0.5811678240976559939, -1.782657835994590156 ) ) ;
#28752 = CARTESIAN_POINT ( 'NONE',  ( 58.72973946705038628, -0.4999999999993850475, 1.835413506854427501 ) ) ;
#28753 = CARTESIAN_POINT ( 'NONE',  ( -56.15400635094609072, 1.737685414808526341, -3.471684241605562438 ) ) ;
#28754 = EDGE_CURVE ( 'NONE', #27818, #19242, #17597, .T. ) ;
#28755 = DIRECTION ( 'NONE',  ( -1.000000000000000000, -0.000000000000000000, -0.000000000000000000 ) ) ;
#28756 = ORIENTED_EDGE ( 'NONE', *, *, #2460, .F. ) ;
#28757 = ADVANCED_FACE ( 'NONE', ( #16603 ), #3931, .T. ) ;
#28758 = CIRCLE ( 'NONE', #19659, 4.700000000000000178 ) ;
#28759 = TOROIDAL_SURFACE ( 'NONE', #9563, 1.850000000000000089, 0.05000000000000000278 ) ;
#28760 = CARTESIAN_POINT ( 'NONE',  ( 58.74487987613195372, 0.5000000000003640421, -1.852860917432736620 ) ) ;
#28761 = ORIENTED_EDGE ( 'NONE', *, *, #24260, .T. ) ;
#28762 = CARTESIAN_POINT ( 'NONE',  ( 52.41226287506260917, 8.644902628253648302, 2.049999999999817302 ) ) ;
#28763 = CARTESIAN_POINT ( 'NONE',  ( -59.47085481156723574, 2.489203624310591945, -2.804704140674918911 ) ) ;
#28765 = CARTESIAN_POINT ( 'NONE',  ( 51.30671737785521458, -3.991926107141777980, -1.294864543654180133 ) ) ;
#28764 = FACE_OUTER_BOUND ( 'NONE', #25968, .T. ) ;
#28766 = ORIENTED_EDGE ( 'NONE', *, *, #22832, .T. ) ;
#28767 = VERTEX_POINT ( 'NONE', #2021 ) ;
#28768 = ORIENTED_EDGE ( 'NONE', *, *, #30372, .F. ) ;
#28769 = DIRECTION ( 'NONE',  ( -1.000000000000000000, -2.586136946169074517E-16, 0.000000000000000000 ) ) ;
#28770 = EDGE_CURVE ( 'NONE', #18491, #6711, #22672, .T. ) ;
#28771 = VERTEX_POINT ( 'NONE', #30841 ) ;
#28772 = CARTESIAN_POINT ( 'NONE',  ( 50.36079629521400847, 1.278211010209494347, 3.870212229389975889 ) ) ;
#28773 = ORIENTED_EDGE ( 'NONE', *, *, #18901, .F. ) ;
#28774 = CARTESIAN_POINT ( 'NONE',  ( 56.99229187639506478, -0.7794873559220516501, 1.732743334125896428 ) ) ;
#28775 = CARTESIAN_POINT ( 'NONE',  ( 57.03643325641707662, 0.7481242503215885797, 1.780024810282529790 ) ) ;
#28776 = CARTESIAN_POINT ( 'NONE',  ( 47.12246479398822885, -4.133513435957373083, 2.021478398489655159 ) ) ;
#28777 = DIRECTION ( 'NONE',  ( 1.000000000000000000, -1.219044193948983948E-29, 3.491481338843133355E-15 ) ) ;
#28778 = CARTESIAN_POINT ( 'NONE',  ( -60.63452994616204705, -3.117691453623976816, 1.799999999999772671 ) ) ;
#28779 = ADVANCED_FACE ( 'NONE', ( #7096 ), #16279, .F. ) ;
#28780 = CARTESIAN_POINT ( 'NONE',  ( -59.13880064263039316, -2.480191926443811479, -0.9536590270807077108 ) ) ;
#28781 = TOROIDAL_SURFACE ( 'NONE', #27252, 4.279289321881344144, 0.05000000000000000278 ) ;
#28782 = DIRECTION ( 'NONE',  ( -1.000000000000000000, 0.000000000000000000, 0.000000000000000000 ) ) ;
#28783 = DIRECTION ( 'NONE',  ( -3.491481338843133355E-15, -3.613946018757868503E-15, 1.000000000000000000 ) ) ;
#28784 = SURFACE_STYLE_FILL_AREA ( #4700 ) ;
#28785 = EDGE_CURVE ( 'NONE', #2006, #30563, #4698, .T. ) ;
#28786 = CARTESIAN_POINT ( 'NONE',  ( -36.14490256869205353, -1.093737229520479470, 5.295968199484772931 ) ) ;
#28787 = EDGE_CURVE ( 'NONE', #3208, #29340, #390, .T. ) ;
#28788 = AXIS2_PLACEMENT_3D ( 'NONE', #16241, #8942, #25565 ) ;
#28789 = ORIENTED_EDGE ( 'NONE', *, *, #5935, .T. ) ;
#28790 = EDGE_CURVE ( 'NONE', #9864, #14055, #11836, .T. ) ;
#28791 = DIRECTION ( 'NONE',  ( -1.000000000000000000, -3.054025858079668409E-16, 2.042474015755241579E-16 ) ) ;
#28792 = CARTESIAN_POINT ( 'NONE',  ( -54.47366401599046526, 1.505709097230404359, 3.303769268891089794 ) ) ;
#28793 = CARTESIAN_POINT ( 'NONE',  ( 53.94287803706861695, 6.382080985259960038, -1.484311132272649436 ) ) ;
#28794 = ORIENTED_EDGE ( 'NONE', *, *, #12620, .T. ) ;
#28795 = CARTESIAN_POINT ( 'NONE',  ( -54.49999999999997868, 1.549999999999999600, 4.064480286580312907 ) ) ;
#28796 = VERTEX_POINT ( 'NONE', #16426 ) ;
#28797 = CARTESIAN_POINT ( 'NONE',  ( 15.49676243306307732, 0.05686983728432184332, -5.199999998843000348 ) ) ;
#28799 = DIRECTION ( 'NONE',  ( 0.000000000000000000, 0.000000000000000000, -1.000000000000000000 ) ) ;
#28798 = CARTESIAN_POINT ( 'NONE',  ( 58.72200624034153549, 0.9564954546397702595, -1.612834625125357135 ) ) ;
#28800 = VERTEX_POINT ( 'NONE', #2331 ) ;
#28801 = ORIENTED_EDGE ( 'NONE', *, *, #15021, .F. ) ;
#28802 = DIRECTION ( 'NONE',  ( 2.150099724758698120E-15, 0.05332224631949595423, -0.9985773570672645816 ) ) ;
#28803 = PRESENTATION_LAYER_ASSIGNMENT (  '', '', ( #24744 ) ) ;
#28804 = AXIS2_PLACEMENT_3D ( 'NONE', #2844, #9989, #7609 ) ;
#28805 = CARTESIAN_POINT ( 'NONE',  ( -69.19999999999998863, -0.4218824419643717460, 2.057186234924341939 ) ) ;
#28807 = DIRECTION ( 'NONE',  ( 1.000000000000000000, 0.000000000000000000, 0.000000000000000000 ) ) ;
#28806 = DIRECTION ( 'NONE',  ( 0.000000000000000000, 0.000000000000000000, 1.000000000000000000 ) ) ;
#28808 = ORIENTED_EDGE ( 'NONE', *, *, #14964, .T. ) ;
#28809 = CARTESIAN_POINT ( 'NONE',  ( -56.18749999999997158, 0.8699069336946689823, -4.241846523238429256 ) ) ;
#28810 = CARTESIAN_POINT ( 'NONE',  ( 61.25000000000001421, 0.9885922787763641306, 1.658880815146376753 ) ) ;
#28811 = DIRECTION ( 'NONE',  ( -1.168655815394902336E-14, 0.000000000000000000, -1.000000000000000000 ) ) ;
#28812 = CARTESIAN_POINT ( 'NONE',  ( -62.04999999999998295, -2.737158043526071172, 0.2654540351181890467 ) ) ;
#28813 = CARTESIAN_POINT ( 'NONE',  ( 50.55258015808398397, 5.293720379222080095E-13, -1.177580158083963546 ) ) ;
#28814 = CARTESIAN_POINT ( 'NONE',  ( -58.06249999999996447, 3.400000000000007905, -1.844164440896605116E-13 ) ) ;
#28815 = FACE_OUTER_BOUND ( 'NONE', #3005, .T. ) ;
#28816 = EDGE_CURVE ( 'NONE', #7825, #76, #20635, .T. ) ;
#28817 = ORIENTED_EDGE ( 'NONE', *, *, #10252, .T. ) ;
#28818 = DIRECTION ( 'NONE',  ( 1.000000000000000000, 0.000000000000000000, -1.047444401652940007E-14 ) ) ;
#28819 = EDGE_CURVE ( 'NONE', #26590, #9481, #19619, .T. ) ;
#28820 = DIRECTION ( 'NONE',  ( 0.000000000000000000, 0.000000000000000000, -1.000000000000000000 ) ) ;
#28821 = CARTESIAN_POINT ( 'NONE',  ( 57.05000000000001847, -0.8000000000000000444, 2.471260002560650371 ) ) ;
#28822 = DIRECTION ( 'NONE',  ( 1.000000000000000000, 1.047444401652940007E-14, 0.000000000000000000 ) ) ;
#28823 = LINE ( 'NONE', #14394, #10965 ) ;
#28824 = VECTOR ( 'NONE', #8677, 1000.000000000000114 ) ;
#28825 = AXIS2_PLACEMENT_3D ( 'NONE', #8392, #28186, #22969 ) ;
#28827 = DIRECTION ( 'NONE',  ( 1.000000000000000000, 2.586136946169074517E-16, -0.000000000000000000 ) ) ;
#28826 = CARTESIAN_POINT ( 'NONE',  ( -59.09665968485343512, 2.466443774698494629, -0.9691001528487590555 ) ) ;
#28829 = CIRCLE ( 'NONE', #2531, 4.650000000000000355 ) ;
#28828 = CARTESIAN_POINT ( 'NONE',  ( 47.10000000000000853, -4.020776289669854009, -2.234582293948742748 ) ) ;
#28831 = FACE_OUTER_BOUND ( 'NONE', #16437, .T. ) ;
#28830 = CARTESIAN_POINT ( 'NONE',  ( 63.50000000000000000, 1.401298464324817071E-42, -2.375000000000663913 ) ) ;
#28832 = ORIENTED_EDGE ( 'NONE', *, *, #20337, .F. ) ;
#28833 = CARTESIAN_POINT ( 'NONE',  ( 58.75000000694010538, -1.869674713775759223, 0.4751516942898563745 ) ) ;
#28834 = UNCERTAINTY_MEASURE_WITH_UNIT (LENGTH_MEASURE( 1.000000000000000082E-05 ), #1294, 'distance_accuracy_value', 'NONE');
#28835 = CARTESIAN_POINT ( 'NONE',  ( 50.50000000000002132, -0.6462379109120509613, 4.048750000000023164 ) ) ;
#28836 = CARTESIAN_POINT ( 'NONE',  ( -36.48174642953026137, 5.256245472275701047, 1.286369972357462199 ) ) ;
#28837 = CARTESIAN_POINT ( 'NONE',  ( 15.29449157529473702, -4.822464347458966571, 1.985534350301629392 ) ) ;
#28838 = ORIENTED_EDGE ( 'NONE', *, *, #25445, .F. ) ;
#28839 = ORIENTED_EDGE ( 'NONE', *, *, #23367, .F. ) ;
#28840 = CARTESIAN_POINT ( 'NONE',  ( -57.65835481156722864, -0.7533615035078039535, 3.673546848079178861 ) ) ;
#28841 = ORIENTED_EDGE ( 'NONE', *, *, #25272, .F. ) ;
#28842 = CARTESIAN_POINT ( 'NONE',  ( 56.95000000000001705, 0.7137254901960785602, -2.500119182087999548 ) ) ;
#28843 = CARTESIAN_POINT ( 'NONE',  ( 69.25000000000000000, 0.7500000000000000000, -1.988246715074081905 ) ) ;
#28844 = VERTEX_POINT ( 'NONE', #25924 ) ;
#28845 = CARTESIAN_POINT ( 'NONE',  ( 58.73371041428907091, 1.873417296529001908, 0.08026432063284159868 ) ) ;
#28846 = ORIENTED_EDGE ( 'NONE', *, *, #13839, .T. ) ;
#28847 = CARTESIAN_POINT ( 'NONE',  ( -60.58155989232412253, -1.962990915244731571, 3.399999999999776534 ) ) ;
#28848 = EDGE_LOOP ( 'NONE', ( #7492, #210, #9099, #29336 ) ) ;
#28849 =( NAMED_UNIT ( * ) SI_UNIT ( $, .STERADIAN. ) SOLID_ANGLE_UNIT ( ) );
#28850 = ORIENTED_EDGE ( 'NONE', *, *, #4375, .T. ) ;
#28851 = EDGE_CURVE ( 'NONE', #15131, #4358, #15557, .T. ) ;
#28852 = VERTEX_POINT ( 'NONE', #19143 ) ;
#28853 = CIRCLE ( 'NONE', #4572, 2.000000000000000000 ) ;
#28854 = EDGE_CURVE ( 'NONE', #2938, #1198, #24178, .T. ) ;
#28855 = CARTESIAN_POINT ( 'NONE',  ( -54.69702994616206837, -2.078460969082657872, 3.599999999999797584 ) ) ;
#28856 = ADVANCED_FACE ( 'NONE', ( #9639 ), #17297, .T. ) ;
#28857 = CARTESIAN_POINT ( 'NONE',  ( 53.87894805006523313, 4.971284855691957993, -2.050000000000188116 ) ) ;
#28858 = DIRECTION ( 'NONE',  ( 0.000000000000000000, -0.8660422822663634834, -0.4999707644721521627 ) ) ;
#28859 = CARTESIAN_POINT ( 'NONE',  ( -44.59999999999998721, -1.400000000000004574, 3.363870538531272825 ) ) ;
#28860 = CARTESIAN_POINT ( 'NONE',  ( -60.61250724947091584, -2.452226114303401427, -1.129861533254596928 ) ) ;
#28861 =( BOUNDED_CURVE ( )  B_SPLINE_CURVE ( 2, ( #17917, #981, #20773, #12828, #6048, #22510, #20311, #15700, #25347 ),
 .UNSPECIFIED., .F., .T. ) 
 B_SPLINE_CURVE_WITH_KNOTS ( ( 3, 2, 2, 2, 3 ),
 ( 0.7011399156489748208, 0.7037037037037037202, 0.7222222222222222099, 0.7407407407407406996, 0.7424297805561814734 ),
 .UNSPECIFIED. ) 
 CURVE ( )  GEOMETRIC_REPRESENTATION_ITEM ( )  RATIONAL_B_SPLINE_CURVE ( ( 0.9680396472854365664, 0.9814519466516125057, 1.000000000000000000, 0.8660254037844387076, 1.000000000000000000, 0.8660254037844387076, 1.000000000000000000, 0.9877804249276531667, 0.9777898995284022288 ) ) 
 REPRESENTATION_ITEM ( '' )  );
#28863 = FACE_OUTER_BOUND ( 'NONE', #13174, .T. ) ;
#28862 = DIRECTION ( 'NONE',  ( 0.000000000000000000, 0.000000000000000000, 1.000000000000000000 ) ) ;
#28864 = CARTESIAN_POINT ( 'NONE',  ( 47.10000000000002984, -4.179189514726507682, 0.9999999999999997780 ) ) ;
#28865 = DIRECTION ( 'NONE',  ( 1.000000000000000000, 0.000000000000000000, -1.047444401652940007E-14 ) ) ;
#28867 = PLANE ( 'NONE',  #22590 ) ;
#28866 = CARTESIAN_POINT ( 'NONE',  ( 15.94709373951304343, 5.297368390263439863, -1.087079755157641880 ) ) ;
#28868 = ADVANCED_FACE ( 'NONE', ( #15140 ), #10521, .T. ) ;
#28869 = EDGE_LOOP ( 'NONE', ( #2287, #18610 ) ) ;
#28870 = DIRECTION ( 'NONE',  ( 1.000000000000000000, 0.000000000000000000, 0.000000000000000000 ) ) ;
#28871 = DIRECTION ( 'NONE',  ( 1.000000000000000000, -0.000000000000000000, -1.047444401652940007E-14 ) ) ;
#28873 = CARTESIAN_POINT ( 'NONE',  ( 50.33755732750837097, -1.426738769040649224, 3.843750315111184257 ) ) ;
#28872 = CARTESIAN_POINT ( 'NONE',  ( 48.40000000000002700, -0.6304760106459033064, 3.950000000000022826 ) ) ;
#28874 = CARTESIAN_POINT ( 'NONE',  ( 54.35699767715569664, 6.713389823568764569, -2.043118470513792140 ) ) ;
#28875 = DIRECTION ( 'NONE',  ( 1.000000000000000000, 2.586136946169074517E-16, -0.000000000000000000 ) ) ;
#28876 = CIRCLE ( 'NONE', #12667, 2.000000000000000000 ) ;
#28877 = ORIENTED_EDGE ( 'NONE', *, *, #10323, .F. ) ;
#28878 = DIRECTION ( 'NONE',  ( -3.491481338843133355E-15, 0.000000000000000000, -1.000000000000000000 ) ) ;
#28879 = CARTESIAN_POINT ( 'NONE',  ( -61.06249999999995737, 3.925981830489463142, -2.023818954174166834E-13 ) ) ;
#28880 = ORIENTED_EDGE ( 'NONE', *, *, #26055, .T. ) ;
#28881 = ORIENTED_EDGE ( 'NONE', *, *, #22364, .T. ) ;
#28882 = CARTESIAN_POINT ( 'NONE',  ( -59.49584459105846435, 3.403422474738959203, -1.120669429153365870 ) ) ;
#28883 = ORIENTED_EDGE ( 'NONE', *, *, #677, .F. ) ;
#28884 = CARTESIAN_POINT ( 'NONE',  ( 51.01608411450971658, 0.7569233679480915633, 1.030722644926825859 ) ) ;
#28885 = CARTESIAN_POINT ( 'NONE',  ( -57.88452994616205416, 3.117691453623979481, 1.799999999999806422 ) ) ;
#28886 = ORIENTED_EDGE ( 'NONE', *, *, #6324, .T. ) ;
#28887 = DIRECTION ( 'NONE',  ( 1.000000000000000000, 1.047444401652940007E-14, 0.000000000000000000 ) ) ;
#28888 = CARTESIAN_POINT ( 'NONE',  ( 51.36308620441100459, -1.097739233405182979, 1.198394850649636245 ) ) ;
#28889 = FACE_OUTER_BOUND ( 'NONE', #31279, .T. ) ;
#28890 = ORIENTED_EDGE ( 'NONE', *, *, #23612, .T. ) ;
#28891 = CIRCLE ( 'NONE', #29896, 0.1500000000000002720 ) ;
#28892 = EDGE_CURVE ( 'NONE', #2387, #23636, #19128, .T. ) ;
#28893 = CARTESIAN_POINT ( 'NONE',  ( -58.56249999999997868, -3.238593381231838819, -2.874284765127022023 ) ) ;
#28894 = CARTESIAN_POINT ( 'NONE',  ( 50.59602332238209499, -0.1408342061598471806, -0.8215393206232035617 ) ) ;
#28895 = EDGE_LOOP ( 'NONE', ( #16504, #25990, #13811, #18104 ) ) ;
#28896 = CARTESIAN_POINT ( 'NONE',  ( -60.89492752328840908, -2.547300119769525750, 0.9005536500125419508 ) ) ;
#28897 = CARTESIAN_POINT ( 'NONE',  ( -62.04999999999998295, -2.625757682666624238, -0.2804666419185135040 ) ) ;
#28899 = CARTESIAN_POINT ( 'NONE',  ( 58.74999981404334903, -0.9032433253524316807, 1.734728236458898287 ) ) ;
#28898 = SURFACE_STYLE_USAGE ( .BOTH. , #10345 ) ;
#28900 = CARTESIAN_POINT ( 'NONE',  ( 51.40674769956036272, 0.9873535814804794697, 1.422142864483640912 ) ) ;
#28901 = DIRECTION ( 'NONE',  ( 1.000000000000000000, 1.047444401652940007E-14, 0.000000000000000000 ) ) ;
#28902 = EDGE_CURVE ( 'NONE', #29235, #15307, #12516, .T. ) ;
#28903 = CARTESIAN_POINT ( 'NONE',  ( 61.25000000000004263, -1.470078920827180724, -1.470078920827526892 ) ) ;
#28904 = VERTEX_POINT ( 'NONE', #29084 ) ;
#28905 = ORIENTED_EDGE ( 'NONE', *, *, #4390, .F. ) ;
#28906 = AXIS2_PLACEMENT_3D ( 'NONE', #25560, #25257, #11159 ) ;
#28907 = CARTESIAN_POINT ( 'NONE',  ( -73.89999999999997726, -2.435524336289708093E-15, 4.607889071584891164E-15 ) ) ;
#28908 = EDGE_LOOP ( 'NONE', ( #14502, #12576, #29795, #18056 ) ) ;
#28909 = CARTESIAN_POINT ( 'NONE',  ( -35.85663232820584767, 3.817150320980676081, -2.203324261490498426 ) ) ;
#28910 = CARTESIAN_POINT ( 'NONE',  ( -60.47085481156722864, -3.673546848079176197, -0.7533615035078059519 ) ) ;
#28912 = DIRECTION ( 'NONE',  ( 1.000000000000000000, 0.000000000000000000, 0.000000000000000000 ) ) ;
#28911 = DIRECTION ( 'NONE',  ( 1.000000000000000000, 1.047444401652940007E-14, 0.000000000000000000 ) ) ;
#28913 = ORIENTED_EDGE ( 'NONE', *, *, #27593, .F. ) ;
#28914 = VERTEX_POINT ( 'NONE', #24191 ) ;
#28915 = CARTESIAN_POINT ( 'NONE',  ( -59.29999999999997584, -0.7533615035078030653, 3.673546848079178417 ) ) ;
#28916 = ORIENTED_EDGE ( 'NONE', *, *, #28851, .T. ) ;
#28917 = CARTESIAN_POINT ( 'NONE',  ( 33.47623932017462778, -5.377732432866642931, 0.5657657256215455899 ) ) ;
#28918 = ORIENTED_EDGE ( 'NONE', *, *, #29349, .T. ) ;
#28919 = CARTESIAN_POINT ( 'NONE',  ( -36.14490256869206064, 4.698781674909465522, 2.676750094560181203 ) ) ;
#28920 = EDGE_LOOP ( 'NONE', ( #8613, #26564, #3738, #20079 ) ) ;
#28921 = CARTESIAN_POINT ( 'NONE',  ( 56.95000000000001705, -0.6820512820512815155, 1.773360101234998210 ) ) ;
#28922 = DIRECTION ( 'NONE',  ( 1.282749433769087582E-30, 1.000000000000000000, 1.224646799147353207E-16 ) ) ;
#28923 = EDGE_CURVE ( 'NONE', #3746, #15927, #8993, .T. ) ;
#28924 = CARTESIAN_POINT ( 'NONE',  ( 51.13989201884550795, 0.9305404255935276758, -1.499649012356545796 ) ) ;
#28925 = CARTESIAN_POINT ( 'NONE',  ( -60.94702994616203995, 4.156921938165313080, -2.011299877933566609E-13 ) ) ;
#28926 = DIRECTION ( 'NONE',  ( -1.016952486242704214E-14, 0.000000000000000000, -1.000000000000000000 ) ) ;
#28927 = CIRCLE ( 'NONE', #19336, 2.764644660940665855 ) ;
#28928 = AXIS2_PLACEMENT_3D ( 'NONE', #532, #17474, #19560 ) ;
#28929 = DIRECTION ( 'NONE',  ( 0.000000000000000000, -1.000000000000000000, -1.224646799147352961E-16 ) ) ;
#28930 = CARTESIAN_POINT ( 'NONE',  ( -54.49999999999997868, -4.766731106216463600E-14, -1.834893917355220926E-13 ) ) ;
#28932 = ORIENTED_EDGE ( 'NONE', *, *, #29742, .F. ) ;
#28931 = EDGE_CURVE ( 'NONE', #9397, #17741, #30214, .T. ) ;
#28933 = CARTESIAN_POINT ( 'NONE',  ( -36.89831264271880684, 0.2888463313200247407, 5.401384060636566176 ) ) ;
#28934 = ADVANCED_BREP_SHAPE_REPRESENTATION ( '', ( #25849, #9018 ), #21749 ) ;
#28935 = ORIENTED_EDGE ( 'NONE', *, *, #17708, .F. ) ;
#28936 = CARTESIAN_POINT ( 'NONE',  ( -54.49999999999996447, 1.514093959731561467, -3.183260039818583298 ) ) ;
#28937 = CARTESIAN_POINT ( 'NONE',  ( -54.49865678108456279, 1.537045020190657585, 3.323865043138458208 ) ) ;
#28938 = CYLINDRICAL_SURFACE ( 'NONE', #30192, 0.1500000000000001887 ) ;
#28939 = ORIENTED_EDGE ( 'NONE', *, *, #27912, .T. ) ;
#28940 = CARTESIAN_POINT ( 'NONE',  ( -54.49409853110120139, 1.525884777627347644, 4.047834655405393889 ) ) ;
#28941 = ORIENTED_EDGE ( 'NONE', *, *, #7519, .F. ) ;
#28942 = CARTESIAN_POINT ( 'NONE',  ( 15.49702763512084047, -0.05469410396135043068, -5.200000001156997342 ) ) ;
#28944 = CARTESIAN_POINT ( 'NONE',  ( 47.28118949446516694, -3.793704335752947632, -1.557065711441589562 ) ) ;
#28943 = DIRECTION ( 'NONE',  ( 9.408669700213139918E-15, -1.000000000000000000, 0.000000000000000000 ) ) ;
#28945 = EDGE_CURVE ( 'NONE', #20971, #12243, #723, .T. ) ;
#28946 = VERTEX_POINT ( 'NONE', #17522 ) ;
#28947 = CARTESIAN_POINT ( 'NONE',  ( 50.59602332238209499, 0.1408342061609077767, -1.125000000000000222 ) ) ;
#28948 = CARTESIAN_POINT ( 'NONE',  ( 50.59602332238209499, 0.1408342061609076379, -0.8215393206232032286 ) ) ;
#28950 = CARTESIAN_POINT ( 'NONE',  ( 47.10000000000002274, 2.428612866367529932E-14, -1.644487710595116631E-13 ) ) ;
#28949 = CYLINDRICAL_SURFACE ( 'NONE', #16076, 2.000000000000000000 ) ;
#28951 = ORIENTED_EDGE ( 'NONE', *, *, #13531, .F. ) ;
#28952 = CARTESIAN_POINT ( 'NONE',  ( -56.43749999999997158, -4.108500314926507357, 1.367561758111406345 ) ) ;
#28953 = DIRECTION ( 'NONE',  ( -2.581436205204234499E-16, 0.9796124928211140670, 0.2008964009354147762 ) ) ;
#28954 = FACE_OUTER_BOUND ( 'NONE', #4451, .T. ) ;
#28955 = CARTESIAN_POINT ( 'NONE',  ( 16.08093158123429944, -2.941172302009019468, -4.539591111929662581 ) ) ;
#28956 = ADVANCED_FACE ( 'NONE', ( #5311 ), #10233, .F. ) ;
#28957 = CARTESIAN_POINT ( 'NONE',  ( -59.41132486540516311, 2.423250918913632201, 1.250136525132548027 ) ) ;
#28958 = DIRECTION ( 'NONE',  ( -1.000000000000000000, -3.053848253006669023E-16, 2.042510438544995169E-16 ) ) ;
#28959 = EDGE_CURVE ( 'NONE', #24355, #26303, #24797, .T. ) ;
#28961 = DIRECTION ( 'NONE',  ( 1.000000000000000000, 0.000000000000000000, 0.000000000000000000 ) ) ;
#28960 = AXIS2_PLACEMENT_3D ( 'NONE', #19108, #28755, #7068 ) ;
#28962 = ADVANCED_FACE ( 'NONE', ( #3106 ), #29041, .T. ) ;
#28963 = ORIENTED_EDGE ( 'NONE', *, *, #12188, .F. ) ;
#28964 = FACE_OUTER_BOUND ( 'NONE', #16431, .T. ) ;
#28965 = CARTESIAN_POINT ( 'NONE',  ( 15.56274145962646926, -3.953287617511611174, 3.694739123711129558 ) ) ;
#28966 = CARTESIAN_POINT ( 'NONE',  ( 48.39188949082539182, 1.340787288841451819, -3.874691554877328414 ) ) ;
#28967 = B_SPLINE_CURVE_WITH_KNOTS ( 'NONE', 3,
 ( #31189, #19475, #17112, #29423 ),
 .UNSPECIFIED., .F., .F.,
 ( 4, 4 ),
 ( 0.000000000000000000, 0.0003113238203258932740 ),
 .UNSPECIFIED. ) ;
#28968 = CARTESIAN_POINT ( 'NONE',  ( 25.89592582029650103, 5.217927461809758860, -1.950000000000090328 ) ) ;
#28969 = CARTESIAN_POINT ( 'NONE',  ( -62.06682860016772452, -2.653360696315357092, 0.1987474702245471680 ) ) ;
#28970 = ADVANCED_FACE ( 'NONE', ( #24485 ), #5496, .T. ) ;
#28972 = CARTESIAN_POINT ( 'NONE',  ( 53.06648468529573393, 8.205141401880769791, -1.913421085928479259 ) ) ;
#28971 = CARTESIAN_POINT ( 'NONE',  ( 58.65000000000000568, 1.253243060177670287, 1.394635017528978782 ) ) ;
#28974 = LINE ( 'NONE', #24381, #1848 ) ;
#28973 = DIRECTION ( 'NONE',  ( -0.9993908270191184107, 0.03489949670185085034, 3.491481338843133355E-15 ) ) ;
#28975 = ORIENTED_EDGE ( 'NONE', *, *, #15447, .T. ) ;
#28976 = DIRECTION ( 'NONE',  ( 1.000000000000000000, 1.047444401652940007E-14, 0.000000000000000000 ) ) ;
#28977 = CYLINDRICAL_SURFACE ( 'NONE', #8518, 3.399999999999999911 ) ;
#28978 = AXIS2_PLACEMENT_3D ( 'NONE', #14325, #29217, #7531 ) ;
#28980 = CARTESIAN_POINT ( 'NONE',  ( -36.77443515226919857, 4.926689578693665972, 2.233438676318016292 ) ) ;
#28979 = CARTESIAN_POINT ( 'NONE',  ( -44.59999999999995879, 1.500000000000023981, -4.029888335922147569 ) ) ;
#28981 = DIRECTION ( 'NONE',  ( 1.000000000000000000, 0.000000000000000000, 0.000000000000000000 ) ) ;
#28982 = EDGE_CURVE ( 'NONE', #23193, #207, #22939, .T. ) ;
#28983 = ORIENTED_EDGE ( 'NONE', *, *, #28039, .T. ) ;
#28984 = ORIENTED_EDGE ( 'NONE', *, *, #29379, .T. ) ;
#28985 = CARTESIAN_POINT ( 'NONE',  ( 22.07280086217093640, 8.086143481909148889, -2.050000000000076650 ) ) ;
#28986 = B_SPLINE_CURVE_WITH_KNOTS ( 'NONE', 3,
 ( #28027, #30889, #16477, #16001, #4446, #14096, #13611, #1271, #11096, #20776, #30402, #25662, #3971, #23301, #11243, #30553 ),
 .UNSPECIFIED., .F., .F.,
 ( 4, 3, 3, 3, 3, 4 ),
 ( 0.000000000000000000, 2.177138635050367827E-05, 4.299041441261427111E-05, 6.255873377259018090E-05, 8.005453962339759144E-05, 9.359446731969179928E-05 ),
 .UNSPECIFIED. ) ;
#28987 = ORIENTED_EDGE ( 'NONE', *, *, #6615, .T. ) ;
#28988 = EDGE_CURVE ( 'NONE', #17666, #7967, #7406, .T. ) ;
#28989 = DIRECTION ( 'NONE',  ( 1.000000000000000000, 1.047444401652940007E-14, 0.000000000000000000 ) ) ;
#28990 = B_SPLINE_CURVE_WITH_KNOTS ( 'NONE', 3,
 ( #20316, #15074, #7640, #15549 ),
 .UNSPECIFIED., .F., .F.,
 ( 4, 4 ),
 ( 0.000000000000000000, 0.0002183616642542151958 ),
 .UNSPECIFIED. ) ;
#28991 = CARTESIAN_POINT ( 'NONE',  ( 51.14630318392405428, 0.9364487020640391846, 1.503522130792586342 ) ) ;
#28992 = ORIENTED_EDGE ( 'NONE', *, *, #6721, .T. ) ;
#28993 = CARTESIAN_POINT ( 'NONE',  ( -36.48174642952978530, -5.256245472275803188, -1.286369972357330749 ) ) ;
#28994 = ORIENTED_EDGE ( 'NONE', *, *, #16643, .T. ) ;
#28995 = FILL_AREA_STYLE ('',( #14113 ) ) ;
#28996 = FACE_OUTER_BOUND ( 'NONE', #25037, .T. ) ;
#28997 =( NAMED_UNIT ( * ) SI_UNIT ( $, .STERADIAN. ) SOLID_ANGLE_UNIT ( ) );
#28998 = ORIENTED_EDGE ( 'NONE', *, *, #22253, .F. ) ;
#28999 = EDGE_CURVE ( 'NONE', #11630, #10988, #10240, .T. ) ;
#29000 = ADVANCED_FACE ( 'NONE', ( #22295 ), #20550, .T. ) ;
#29001 = ORIENTED_EDGE ( 'NONE', *, *, #18671, .T. ) ;
#29002 = CARTESIAN_POINT ( 'NONE',  ( -56.44702994616204705, 4.156921938165313080, -1.854183217685626176E-13 ) ) ;
#29003 = CARTESIAN_POINT ( 'NONE',  ( -67.97846802697301882, 0.6530782982312793861, -3.184545152421069947 ) ) ;
#29004 = DIRECTION ( 'NONE',  ( 0.000000000000000000, 0.000000000000000000, 1.000000000000000000 ) ) ;
#29005 = AXIS2_PLACEMENT_3D ( 'NONE', #30256, #18245, #25969 ) ;
#29006 = CIRCLE ( 'NONE', #31014, 0.1500000000000001887 ) ;
#29007 = DIRECTION ( 'NONE',  ( 1.000000000000000000, 1.047444401652940007E-14, 0.000000000000000000 ) ) ;
#29009 = CARTESIAN_POINT ( 'NONE',  ( -36.48821680285183788, 0.3995010896672961942, -5.397102918580238828 ) ) ;
#29008 = DIRECTION ( 'NONE',  ( 2.463111065593883491E-12, 0.2069455031824437852, -0.9783524716136640098 ) ) ;
#29010 = PLANE ( 'NONE',  #4888 ) ;
#29011 = CARTESIAN_POINT ( 'NONE',  ( -54.49999999999997868, 8.366749974758489177E-15, -2.216533082070116467E-13 ) ) ;
#29013 = CARTESIAN_POINT ( 'NONE',  ( 58.75000000000004263, -2.079005547593188119, 1.932245437381540134E-15 ) ) ;
#29012 = CARTESIAN_POINT ( 'NONE',  ( 54.49932581792542408, -0.002837702348961988318, -4.287546236934917765 ) ) ;
#29014 = EDGE_LOOP ( 'NONE', ( #30698, #3416, #2440, #5262, #15082, #17890 ) ) ;
#29015 = CARTESIAN_POINT ( 'NONE',  ( -61.34999999999997300, -2.581364933566181019, -0.7915523228156536861 ) ) ;
#29016 =( REPRESENTATION_RELATIONSHIP ('NONE','NONE', #7047, #15725 ) REPRESENTATION_RELATIONSHIP_WITH_TRANSFORMATION ( #26428 )SHAPE_REPRESENTATION_RELATIONSHIP( ) );
#29017 = CARTESIAN_POINT ( 'NONE',  ( 51.72415272413284271, 3.851081239263533629, 1.414169555378673504 ) ) ;
#29019 = CARTESIAN_POINT ( 'NONE',  ( 48.43975240335598897, -1.282505688586073944, -3.869483523004607406 ) ) ;
#29018 = DIRECTION ( 'NONE',  ( 1.000000000000000000, -0.000000000000000000, -0.000000000000000000 ) ) ;
#29020 = CARTESIAN_POINT ( 'NONE',  ( -58.24999999999995737, 3.648081215184779629E-14, -3.400000000000207301 ) ) ;
#29021 = EDGE_CURVE ( 'NONE', #12582, #26840, #10861, .T. ) ;
#29022 = VERTEX_POINT ( 'NONE', #23338 ) ;
#29023 = FACE_OUTER_BOUND ( 'NONE', #24206, .T. ) ;
#29024 = EDGE_CURVE ( 'NONE', #28408, #16052, #21162, .T. ) ;
#29025 = ORIENTED_EDGE ( 'NONE', *, *, #27912, .F. ) ;
#29026 = EDGE_CURVE ( 'NONE', #4358, #4028, #27190, .T. ) ;
#29027 = AXIS2_PLACEMENT_3D ( 'NONE', #23159, #11103, #18398 ) ;
#29028 = CARTESIAN_POINT ( 'NONE',  ( 51.60188271988062070, -4.191430714671220414, 1.624095931900496836 ) ) ;
#29029 = CARTESIAN_POINT ( 'NONE',  ( -59.38452994616203995, 3.117691453623979481, 1.799999999999801092 ) ) ;
#29030 = ORIENTED_EDGE ( 'NONE', *, *, #27308, .T. ) ;
#29031 = EDGE_LOOP ( 'NONE', ( #26494, #12215, #3477, #17827, #180 ) ) ;
#29032 = CARTESIAN_POINT ( 'NONE',  ( -59.50593083503063951, 3.383800819141645100, -1.126492724825817415 ) ) ;
#29033 = ORIENTED_EDGE ( 'NONE', *, *, #21764, .T. ) ;
#29034 = CARTESIAN_POINT ( 'NONE',  ( 48.47372026270297596, -1.373706569044463199, 3.853361913240786141 ) ) ;
#29035 = CARTESIAN_POINT ( 'NONE',  ( -55.69702994616204705, 4.156921938165313080, -1.827997107644302771E-13 ) ) ;
#29036 = ORIENTED_EDGE ( 'NONE', *, *, #713, .T. ) ;
#29037 = CARTESIAN_POINT ( 'NONE',  ( 54.49860577577695864, -0.002682860454229076680, 4.292318283074051166 ) ) ;
#29038 = TOROIDAL_SURFACE ( 'NONE', #15368, 2.100674278852607824, 0.05000000000000000278 ) ;
#29039 = CARTESIAN_POINT ( 'NONE',  ( 30.98482657347519975, 7.184130539199036214, 1.949999999999890710 ) ) ;
#29040 = VERTEX_POINT ( 'NONE', #27485 ) ;
#29041 =( BOUNDED_SURFACE ( )  B_SPLINE_SURFACE ( 3, 2, ( 
 ( #26860, #19759, #26726 ),
 ( #8021, #14678, #5488 ),
 ( #14816, #12754, #21973 ),
 ( #20067, #263, #127 ),
 ( #432, #12294, #2795 ),
 ( #14826, #10392, #9937 ),
 ( #24804, #19616, #5649 ),
 ( #22438, #20077, #581 ),
 ( #5025, #27185, #9780 ),
 ( #3114, #21841, #27337 ),
 ( #29253, #24344, #10092 ),
 ( #19763, #26867, #733 ),
 ( #14984, #29714, #2505 ),
 ( #17081, #29394, #19446 ),
 ( #15302, #12451, #8029 ),
 ( #5177, #17534, #17694 ) ),
 .UNSPECIFIED., .F., .F., .F. ) 
 B_SPLINE_SURFACE_WITH_KNOTS ( ( 4, 2, 2, 2, 2, 2, 2, 4 ),
 ( 3, 3 ),
 ( 0.001780502285214259975, 0.002558945925323794120, 0.002753556835351177873, 0.002948167745378561192, 0.003337389565433328265, 0.003726611385488095337, 0.004115833205542862409, 0.004894276845652396554 ),
 ( 0.000000000000000000, 1.000000000000000000 ),
 .UNSPECIFIED. ) 
 GEOMETRIC_REPRESENTATION_ITEM ( )  RATIONAL_B_SPLINE_SURFACE ( (
 ( 1.000000000000000000, 0.9418517008537217183, 1.000000000000000000),
 ( 1.000000000000000000, 0.9417987965885166179, 1.000000000000000000),
 ( 1.000000000000000000, 0.9418198861733918514, 1.000000000000000000),
 ( 1.000000000000000000, 0.9434060303845587248, 1.000000000000000000),
 ( 1.000000000000000000, 0.9437939819948625297, 1.000000000000000000),
 ( 1.000000000000000000, 0.9445989566712326146, 1.000000000000000000),
 ( 1.000000000000000000, 0.9450169930050459355, 1.000000000000000000),
 ( 1.000000000000000000, 0.9461610507672288950, 1.000000000000000000),
 ( 1.000000000000000000, 0.9467217966428351783, 1.000000000000000000),
 ( 1.000000000000000000, 0.9467345476123190107, 1.000000000000000000),
 ( 1.000000000000000000, 0.9461964028051400577, 1.000000000000000000),
 ( 1.000000000000000000, 0.9446801822475351385, 1.000000000000000000),
 ( 1.000000000000000000, 0.9437582546536535943, 1.000000000000000000),
 ( 1.000000000000000000, 0.9418129560295680491, 1.000000000000000000),
 ( 1.000000000000000000, 0.9418016889777458545, 1.000000000000000000),
 ( 1.000000000000000000, 0.9418517008537214963, 1.000000000000000000) ) ) 
 REPRESENTATION_ITEM ( '' )  SURFACE ( )  );
#29042 = DIRECTION ( 'NONE',  ( 0.000000000000000000, -0.2745098039215694841, 0.9615843008030765526 ) ) ;
#29043 = CARTESIAN_POINT ( 'NONE',  ( 54.21707933481621922, 5.861459378068796688, -2.050000000000189004 ) ) ;
#29044 = CARTESIAN_POINT ( 'NONE',  ( 58.73371041428920591, -0.8671977075792437484, -1.662559130998595203 ) ) ;
#29045 = CARTESIAN_POINT ( 'NONE',  ( -59.61589511801003738, 3.087468777912107942, -1.452347209873861456 ) ) ;
#29046 = CARTESIAN_POINT ( 'NONE',  ( 34.55000000000001847, 0.000000000000000000, 0.000000000000000000 ) ) ;
#29047 = CIRCLE ( 'NONE', #15383, 0.1000000000000000472 ) ;
#29049 = CYLINDRICAL_SURFACE ( 'NONE', #245, 0.2500000000000000000 ) ;
#29048 = CARTESIAN_POINT ( 'NONE',  ( 57.05000000000001847, -0.8000000000000000444, 1.778341924377873751 ) ) ;
#29050 = CIRCLE ( 'NONE', #13328, 3.075000000000000622 ) ;
#29051 = B_SPLINE_CURVE_WITH_KNOTS ( 'NONE', 3,
 ( #28723, #9574, #11617, #26336, #14447, #6702, #29019, #17002, #26653, #11454, #28549, #9082, #19232, #21770 ),
 .UNSPECIFIED., .F., .F.,
 ( 4, 2, 2, 2, 2, 2, 4 ),
 ( 0.000000000000000000, 0.0003953907277084696219, 0.0005930860915627040805, 0.0006919337734898216080, 0.0007413576144533806428, 0.0007660695349351558233, 0.0007907814554169310039 ),
 .UNSPECIFIED. ) ;
#29052 = CARTESIAN_POINT ( 'NONE',  ( 51.44193764627932808, 0.9752197701250188144, 1.304631266258923006 ) ) ;
#29053 = CARTESIAN_POINT ( 'NONE',  ( 36.50000000000002132, 0.8000000000000000444, 1.778341924377873751 ) ) ;
#29054 = DIRECTION ( 'NONE',  ( 0.000000000000000000, -0.2008964009354162750, 0.9796124928211136229 ) ) ;
#29055 = AXIS2_PLACEMENT_3D ( 'NONE', #22003, #7729, #17391 ) ;
#29056 = VERTEX_POINT ( 'NONE', #4162 ) ;
#29057 = EDGE_CURVE ( 'NONE', #1093, #3490, #2921, .T. ) ;
#29058 = ORIENTED_EDGE ( 'NONE', *, *, #9608, .T. ) ;
#29059 = CARTESIAN_POINT ( 'NONE',  ( 58.70142274306336105, 0.5000000000006148415, -1.816042500834985196 ) ) ;
#29060 = ORIENTED_EDGE ( 'NONE', *, *, #3676, .F. ) ;
#29061 = EDGE_CURVE ( 'NONE', #29835, #23193, #11453, .T. ) ;
#29062 = DIRECTION ( 'NONE',  ( 0.000000000000000000, 0.000000000000000000, -1.000000000000000000 ) ) ;
#29063 = CARTESIAN_POINT ( 'NONE',  ( -56.17292740578360366, -3.330682475591782765, -0.6830477631804111605 ) ) ;
#29065 = CARTESIAN_POINT ( 'NONE',  ( 50.25000000000000000, 2.008165151418512373, 0.5380862305919300592 ) ) ;
#29064 = FACE_OUTER_BOUND ( 'NONE', #19833, .T. ) ;
#29066 = ORIENTED_EDGE ( 'NONE', *, *, #29487, .F. ) ;
#29067 = EDGE_LOOP ( 'NONE', ( #29983, #4033, #27161, #21309, #14275, #13175 ) ) ;
#29068 = AXIS2_PLACEMENT_3D ( 'NONE', #23696, #16565, #23845 ) ;
#29069 = CARTESIAN_POINT ( 'NONE',  ( 61.00000000000001421, 0.8666666666673054076, -1.374595900215364930 ) ) ;
#29070 = VERTEX_POINT ( 'NONE', #4013 ) ;
#29071 = CARTESIAN_POINT ( 'NONE',  ( 31.30720621464603326, 7.411182539856416618, 1.949999999999890488 ) ) ;
#29072 = ORIENTED_EDGE ( 'NONE', *, *, #13067, .T. ) ;
#29073 = CARTESIAN_POINT ( 'NONE',  ( 50.36610310744725183, 1.399562922973069057, 3.853849143137397792 ) ) ;
#29074 = ORIENTED_EDGE ( 'NONE', *, *, #23966, .F. ) ;
#29075 = VECTOR ( 'NONE', #20557, 1000.000000000000000 ) ;
#29076 = CARTESIAN_POINT ( 'NONE',  ( 53.91574522235882228, 6.672251602522421443, 1.774295301432037286 ) ) ;
#29077 = FACE_OUTER_BOUND ( 'NONE', #12067, .T. ) ;
#29078 = EDGE_CURVE ( 'NONE', #11667, #826, #1956, .T. ) ;
#29079 = CARTESIAN_POINT ( 'NONE',  ( 56.99229187639506478, 0.7794873559220516501, -1.732743334125896428 ) ) ;
#29080 = AXIS2_PLACEMENT_3D ( 'NONE', #30266, #16335, #7006 ) ;
#29081 = CARTESIAN_POINT ( 'NONE',  ( -54.64405989232413674, -3.920666489018357767E-15, 3.399999999999804512 ) ) ;
#29082 = CARTESIAN_POINT ( 'NONE',  ( 52.45567523936517773, 8.517307475678894235, -2.050000000000181899 ) ) ;
#29083 = CARTESIAN_POINT ( 'NONE',  ( -58.77900635094606940, 3.400000000000002132, 0.9110272542656305816 ) ) ;
#29084 = CARTESIAN_POINT ( 'NONE',  ( 54.28867365409859502, 5.640057820322912363, -1.950000000000180256 ) ) ;
#29085 = CIRCLE ( 'NONE', #26049, 0.04999999999999991257 ) ;
#29086 = CARTESIAN_POINT ( 'NONE',  ( 58.75000000000002842, -0.8948927608030052827, -1.760622601996601366 ) ) ;
#29087 = CARTESIAN_POINT ( 'NONE',  ( 51.80000000000001137, 6.475000000000062705, -1.950000000000180256 ) ) ;
#29088 = EDGE_LOOP ( 'NONE', ( #8215, #13017, #25863, #3976 ) ) ;
#29089 = DIRECTION ( 'NONE',  ( 0.09218405009836744268, -0.9957419851083220141, -9.170184867090491304E-13 ) ) ;
#29091 = CARTESIAN_POINT ( 'NONE',  ( -59.69818608288214534, -2.432011272524986278, -1.237491343926018006 ) ) ;
#29090 = CARTESIAN_POINT ( 'NONE',  ( 61.16862972101695561, -0.7079877303042131365, 1.871978752394868550 ) ) ;
#29092 = CARTESIAN_POINT ( 'NONE',  ( 54.02708675723533105, 5.727819401067892890, 2.034055266290029085 ) ) ;
#29093 = AXIS2_PLACEMENT_3D ( 'NONE', #18162, #12901, #1187 ) ;
#29094 = ORIENTED_EDGE ( 'NONE', *, *, #3069, .F. ) ;
#29095 = ADVANCED_FACE ( 'NONE', ( #5978 ), #12915, .T. ) ;
#29096 = CARTESIAN_POINT ( 'NONE',  ( -36.92398358572909700, -5.231589534716087009, 1.397536681175191475 ) ) ;
#29097 = ORIENTED_EDGE ( 'NONE', *, *, #10728, .T. ) ;
#29098 = CIRCLE ( 'NONE', #27570, 0.09999999999999963085 ) ;
#29099 = CARTESIAN_POINT ( 'NONE',  ( 15.03925126672126034, 0.7747498368337761843, -5.363501452440937456 ) ) ;
#29100 = CARTESIAN_POINT ( 'NONE',  ( -36.56242893520637693, -5.074157625981839281, 1.874066637979944883 ) ) ;
#29102 = PLANE ( 'NONE',  #30831 ) ;
#29101 = CARTESIAN_POINT ( 'NONE',  ( -57.31249999999996447, 3.400000000000008349, -1.881930883448047941E-13 ) ) ;
#29103 = ORIENTED_EDGE ( 'NONE', *, *, #7527, .T. ) ;
#29104 = CARTESIAN_POINT ( 'NONE',  ( 52.20711756518982583, 0.7500000000005468959, -1.996089927833914146 ) ) ;
#29105 = DIRECTION ( 'NONE',  ( 0.000000000000000000, 1.000000000000000000, 0.000000000000000000 ) ) ;
#29107 = CARTESIAN_POINT ( 'NONE',  ( 47.10000000000002984, -4.020776289669855785, 2.234582293948414122 ) ) ;
#29106 = CARTESIAN_POINT ( 'NONE',  ( -58.58155989232410832, 3.400000000000007905, -1.908076882137507950E-13 ) ) ;
#29108 = ORIENTED_EDGE ( 'NONE', *, *, #13112, .T. ) ;
#29109 = CARTESIAN_POINT ( 'NONE',  ( -59.87499999999997158, 2.489203624310590168, -2.804704140674917134 ) ) ;
#29110 = DIRECTION ( 'NONE',  ( -1.000000000000000000, -0.000000000000000000, 3.491481338843133355E-15 ) ) ;
#29111 = DIRECTION ( 'NONE',  ( -1.000000000000000000, -3.053848253006669023E-16, 2.042510438544995415E-16 ) ) ;
#29112 = CIRCLE ( 'NONE', #19517, 4.279289321881344144 ) ;
#29113 = CARTESIAN_POINT ( 'NONE',  ( -55.24999999999996447, 2.107054635024525356E-14, -3.400000000000196643 ) ) ;
#29114 = CIRCLE ( 'NONE', #4829, 0.2500000000000000000 ) ;
#29115 = CARTESIAN_POINT ( 'NONE',  ( -54.87499999999997868, -3.673546848079173532, -0.7533615035078067290 ) ) ;
#29116 = CARTESIAN_POINT ( 'NONE',  ( -57.81249999999998579, -1.962990915244744228, 3.399999999999779643 ) ) ;
#29117 = PLANE ( 'NONE',  #1730 ) ;
#29118 = VECTOR ( 'NONE', #20845, 1000.000000000000000 ) ;
#29119 = ORIENTED_EDGE ( 'NONE', *, *, #28982, .T. ) ;
#29120 = AXIS2_PLACEMENT_3D ( 'NONE', #30430, #23471, #18891 ) ;
#29121 = CARTESIAN_POINT ( 'NONE',  ( 15.17214319754859098, -3.426725954212797465, 3.937891351789523320 ) ) ;
#29122 = CARTESIAN_POINT ( 'NONE',  ( 32.51063813751913045, 7.887597498970548848, -1.950000000000113864 ) ) ;
#29123 = EDGE_CURVE ( 'NONE', #1074, #28519, #25181, .T. ) ;
#29124 = CARTESIAN_POINT ( 'NONE',  ( -54.54999999999998295, 3.780972210569126836E-15, -5.448124817252668230E-16 ) ) ;
#29125 = DIRECTION ( 'NONE',  ( 0.000000000000000000, 0.000000000000000000, -1.000000000000000000 ) ) ;
#29126 = AXIS2_PLACEMENT_3D ( 'NONE', #24272, #14899, #7777 ) ;
#29127 = CARTESIAN_POINT ( 'NONE',  ( -35.85663232820584057, -0.4576450603546987628, 5.200000000000000178 ) ) ;
#29129 = CARTESIAN_POINT ( 'NONE',  ( 27.79265796670792099, 5.432811198890458826, 1.424999999999903011 ) ) ;
#29128 = CARTESIAN_POINT ( 'NONE',  ( 51.67649652704533736, -3.663955391962993247, 1.843087722223471392 ) ) ;
#29130 = AXIS2_PLACEMENT_3D ( 'NONE', #17145, #5873, #8241 ) ;
#29131 = ORIENTED_EDGE ( 'NONE', *, *, #13737, .F. ) ;
#29132 = EDGE_CURVE ( 'NONE', #7829, #11599, #21837, .T. ) ;
#29133 = DIRECTION ( 'NONE',  ( 0.000000000000000000, -0.000000000000000000, -1.000000000000000000 ) ) ;
#29134 = CIRCLE ( 'NONE', #21060, 0.05000000000000012768 ) ;
#29135 = ADVANCED_FACE ( 'NONE', ( #16053 ), #7493, .T. ) ;
#29137 = DIRECTION ( 'NONE',  ( 9.754918421198722508E-16, -0.9601771338024398528, 0.2793919678926571337 ) ) ;
#29136 = LINE ( 'NONE', #14576, #23687 ) ;
#29139 = EDGE_CURVE ( 'NONE', #8649, #22245, #28667, .T. ) ;
#29138 = DIRECTION ( 'NONE',  ( 0.000000000000000000, 0.000000000000000000, 1.000000000000000000 ) ) ;
#29140 = CONICAL_SURFACE ( 'NONE', #25603, 1.625000000000000444, 0.04363323129985093030 ) ;
#29141 = ORIENTED_EDGE ( 'NONE', *, *, #17238, .F. ) ;
#29142 = EDGE_LOOP ( 'NONE', ( #2099, #10326, #18919, #8783 ) ) ;
#29143 = CARTESIAN_POINT ( 'NONE',  ( 51.18284667156842715, -0.9660006958939171273, -1.457928575331213894 ) ) ;
#29144 = TOROIDAL_SURFACE ( 'NONE', #4340, 3.648039984012787063, 0.05000000000000000278 ) ;
#29145 = AXIS2_PLACEMENT_3D ( 'NONE', #28023, #15995, #25657 ) ;
#29146 = ORIENTED_EDGE ( 'NONE', *, *, #2080, .T. ) ;
#29147 = PRESENTATION_LAYER_ASSIGNMENT (  '', '', ( #23098 ) ) ;
#29148 = LINE ( 'NONE', #17133, #15527 ) ;
#29149 = VERTEX_POINT ( 'NONE', #18595 ) ;
#29150 = FACE_OUTER_BOUND ( 'NONE', #4201, .T. ) ;
#29151 = ORIENTED_EDGE ( 'NONE', *, *, #19481, .F. ) ;
#29152 = EDGE_CURVE ( 'NONE', #14189, #30539, #11535, .T. ) ;
#29153 = CARTESIAN_POINT ( 'NONE',  ( 58.74160516400037579, -1.390091577294200631, -1.258299259017775062 ) ) ;
#29154 = FILL_AREA_STYLE_COLOUR ( '', #29275 ) ;
#29156 = VERTEX_POINT ( 'NONE', #1058 ) ;
#29155 = CIRCLE ( 'NONE', #4379, 2.750000000000000444 ) ;
#29157 = AXIS2_PLACEMENT_3D ( 'NONE', #9355, #30731, #13919 ) ;
#29158 = EDGE_LOOP ( 'NONE', ( #13407, #26406, #29684 ) ) ;
#29159 = AXIS2_PLACEMENT_3D ( 'NONE', #5540, #29295, #3158 ) ;
#29160 = CARTESIAN_POINT ( 'NONE',  ( -56.38452994616205416, 3.117691453623979481, 1.799999999999811751 ) ) ;
#29161 = CIRCLE ( 'NONE', #24128, 0.01000000000000001929 ) ;
#29162 = CARTESIAN_POINT ( 'NONE',  ( 50.37722501620130799, 1.384253668070434484, 3.859284659399053741 ) ) ;
#29163 = SPHERICAL_SURFACE ( 'NONE', #5561, 0.05000000000000000278 ) ;
#29164 = CARTESIAN_POINT ( 'NONE',  ( -53.99999999999997868, 0.000000000000000000, 0.000000000000000000 ) ) ;
#29166 = EDGE_CURVE ( 'NONE', #26655, #15962, #11768, .T. ) ;
#29165 = CIRCLE ( 'NONE', #15511, 4.600000000000036948 ) ;
#29167 = FACE_OUTER_BOUND ( 'NONE', #12455, .T. ) ;
#29168 = CIRCLE ( 'NONE', #1857, 0.09999999999999999167 ) ;
#29169 = AXIS2_PLACEMENT_3D ( 'NONE', #25382, #1015, #3685 ) ;
#29171 = CARTESIAN_POINT ( 'NONE',  ( -36.48174642953001978, -0.4008586329626669387, -5.396496690166842747 ) ) ;
#29170 = CARTESIAN_POINT ( 'NONE',  ( 53.96125931204732495, 5.169815675097246377, -2.050000000000188116 ) ) ;
#29172 = CARTESIAN_POINT ( 'NONE',  ( -44.49999999999999289, 1.499999999999999556, 4.029888335921975262 ) ) ;
#29174 = DIRECTION ( 'NONE',  ( -3.696862594069201137E-15, 0.9356455129756980904, -0.3529411764705883137 ) ) ;
#29173 = DIRECTION ( 'NONE',  ( 1.000000000000000000, 1.047444401652940007E-14, 0.000000000000000000 ) ) ;
#29175 = EDGE_LOOP ( 'NONE', ( #10483, #13137, #11749, #12512 ) ) ;
#29176 = EDGE_CURVE ( 'NONE', #14207, #15114, #27137, .T. ) ;
#29177 = LINE ( 'NONE', #24119, #783 ) ;
#29178 = EDGE_CURVE ( 'NONE', #23320, #19132, #414, .T. ) ;
#29179 = DIRECTION ( 'NONE',  ( 0.000000000000000000, 0.3529411764705897014, -0.9356455129756974243 ) ) ;
#29180 = VECTOR ( 'NONE', #19809, 1000.000000000000000 ) ;
#29182 = DIRECTION ( 'NONE',  ( 1.000000000000000000, 1.047444401652940007E-14, 0.000000000000000000 ) ) ;
#29181 = DIRECTION ( 'NONE',  ( 0.000000000000000000, 0.000000000000000000, 1.000000000000000000 ) ) ;
#29184 = EDGE_CURVE ( 'NONE', #16975, #1787, #9398, .T. ) ;
#29183 = CARTESIAN_POINT ( 'NONE',  ( 47.12400915267975421, -4.149782173365510474, 1.728795876848494339 ) ) ;
#29185 = ORIENTED_EDGE ( 'NONE', *, *, #23484, .T. ) ;
#29186 = CARTESIAN_POINT ( 'NONE',  ( 58.50000000000001421, -0.8000000000000000444, 1.778341924377873751 ) ) ;
#29187 = CIRCLE ( 'NONE', #3399, 3.648039984012787507 ) ;
#29188 = ORIENTED_EDGE ( 'NONE', *, *, #10494, .T. ) ;
#29189 = CARTESIAN_POINT ( 'NONE',  ( 51.80000000000001847, -3.995252422878564857, 2.068710474281524991 ) ) ;
#29190 = ORIENTED_EDGE ( 'NONE', *, *, #5716, .F. ) ;
#29191 = ORIENTED_EDGE ( 'NONE', *, *, #11354, .T. ) ;
#29192 = CARTESIAN_POINT ( 'NONE',  ( 16.10667815269232150, 5.187083072802369799, -1.534568794951123083 ) ) ;
#29193 = EDGE_LOOP ( 'NONE', ( #8716, #29103, #22308, #6530 ) ) ;
#29194 = CARTESIAN_POINT ( 'NONE',  ( 58.65000000000000568, 1.320082690053779650, 1.469015551797190788 ) ) ;
#29195 = AXIS2_PLACEMENT_3D ( 'NONE', #25909, #11516, #21194 ) ;
#29196 = CARTESIAN_POINT ( 'NONE',  ( -55.25952994616203995, -3.117691453623963938, -1.800000000000207434 ) ) ;
#29197 = ORIENTED_EDGE ( 'NONE', *, *, #8505, .T. ) ;
#29198 = CARTESIAN_POINT ( 'NONE',  ( 54.50000000000002132, -0.003160834336558230456, 4.277587663180611344 ) ) ;
#29199 = AXIS2_PLACEMENT_3D ( 'NONE', #30881, #13755, #17691 ) ;
#29200 = AXIS2_PLACEMENT_3D ( 'NONE', #2092, #2417, #7172 ) ;
#29201 = CARTESIAN_POINT ( 'NONE',  ( -62.29999999999998295, -2.799131621120614977, -0.06972924524666890278 ) ) ;
#29202 = CARTESIAN_POINT ( 'NONE',  ( 30.73039768916305192, 7.037486599914624108, 1.949999999999957989 ) ) ;
#29203 = EDGE_LOOP ( 'NONE', ( #30739, #20212, #14136, #20075 ) ) ;
#29204 = FACE_OUTER_BOUND ( 'NONE', #3135, .T. ) ;
#29205 = CARTESIAN_POINT ( 'NONE',  ( 52.18343291569983222, 8.689381540779887558, -2.050000000000181455 ) ) ;
#29206 = AXIS2_PLACEMENT_3D ( 'NONE', #27671, #18335, #23243 ) ;
#29207 = EDGE_CURVE ( 'NONE', #7818, #19129, #26485, .T. ) ;
#29208 = CARTESIAN_POINT ( 'NONE',  ( 57.00000000000001421, -0.6999999999999999556, 2.452039967047845437 ) ) ;
#29209 = AXIS2_PLACEMENT_3D ( 'NONE', #22454, #13094, #19775 ) ;
#29210 = AXIS2_PLACEMENT_3D ( 'NONE', #28621, #1863, #11684 ) ;
#29211 = EDGE_CURVE ( 'NONE', #8262, #27197, #29234, .T. ) ;
#29213 = DIRECTION ( 'NONE',  ( 0.000000000000000000, 0.000000000000000000, 1.000000000000000000 ) ) ;
#29212 = CARTESIAN_POINT ( 'NONE',  ( -36.26369610968609436, -3.231775792180338502, 4.079530926931252743 ) ) ;
#29214 = FACE_OUTER_BOUND ( 'NONE', #10651, .T. ) ;
#29215 = FACE_BOUND ( 'NONE', #21308, .T. ) ;
#29216 = TOROIDAL_SURFACE ( 'NONE', #23170, 1.260000000000000009, 0.01000000000000000021 ) ;
#29217 = DIRECTION ( 'NONE',  ( 2.456447210758503401E-12, 0.9507508458638417315, -0.3099561728522108872 ) ) ;
#29218 = ORIENTED_EDGE ( 'NONE', *, *, #20261, .T. ) ;
#29219 = EDGE_CURVE ( 'NONE', #2736, #10297, #7929, .T. ) ;
#29220 = VERTEX_POINT ( 'NONE', #21607 ) ;
#29221 = ORIENTED_EDGE ( 'NONE', *, *, #111, .F. ) ;
#29222 = CARTESIAN_POINT ( 'NONE',  ( 52.98753545145217458, 8.419778228641124684, 2.049999999999815081 ) ) ;
#29223 = CARTESIAN_POINT ( 'NONE',  ( -60.65835481156722864, -0.8699069336946635422, 4.241846523238430144 ) ) ;
#29225 = FACE_OUTER_BOUND ( 'NONE', #25592, .T. ) ;
#29224 = DIRECTION ( 'NONE',  ( 0.000000000000000000, 0.000000000000000000, -1.000000000000000000 ) ) ;
#29226 = AXIS2_PLACEMENT_3D ( 'NONE', #2574, #493, #10011 ) ;
#29227 = ORIENTED_EDGE ( 'NONE', *, *, #18377, .F. ) ;
#29228 = ORIENTED_EDGE ( 'NONE', *, *, #2889, .T. ) ;
#29229 = FACE_OUTER_BOUND ( 'NONE', #29344, .T. ) ;
#29230 = VECTOR ( 'NONE', #16227, 1000.000000000000000 ) ;
#29231 = ORIENTED_EDGE ( 'NONE', *, *, #5186, .T. ) ;
#29232 = CARTESIAN_POINT ( 'NONE',  ( -57.22499999999997300, 2.964020293532818446E-15, 1.549317489258299684E-18 ) ) ;
#29233 =( BOUNDED_CURVE ( )  B_SPLINE_CURVE ( 3, ( #14604, #17150, #21911, #24269 ),
 .UNSPECIFIED., .F., .T. ) 
 B_SPLINE_CURVE_WITH_KNOTS ( ( 4, 4 ),
 ( 1.982313172862383732, 2.241731514487931509 ),
 .UNSPECIFIED. ) 
 CURVE ( )  GEOMETRIC_REPRESENTATION_ITEM ( )  RATIONAL_B_SPLINE_CURVE ( ( 1.000000000000000000, 0.9943997021150918769, 0.9943997021150918769, 1.000000000000000000 ) ) 
 REPRESENTATION_ITEM ( '' )  );
#29234 = CIRCLE ( 'NONE', #1926, 0.1500000000000000777 ) ;
#29235 = VERTEX_POINT ( 'NONE', #26335 ) ;
#29236 = CARTESIAN_POINT ( 'NONE',  ( 30.73039768916300218, 7.037486599914601015, -1.950000000000105871 ) ) ;
#29237 = ORIENTED_EDGE ( 'NONE', *, *, #18931, .T. ) ;
#29238 = CARTESIAN_POINT ( 'NONE',  ( 52.20711756518984714, -0.7499999999994533262, 1.718465885608438937 ) ) ;
#29239 = CARTESIAN_POINT ( 'NONE',  ( -59.09999999999997300, 8.366749974758448157E-15, -2.099585467500611340E-13 ) ) ;
#29240 = CARTESIAN_POINT ( 'NONE',  ( 65.00000000000001421, -1.025519176787267142E-28, -6.808388610744108654E-13 ) ) ;
#29241 = CARTESIAN_POINT ( 'NONE',  ( -56.08155989232413674, -1.962990915244731571, 3.399999999999792077 ) ) ;
#29242 = CARTESIAN_POINT ( 'NONE',  ( 52.48739568812349177, 8.621481665389278959, -2.050000000000182343 ) ) ;
#29243 = ADVANCED_FACE ( 'NONE', ( #4957 ), #19175, .T. ) ;
#29244 = EDGE_CURVE ( 'NONE', #4962, #30274, #18126, .T. ) ;
#29245 = EDGE_CURVE ( 'NONE', #12911, #8533, #5982, .T. ) ;
#29246 = CARTESIAN_POINT ( 'NONE',  ( 50.50000000000002132, 5.291762632692320630E-13, -1.996089927833914146 ) ) ;
#29247 = CARTESIAN_POINT ( 'NONE',  ( 51.70000000000002416, 2.428612866367529932E-14, -1.805095852181900386E-13 ) ) ;
#29248 = AXIS2_PLACEMENT_3D ( 'NONE', #23777, #16479, #23449 ) ;
#29249 = PLANE ( 'NONE',  #20544 ) ;
#29250 = DIRECTION ( 'NONE',  ( -1.000000000000000000, 0.000000000000000000, 3.491481338843132961E-15 ) ) ;
#29251 = VERTEX_POINT ( 'NONE', #12375 ) ;
#29252 = CARTESIAN_POINT ( 'NONE',  ( 61.25000000000002132, 6.415596960124259844E-13, 3.111507638930570854E-58 ) ) ;
#29253 = CARTESIAN_POINT ( 'NONE',  ( -36.89250464418453390, -2.917650619476045204, -4.554978966839832388 ) ) ;
#29254 = CARTESIAN_POINT ( 'NONE',  ( 54.10831690868383959, 6.369227351352716227, 2.033314590869161442 ) ) ;
#29255 = ORIENTED_EDGE ( 'NONE', *, *, #24314, .T. ) ;
#29256 = ADVANCED_FACE ( 'NONE', ( #29329 ), #727, .T. ) ;
#29257 = DIRECTION ( 'NONE',  ( 0.000000000000000000, -1.000000000000000000, -3.491481338843132961E-15 ) ) ;
#29258 = ORIENTED_EDGE ( 'NONE', *, *, #2208, .F. ) ;
#29259 = CARTESIAN_POINT ( 'NONE',  ( 15.57907767661750320, 0.5233326973447868236, -5.388419908789428447 ) ) ;
#29260 = CARTESIAN_POINT ( 'NONE',  ( 52.06628335902944826, 0.5434431642986583544, -1.996089927833914146 ) ) ;
#29261 = B_SPLINE_CURVE_WITH_KNOTS ( 'NONE', 3,
 ( #15905, #18303, #1647, #13216, #27944, #30799, #4188, #22899, #13360, #20837, #1346, #10845, #4041, #6260, #30625, #1506 ),
 .UNSPECIFIED., .F., .F.,
 ( 4, 2, 2, 2, 2, 2, 2, 4 ),
 ( 1.734723475976807094E-18, 0.0004351083927046436742, 0.0008702167854092856137, 0.001740433570818568625, 0.002175541963523209155, 0.002610650356227849252, 0.003045758748932490215, 0.003480867141637130312 ),
 .UNSPECIFIED. ) ;
#29263 = CARTESIAN_POINT ( 'NONE',  ( -62.06968758346935999, -2.680528337278641704, -0.3278885135174935961 ) ) ;
#29262 = DIRECTION ( 'NONE',  ( 0.000000000000000000, 0.000000000000000000, -1.000000000000000000 ) ) ;
#29264 = ORIENTED_EDGE ( 'NONE', *, *, #25507, .F. ) ;
#29265 = PLANE ( 'NONE',  #25989 ) ;
#29266 = B_SPLINE_CURVE_WITH_KNOTS ( 'NONE', 3,
 ( #3774, #13415, #11373, #28000, #6481, #6315, #2036 ),
 .UNSPECIFIED., .F., .F.,
 ( 4, 1, 1, 1, 4 ),
 ( 0.000000000000000000, 0.2499733219912199933, 0.4999822146608134954, 0.7499911073304068587, 1.000000000000000000 ),
 .UNSPECIFIED. ) ;
#29267 = CARTESIAN_POINT ( 'NONE',  ( -44.49999999999998579, -1.843099986694572142E-14, 0.000000000000000000 ) ) ;
#29269 = DIRECTION ( 'NONE',  ( 0.000000000000000000, 0.000000000000000000, -1.000000000000000000 ) ) ;
#29268 = CARTESIAN_POINT ( 'NONE',  ( 58.65000000000003411, -1.671477153793625714, -0.8495817349401489915 ) ) ;
#29270 = ORIENTED_EDGE ( 'NONE', *, *, #27474, .F. ) ;
#29271 = CARTESIAN_POINT ( 'NONE',  ( -58.43749999999997158, 0.8699069336946684272, -4.241846523238428368 ) ) ;
#29272 = CARTESIAN_POINT ( 'NONE',  ( -62.09999999999997300, -2.636465585633694264, 0.1493792525119592707 ) ) ;
#29273 = CARTESIAN_POINT ( 'NONE',  ( 58.75000000000000711, 1.469015551796267305, 1.320082690054878549 ) ) ;
#29274 = CARTESIAN_POINT ( 'NONE',  ( -55.09599364905385954, 3.400000000000011902, -0.9110272542659996198 ) ) ;
#29275 = COLOUR_RGB ( '', 0.31764706, 0.68627451, 0.89019608) ;
#29276 = AXIS2_PLACEMENT_3D ( 'NONE', #23486, #4014, #27771 ) ;
#29277 = CARTESIAN_POINT ( 'NONE',  ( -54.50000000000000000, -3.329534718049536046, -1.527735671238820148 ) ) ;
#29278 = CARTESIAN_POINT ( 'NONE',  ( 31.58270314793946909, 7.514175884156569118, -1.425000000000109956 ) ) ;
#29279 = PLANE ( 'NONE',  #24988 ) ;
#29280 = EDGE_LOOP ( 'NONE', ( #6524, #8872, #1289, #9655 ) ) ;
#29281 = EDGE_CURVE ( 'NONE', #3677, #4799, #11457, .T. ) ;
#29282 = DIRECTION ( 'NONE',  ( 0.000000000000000000, 0.9996898646859343485, 0.02490330187381116153 ) ) ;
#29283 = CARTESIAN_POINT ( 'NONE',  ( 25.58670780871698369, 5.245615029320309652, -1.950000000000087885 ) ) ;
#29284 = CARTESIAN_POINT ( 'NONE',  ( -54.49999999999997158, -3.430639028629426601, -0.8101486624347474796 ) ) ;
#29285 = CARTESIAN_POINT ( 'NONE',  ( -59.48573950359912743, 3.423031164920794289, -1.114835254188495162 ) ) ;
#29286 = DIRECTION ( 'NONE',  ( 1.000000000000000000, 3.054025858079668409E-16, -2.042474015755241579E-16 ) ) ;
#29288 = CARTESIAN_POINT ( 'NONE',  ( 25.71580480958625969, 5.235626398479815258, 1.424999999999910560 ) ) ;
#29287 = CARTESIAN_POINT ( 'NONE',  ( 51.70000000000001705, -3.609867133138429551, 1.947518732152937027 ) ) ;
#29289 = ORIENTED_EDGE ( 'NONE', *, *, #5434, .F. ) ;
#29290 = VECTOR ( 'NONE', #21409, 1000.000000000000000 ) ;
#29291 = EDGE_CURVE ( 'NONE', #18608, #5258, #28990, .T. ) ;
#29292 = CARTESIAN_POINT ( 'NONE',  ( 58.66122797211814088, -1.815363284467121252, 0.4694237433642899360 ) ) ;
#29293 = ORIENTED_EDGE ( 'NONE', *, *, #22286, .T. ) ;
#29294 = DIRECTION ( 'NONE',  ( 0.000000000000000000, 0.000000000000000000, 1.000000000000000000 ) ) ;
#29296 = DIRECTION ( 'NONE',  ( 2.010641683997904432E-15, 0.9428090415820644665, -0.3333333333333307613 ) ) ;
#29295 = DIRECTION ( 'NONE',  ( 1.000000000000000000, 1.047444401652940007E-14, 0.000000000000000000 ) ) ;
#29297 = CYLINDRICAL_SURFACE ( 'NONE', #16077, 2.600000000000000089 ) ;
#29298 = VERTEX_POINT ( 'NONE', #25201 ) ;
#29299 = ORIENTED_EDGE ( 'NONE', *, *, #30878, .T. ) ;
#29300 = CARTESIAN_POINT ( 'NONE',  ( 48.50000000000002132, -1.426739617975173013, 3.843750000000023093 ) ) ;
#29301 = ORIENTED_EDGE ( 'NONE', *, *, #29808, .F. ) ;
#29302 = CARTESIAN_POINT ( 'NONE',  ( -73.89999999999997726, -2.435524336289708093E-15, 4.607889071584891164E-15 ) ) ;
#29303 = CARTESIAN_POINT ( 'NONE',  ( -55.17292740578361077, 2.256877952708269408, -2.542931754211925632 ) ) ;
#29304 = CARTESIAN_POINT ( 'NONE',  ( -59.60196120585266044, -2.158270994723152647, 1.537682753760200027 ) ) ;
#29305 = VERTEX_POINT ( 'NONE', #14905 ) ;
#29306 = CARTESIAN_POINT ( 'NONE',  ( -59.29999999999999005, -2.874490093629469278, -2.376013416532390732 ) ) ;
#29307 = CIRCLE ( 'NONE', #18697, 4.375000000000000000 ) ;
#29308 = SURFACE_SIDE_STYLE ('',( #27072 ) ) ;
#29309 = EDGE_LOOP ( 'NONE', ( #11818, #19463, #18999, #25832, #3155 ) ) ;
#29310 = AXIS2_PLACEMENT_3D ( 'NONE', #8190, #3454, #20713 ) ;
#29311 = ADVANCED_FACE ( 'NONE', ( #3517 ), #19836, .F. ) ;
#29312 = VECTOR ( 'NONE', #14429, 999.9999999999998863 ) ;
#29313 = CARTESIAN_POINT ( 'NONE',  ( -57.00952994616205416, -4.643455692769903542E-15, 3.599999999999796696 ) ) ;
#29314 = CARTESIAN_POINT ( 'NONE',  ( 50.30000000000001847, 1.426739617975221641, 3.843750000000023093 ) ) ;
#29316 = ADVANCED_FACE ( 'NONE', ( #29466 ), #30665, .T. ) ;
#29315 = CARTESIAN_POINT ( 'NONE',  ( -54.48531357662248809, -1.514292094527452948, 3.309285685900293039 ) ) ;
#29317 = CARTESIAN_POINT ( 'NONE',  ( 69.25000000000000000, -0.8558823529411765385, -2.268940368966791077 ) ) ;
#29318 = AXIS2_PLACEMENT_3D ( 'NONE', #30271, #15860, #16022 ) ;
#29319 = CARTESIAN_POINT ( 'NONE',  ( -57.01905989232412963, 2.944486372867089141, 1.699999999999813216 ) ) ;
#29320 = CARTESIAN_POINT ( 'NONE',  ( -35.85663232820579793, -1.123735532908308965, -5.289358697221545391 ) ) ;
#29321 = DIRECTION ( 'NONE',  ( 1.000000000000000000, 1.047444401652940007E-14, 0.000000000000000000 ) ) ;
#29322 = CARTESIAN_POINT ( 'NONE',  ( 48.49151045397272952, 1.391941090707534689, -3.850000000000023181 ) ) ;
#29324 = CARTESIAN_POINT ( 'NONE',  ( -62.09999999999997300, -2.663342603746559512, -0.2885805439117342108 ) ) ;
#29323 = CARTESIAN_POINT ( 'NONE',  ( 58.75000000000002132, 6.153735859711025284E-13, 3.111507638930570854E-58 ) ) ;
#29325 = EDGE_LOOP ( 'NONE', ( #20248, #2942, #22117, #14801 ) ) ;
#29326 = EDGE_CURVE ( 'NONE', #24402, #6307, #3687, .T. ) ;
#29327 = DIRECTION ( 'NONE',  ( 1.000000000000000000, 2.586136946169074517E-16, -0.000000000000000000 ) ) ;
#29328 = CARTESIAN_POINT ( 'NONE',  ( -36.92398358572908990, -5.053896291911982530, -1.944420249220666586 ) ) ;
#29330 = CARTESIAN_POINT ( 'NONE',  ( 52.50319102799119264, 3.945003566797451899, -1.118186572507700038 ) ) ;
#29329 = FACE_OUTER_BOUND ( 'NONE', #3655, .T. ) ;
#29331 = CARTESIAN_POINT ( 'NONE',  ( -58.18749999999995737, 1.962990915244761991, -3.400000000000190870 ) ) ;
#29332 = ORIENTED_EDGE ( 'NONE', *, *, #28568, .T. ) ;
#29333 = CARTESIAN_POINT ( 'NONE',  ( -54.39999999999996305, 1.400000000000023670, -3.959797974644871044 ) ) ;
#29334 = ORIENTED_EDGE ( 'NONE', *, *, #6158, .T. ) ;
#29335 = CARTESIAN_POINT ( 'NONE',  ( 15.71019289815287934, -5.349060760730925068, 0.7993770229878324196 ) ) ;
#29336 = ORIENTED_EDGE ( 'NONE', *, *, #26246, .F. ) ;
#29337 = ADVANCED_FACE ( 'NONE', ( #30556 ), #7218, .F. ) ;
#29338 = ORIENTED_EDGE ( 'NONE', *, *, #11047, .F. ) ;
#29339 = CARTESIAN_POINT ( 'NONE',  ( -44.59999999999996589, -1.499999999999981126, -3.363870538531657406 ) ) ;
#29340 = VERTEX_POINT ( 'NONE', #6513 ) ;
#29341 = CIRCLE ( 'NONE', #26814, 4.375000000000000000 ) ;
#29342 = CARTESIAN_POINT ( 'NONE',  ( 58.50000000000001421, 0.8156862745098042433, -2.468735688885369317 ) ) ;
#29343 = CARTESIAN_POINT ( 'NONE',  ( -60.38452994616202574, 2.093608279459374244E-14, -3.600000000000214140 ) ) ;
#29344 = EDGE_LOOP ( 'NONE', ( #24573, #28984, #22218, #25430 ) ) ;
#29345 = DIRECTION ( 'NONE',  ( 0.000000000000000000, 1.000000000000000000, 0.000000000000000000 ) ) ;
#29346 = FACE_OUTER_BOUND ( 'NONE', #21111, .T. ) ;
#29347 = CARTESIAN_POINT ( 'NONE',  ( -61.14517784068949879, -2.535105743723619742, -0.9343305864993693977 ) ) ;
#29348 = EDGE_LOOP ( 'NONE', ( #10062, #2144, #29512 ) ) ;
#29349 = EDGE_CURVE ( 'NONE', #18823, #3768, #3372, .T. ) ;
#29350 = CARTESIAN_POINT ( 'NONE',  ( 52.06628335902944826, 0.5434431642986596867, -1.718465885608439603 ) ) ;
#29351 = ADVANCED_FACE ( 'NONE', ( #1918 ), #30090, .T. ) ;
#29352 = CARTESIAN_POINT ( 'NONE',  ( -54.45981523601835761, -1.500740478982482973, 4.030402907299741599 ) ) ;
#29353 = DIRECTION ( 'NONE',  ( 1.000000000000000000, 1.047444401652940007E-14, 0.000000000000000000 ) ) ;
#29355 = ADVANCED_FACE ( 'NONE', ( #18093 ), #11098, .T. ) ;
#29354 = CARTESIAN_POINT ( 'NONE',  ( 47.00000000000002132, 1.734723475976807094E-15, 0.000000000000000000 ) ) ;
#29356 = CARTESIAN_POINT ( 'NONE',  ( 57.01549179440438309, 0.7366256376427431363, 2.429951667075468613 ) ) ;
#29358 = DIRECTION ( 'NONE',  ( 1.000000000000000000, 1.047444401652940007E-14, 0.000000000000000000 ) ) ;
#29357 = DIRECTION ( 'NONE',  ( 0.000000000000000000, 1.000000000000000000, 0.000000000000000000 ) ) ;
#29359 = CARTESIAN_POINT ( 'NONE',  ( 50.31874172786521626, -1.426739617975169905, -3.843750000000023537 ) ) ;
#29360 = CARTESIAN_POINT ( 'NONE',  ( 58.64999999999999858, 1.872332544501737361, 0.09997921184905503300 ) ) ;
#29361 = DIRECTION ( 'NONE',  ( 0.000000000000000000, -1.000000000000000000, -4.336808689942015369E-15 ) ) ;
#29362 = EDGE_LOOP ( 'NONE', ( #3520, #9751, #23264, #24524 ) ) ;
#29363 = ORIENTED_EDGE ( 'NONE', *, *, #21915, .T. ) ;
#29364 = ORIENTED_EDGE ( 'NONE', *, *, #18097, .F. ) ;
#29365 =( BOUNDED_CURVE ( )  B_SPLINE_CURVE ( 3, ( #16752, #19289, #11827, #12147 ),
 .UNSPECIFIED., .F., .T. ) 
 B_SPLINE_CURVE_WITH_KNOTS ( ( 4, 4 ),
 ( 2.002124161478338937, 2.111507728364524272 ),
 .UNSPECIFIED. ) 
 CURVE ( )  GEOMETRIC_REPRESENTATION_ITEM ( )  RATIONAL_B_SPLINE_CURVE ( ( 1.000000000000000000, 0.9990031847838436452, 0.9990031847838436452, 1.000000000000000000 ) ) 
 REPRESENTATION_ITEM ( '' )  );
#29366 = DIRECTION ( 'NONE',  ( 0.000000000000000000, 0.000000000000000000, -1.000000000000000000 ) ) ;
#29367 = CARTESIAN_POINT ( 'NONE',  ( -60.23542740578359656, 2.936324665650206889, 2.606018187048499524 ) ) ;
#29369 = CARTESIAN_POINT ( 'NONE',  ( 47.05963571244990362, 8.266527678078146479, -2.050000000000163691 ) ) ;
#29368 = CARTESIAN_POINT ( 'NONE',  ( 15.03925126672132784, 5.377732432866636714, 0.5657657256216092057 ) ) ;
#29370 = ORIENTED_EDGE ( 'NONE', *, *, #10477, .T. ) ;
#29371 = EDGE_CURVE ( 'NONE', #25975, #23625, #10955, .T. ) ;
#29372 = ORIENTED_EDGE ( 'NONE', *, *, #9899, .F. ) ;
#29373 = CARTESIAN_POINT ( 'NONE',  ( 53.90826771765248537, 6.078164526406591328, -1.689602626210267466 ) ) ;
#29374 = ORIENTED_EDGE ( 'NONE', *, *, #7778, .F. ) ;
#29375 = B_SPLINE_CURVE_WITH_KNOTS ( 'NONE', 3,
 ( #26765, #26545, #26242, #16754, #16276, #11994, #14351, #9155, #28780, #11682, #28461, #18971, #14200, #19140, #6764, #9635 ),
 .UNSPECIFIED., .F., .F.,
 ( 4, 3, 3, 3, 3, 4 ),
 ( 0.000000000000000000, 3.327919720224046293E-05, 6.635940013767358458E-05, 0.0001026099359405011871, 0.0001331273372812267933, 0.0001352886551855475084 ),
 .UNSPECIFIED. ) ;
#29376 = LINE ( 'NONE', #10071, #12519 ) ;
#29377 = ORIENTED_EDGE ( 'NONE', *, *, #2761, .F. ) ;
#29378 = CARTESIAN_POINT ( 'NONE',  ( 33.98208436257626630, 8.188484708539069956, -1.950000000000503775 ) ) ;
#29379 = EDGE_CURVE ( 'NONE', #1808, #10647, #18716, .T. ) ;
#29380 = VERTEX_POINT ( 'NONE', #6664 ) ;
#29381 = DIRECTION ( 'NONE',  ( 0.000000000000000000, -1.000000000000000000, -4.336808689942015369E-15 ) ) ;
#29382 = CARTESIAN_POINT ( 'NONE',  ( 57.02942257420237837, 0.7458803891215903814, 1.782029179052657009 ) ) ;
#29383 = CARTESIAN_POINT ( 'NONE',  ( 15.45522337368516119, -4.885888067249546829, -1.790336215468742997 ) ) ;
#29384 = CARTESIAN_POINT ( 'NONE',  ( -54.70655989232413674, 1.962990915244722245, 3.399999999999812950 ) ) ;
#29386 = EDGE_CURVE ( 'NONE', #22370, #15602, #6198, .T. ) ;
#29385 = CARTESIAN_POINT ( 'NONE',  ( 51.29912638713658168, 3.898228643449899167, -2.050000000000178790 ) ) ;
#29387 = DIRECTION ( 'NONE',  ( 0.000000000000000000, 0.000000000000000000, 1.000000000000000000 ) ) ;
#29388 = CARTESIAN_POINT ( 'NONE',  ( 50.30000000000001847, 1.409901620910219311, -3.850000000000021849 ) ) ;
#29389 = CARTESIAN_POINT ( 'NONE',  ( 15.03925126672133139, -4.683225679163337318, -2.703237727951242508 ) ) ;
#29390 = AXIS2_PLACEMENT_3D ( 'NONE', #11301, #18456, #4183 ) ;
#29391 = DIRECTION ( 'NONE',  ( 3.002035892788117459E-16, -0.9996898646859343485, -0.02490330187381123786 ) ) ;
#29392 = ORIENTED_EDGE ( 'NONE', *, *, #21227, .F. ) ;
#29393 = CARTESIAN_POINT ( 'NONE',  ( 53.81457038983117513, 5.799118250651475570, -1.689328355159275041 ) ) ;
#29394 = CARTESIAN_POINT ( 'NONE',  ( -36.22909104983324369, -2.595074437875156903, -4.757608386864808914 ) ) ;
#29395 = DIRECTION ( 'NONE',  ( 1.000000000000000000, 1.047444401652940007E-14, 0.000000000000000000 ) ) ;
#29396 = EDGE_LOOP ( 'NONE', ( #59, #19315, #20505, #4576, #17621, #8429 ) ) ;
#29397 = CARTESIAN_POINT ( 'NONE',  ( 50.42181344116571751, 1.309616516426969302, -3.885368734293527471 ) ) ;
#29398 =( BOUNDED_CURVE ( )  B_SPLINE_CURVE ( 3, ( #21552, #3959, #13602, #18544 ),
 .UNSPECIFIED., .F., .T. ) 
 B_SPLINE_CURVE_WITH_KNOTS ( ( 4, 4 ),
 ( 4.712388980384687898, 6.283185307179586232 ),
 .UNSPECIFIED. ) 
 CURVE ( )  GEOMETRIC_REPRESENTATION_ITEM ( )  RATIONAL_B_SPLINE_CURVE ( ( 1.000000000000000000, 0.8047378541243646044, 0.8047378541243646044, 1.000000000000000000 ) ) 
 REPRESENTATION_ITEM ( '' )  );
#29399 = ORIENTED_EDGE ( 'NONE', *, *, #8366, .F. ) ;
#29400 = CARTESIAN_POINT ( 'NONE',  ( -35.85663232820584057, 0.4576450603546987628, 5.200000000000000178 ) ) ;
#29401 = CARTESIAN_POINT ( 'NONE',  ( -36.89017861347080185, -5.034707333629141246, 1.977875755500610122 ) ) ;
#29403 = CARTESIAN_POINT ( 'NONE',  ( -60.24999999999997868, 2.040177471463716435E-15, 6.193977072552205884E-16 ) ) ;
#29402 = CARTESIAN_POINT ( 'NONE',  ( 48.30260100412290569, -0.9326869175216284669, -3.995127421239667687 ) ) ;
#29404 = ORIENTED_EDGE ( 'NONE', *, *, #23887, .T. ) ;
#29405 = EDGE_CURVE ( 'NONE', #5422, #25428, #28010, .T. ) ;
#29406 = DIRECTION ( 'NONE',  ( 1.000000000000000000, 0.000000000000000000, -1.047444401652940007E-14 ) ) ;
#29407 = EDGE_CURVE ( 'NONE', #30896, #31077, #29136, .T. ) ;
#29408 = CARTESIAN_POINT ( 'NONE',  ( 58.75000000000000711, 1.323060376181323550, 1.499837071479058981 ) ) ;
#29409 = AXIS2_PLACEMENT_3D ( 'NONE', #20191, #5449, #13033 ) ;
#29411 = CARTESIAN_POINT ( 'NONE',  ( -59.69865663803934552, 2.434220863071083318, -1.237763019072676940 ) ) ;
#29410 = CARTESIAN_POINT ( 'NONE',  ( -57.95655989232411542, 1.962990915244761103, -3.400000000000189981 ) ) ;
#29412 = EDGE_CURVE ( 'NONE', #11849, #6214, #21261, .T. ) ;
#29413 = CARTESIAN_POINT ( 'NONE',  ( 52.20711756518984714, -0.6499999999994534594, -1.489337100860648189 ) ) ;
#29414 = CARTESIAN_POINT ( 'NONE',  ( -59.93749999999997158, 0.8699069336946682052, -4.241846523238426592 ) ) ;
#29415 = CARTESIAN_POINT ( 'NONE',  ( 57.00357781822870606, -0.7683521053270409018, 1.737709711729638729 ) ) ;
#29416 = FACE_OUTER_BOUND ( 'NONE', #27384, .T. ) ;
#29417 = LINE ( 'NONE', #22634, #18006 ) ;
#29418 = CYLINDRICAL_SURFACE ( 'NONE', #13686, 0.09999999999999982514 ) ;
#29419 = FACE_OUTER_BOUND ( 'NONE', #15718, .T. ) ;
#29420 = CARTESIAN_POINT ( 'NONE',  ( 16.08093158123429589, -0.2888463313200277383, 5.401384060636566176 ) ) ;
#29421 = ORIENTED_EDGE ( 'NONE', *, *, #2433, .F. ) ;
#29422 = EDGE_CURVE ( 'NONE', #1939, #27496, #14998, .T. ) ;
#29423 = CARTESIAN_POINT ( 'NONE',  ( 61.09423418604048095, 0.6373668173476213505, -1.895722432252298084 ) ) ;
#29424 = CARTESIAN_POINT ( 'NONE',  ( -62.06710100716625789, -2.637635658083895329, 0.1963493119579511614 ) ) ;
#29425 = CARTESIAN_POINT ( 'NONE',  ( 51.80000000000001847, 2.428612866367529932E-14, -1.808587333520743709E-13 ) ) ;
#29426 = CARTESIAN_POINT ( 'NONE',  ( -56.87499999999997158, 2.489203624310596386, -2.804704140674913582 ) ) ;
#29428 = CARTESIAN_POINT ( 'NONE',  ( 30.78427835929706191, 7.077770142316436974, 1.424999999999892353 ) ) ;
#29427 = CARTESIAN_POINT ( 'NONE',  ( 51.51881050553487995, -3.793704335752947632, 1.557065711441241840 ) ) ;
#29429 = ORIENTED_EDGE ( 'NONE', *, *, #813, .F. ) ;
#29430 = DIRECTION ( 'NONE',  ( 0.000000000000000000, 0.000000000000000000, 1.000000000000000000 ) ) ;
#29431 = ORIENTED_EDGE ( 'NONE', *, *, #7889, .T. ) ;
#29432 = CARTESIAN_POINT ( 'NONE',  ( 60.81555826527925035, 0.6500000000006364020, 1.489337100860648633 ) ) ;
#29434 = DIRECTION ( 'NONE',  ( 1.000000000000000000, 3.053848253006669023E-16, -2.042510438544995415E-16 ) ) ;
#29433 = CARTESIAN_POINT ( 'NONE',  ( 15.74652664997095286, -3.345968172200381119, -4.250076229745499923 ) ) ;
#29435 = DIRECTION ( 'NONE',  ( 0.000000000000000000, -0.9996898646859343485, -0.02490330187381123786 ) ) ;
#29436 = ORIENTED_EDGE ( 'NONE', *, *, #20534, .F. ) ;
#29437 = VERTEX_POINT ( 'NONE', #7146 ) ;
#29438 = DIRECTION ( 'NONE',  ( 1.000000000000000000, -0.000000000000000000, -0.000000000000000000 ) ) ;
#29439 = EDGE_CURVE ( 'NONE', #1323, #4682, #24240, .T. ) ;
#29440 = CARTESIAN_POINT ( 'NONE',  ( 51.78364358464218498, 0.9002346248705929144, 1.360127766454912068 ) ) ;
#29441 = ORIENTED_EDGE ( 'NONE', *, *, #8319, .T. ) ;
#29442 = LINE ( 'NONE', #14733, #29180 ) ;
#29443 = CARTESIAN_POINT ( 'NONE',  ( 50.40000000000001990, 0.6304760106459513791, 3.950000000000022826 ) ) ;
#29444 = AXIS2_PLACEMENT_3D ( 'NONE', #11706, #27574, #16018 ) ;
#29445 = CARTESIAN_POINT ( 'NONE',  ( -35.85663232820578372, -5.377732432866659806, -0.5657657256215627983 ) ) ;
#29446 = VERTEX_POINT ( 'NONE', #31037 ) ;
#29447 = CARTESIAN_POINT ( 'NONE',  ( -59.29999999999996163, -3.060620570343238089, 1.662570173752615954 ) ) ;
#29448 = VERTEX_POINT ( 'NONE', #16480 ) ;
#29449 = EDGE_CURVE ( 'NONE', #25335, #8618, #26994, .T. ) ;
#29450 = CARTESIAN_POINT ( 'NONE',  ( -58.07202994616203995, 2.078460969082674747, -3.600000000000197709 ) ) ;
#29451 = CARTESIAN_POINT ( 'NONE',  ( -55.20655989232412963, -3.399999999999991473, -2.086450695418937968E-13 ) ) ;
#29452 = CARTESIAN_POINT ( 'NONE',  ( 48.42176022524417789, -1.183413901109541477, -3.885761703493072261 ) ) ;
#29453 = CARTESIAN_POINT ( 'NONE',  ( -54.46926330052497178, -1.503605180550109388, 3.302415457191588910 ) ) ;
#29454 = DIRECTION ( 'NONE',  ( 1.000000000000000000, 0.000000000000000000, -1.047444401652940007E-14 ) ) ;
#29455 = CARTESIAN_POINT ( 'NONE',  ( -56.95655989232413674, 1.962990915244718915, 3.399999999999805844 ) ) ;
#29457 = CARTESIAN_POINT ( 'NONE',  ( -61.35212809946285972, -2.542122018907453374, -0.7980057954928057029 ) ) ;
#29456 = CARTESIAN_POINT ( 'NONE',  ( 68.00000000000004263, -0.5000000000000000000, 1.988246715072644166 ) ) ;
#29458 = AXIS2_PLACEMENT_3D ( 'NONE', #7039, #14616, #17008 ) ;
#29459 = CARTESIAN_POINT ( 'NONE',  ( -62.09559345744012404, -2.519030794919479010, 0.1735854400584113666 ) ) ;
#29460 = DIRECTION ( 'NONE',  ( -1.000000000000000000, 1.219044193948983948E-29, -3.491481338843133355E-15 ) ) ;
#29462 = DIRECTION ( 'NONE',  ( -2.614375865348241018E-16, 0.2008964009354147762, -0.9796124928211140670 ) ) ;
#29461 = CARTESIAN_POINT ( 'NONE',  ( 15.49676243306307377, 4.963067629822636384, -1.552801941062253999 ) ) ;
#29463 = ORIENTED_EDGE ( 'NONE', *, *, #24764, .T. ) ;
#29464 = CARTESIAN_POINT ( 'NONE',  ( 50.38490132722630932, -1.114141714781589521, -3.896173399896524003 ) ) ;
#29465 = CARTESIAN_POINT ( 'NONE',  ( 51.74870924761699342, 3.850494199885640345, 1.444083690939125697 ) ) ;
#29467 = CARTESIAN_POINT ( 'NONE',  ( 52.06031971197555919, 3.858116234519211929, -1.389650576489513956 ) ) ;
#29466 = FACE_OUTER_BOUND ( 'NONE', #16821, .T. ) ;
#29468 = CARTESIAN_POINT ( 'NONE',  ( 47.86851286004601036, -4.319730106380312407, 1.256953381515252044 ) ) ;
#29469 = ORIENTED_EDGE ( 'NONE', *, *, #3676, .T. ) ;
#29470 = CARTESIAN_POINT ( 'NONE',  ( -61.38468220210111070, -2.652782842985662803, 0.4917085785661312047 ) ) ;
#29471 = EDGE_CURVE ( 'NONE', #26348, #19839, #19069, .T. ) ;
#29472 = EDGE_LOOP ( 'NONE', ( #9668, #11477, #11101, #2002 ) ) ;
#29473 = DIRECTION ( 'NONE',  ( -1.000000000000000000, -3.053848253006669023E-16, 2.042510438544995415E-16 ) ) ;
#29474 = EDGE_LOOP ( 'NONE', ( #21118, #13609 ) ) ;
#29475 = ORIENTED_EDGE ( 'NONE', *, *, #10252, .F. ) ;
#29476 = CARTESIAN_POINT ( 'NONE',  ( 15.44631504820157097, 5.012449653004692252, 1.400819699606158819 ) ) ;
#29477 = ORIENTED_EDGE ( 'NONE', *, *, #26993, .F. ) ;
#29478 = CARTESIAN_POINT ( 'NONE',  ( 33.10182602044763200, 8.045524457602619250, 1.949999999999884714 ) ) ;
#29479 = CARTESIAN_POINT ( 'NONE',  ( -60.75952994616205416, -4.643455692769856999E-15, 3.599999999999783373 ) ) ;
#29480 = ORIENTED_EDGE ( 'NONE', *, *, #7850, .F. ) ;
#29481 = DIRECTION ( 'NONE',  ( 0.000000000000000000, 0.000000000000000000, -1.000000000000000000 ) ) ;
#29482 = EDGE_LOOP ( 'NONE', ( #29710, #30452, #10067, #16609 ) ) ;
#29483 = CARTESIAN_POINT ( 'NONE',  ( 58.75000000000002132, 6.153735859711025284E-13, 3.111507638930570854E-58 ) ) ;
#29484 = AXIS2_PLACEMENT_3D ( 'NONE', #197, #10029, #14609 ) ;
#29485 = CARTESIAN_POINT ( 'NONE',  ( 48.40000000000001990, -4.899999999999999467, 3.850000000000022737 ) ) ;
#29486 = ORIENTED_EDGE ( 'NONE', *, *, #19545, .T. ) ;
#29487 = EDGE_CURVE ( 'NONE', #16075, #4682, #8911, .T. ) ;
#29488 = CARTESIAN_POINT ( 'NONE',  ( 51.71101551635177884, -4.179189514726506793, -1.000000000000000000 ) ) ;
#29489 = CARTESIAN_POINT ( 'NONE',  ( -54.49998548284560940, -1.548795215916124457, 4.063650232134933482 ) ) ;
#29490 = CARTESIAN_POINT ( 'NONE',  ( -59.29999999999997584, -0.7533615035078030653, 3.673546848079178417 ) ) ;
#29491 = CYLINDRICAL_SURFACE ( 'NONE', #25576, 1.000000000000000000 ) ;
#29492 = CARTESIAN_POINT ( 'NONE',  ( -59.19999999999997442, 3.161828374300071687, 1.250136525132551357 ) ) ;
#29493 = B_SPLINE_CURVE_WITH_KNOTS ( 'NONE', 3,
 ( #28537, #4305, #18584, #11442, #9387, #16514, #26169, #25697, #21288, #18422, #6540, #28059, #6380, #4476, #11271, #23802 ),
 .UNSPECIFIED., .F., .F.,
 ( 4, 2, 2, 2, 2, 2, 2, 4 ),
 ( 0.000000000000000000, 0.0004351083927046389579, 0.0008702167854092779159, 0.001740433570818555615, 0.002175541963523194844, 0.002610650356227833639, 0.003045758748932472868, 0.003480867141637111663 ),
 .UNSPECIFIED. ) ;
#29495 = DIRECTION ( 'NONE',  ( 0.000000000000000000, 0.000000000000000000, 1.000000000000000000 ) ) ;
#29494 = CARTESIAN_POINT ( 'NONE',  ( -36.30347965937246357, -2.964363692626382552, 4.273817190665925914 ) ) ;
#29496 = ADVANCED_FACE ( 'NONE', ( #21564 ), #16958, .T. ) ;
#29497 = CARTESIAN_POINT ( 'NONE',  ( 47.00000000000002132, -3.726179070414207928, -1.100000000000000089 ) ) ;
#29498 = FACE_OUTER_BOUND ( 'NONE', #30822, .T. ) ;
#29499 = CARTESIAN_POINT ( 'NONE',  ( -54.49999999999997868, 1.549582583372307809, -3.331868970650947226 ) ) ;
#29500 = CARTESIAN_POINT ( 'NONE',  ( 53.29207122288458720, 4.934008984266801789, 1.614082030464476292 ) ) ;
#29501 = VECTOR ( 'NONE', #9285, 1000.000000000000000 ) ;
#29502 = EDGE_LOOP ( 'NONE', ( #8218, #22119, #23819, #11639 ) ) ;
#29503 = ORIENTED_EDGE ( 'NONE', *, *, #30957, .F. ) ;
#29504 = ADVANCED_FACE ( 'NONE', ( #16658 ), #938, .T. ) ;
#29505 = ORIENTED_EDGE ( 'NONE', *, *, #23316, .T. ) ;
#29506 = EDGE_CURVE ( 'NONE', #16699, #13465, #3883, .T. ) ;
#29507 = CARTESIAN_POINT ( 'NONE',  ( -62.09999999999997300, -2.509076856576755166, -0.2831785779091364752 ) ) ;
#29508 = CARTESIAN_POINT ( 'NONE',  ( -59.92292740578359656, -3.330682475591783653, -0.6830477631804103833 ) ) ;
#29510 = DIRECTION ( 'NONE',  ( 1.000000000000000000, 0.000000000000000000, 0.000000000000000000 ) ) ;
#29509 = CARTESIAN_POINT ( 'NONE',  ( 15.70940947763170215, 5.349174094756180331, 0.7986533162261519880 ) ) ;
#29511 = EDGE_CURVE ( 'NONE', #24802, #16489, #2914, .T. ) ;
#29512 = ORIENTED_EDGE ( 'NONE', *, *, #20410, .T. ) ;
#29513 = ORIENTED_EDGE ( 'NONE', *, *, #11983, .F. ) ;
#29514 = CARTESIAN_POINT ( 'NONE',  ( 51.42113644652349080, -4.356776102639509318, -1.481376528584163577 ) ) ;
#29515 = ORIENTED_EDGE ( 'NONE', *, *, #14323, .F. ) ;
#29516 = DIRECTION ( 'NONE',  ( -1.000000000000000000, -3.053848253006669023E-16, 2.042510438544995415E-16 ) ) ;
#29517 = ORIENTED_EDGE ( 'NONE', *, *, #10051, .F. ) ;
#29518 = CARTESIAN_POINT ( 'NONE',  ( 26.61920844898535776, 5.219578738934656847, -1.950000000000091438 ) ) ;
#29519 = VERTEX_POINT ( 'NONE', #7906 ) ;
#29520 = CARTESIAN_POINT ( 'NONE',  ( 15.03925126672132961, 4.018128179617504792, 3.618665901676689778 ) ) ;
#29521 = CARTESIAN_POINT ( 'NONE',  ( 47.28076429169690442, -3.793498434807316855, 1.557570148622769546 ) ) ;
#29522 = EDGE_CURVE ( 'NONE', #8786, #24661, #20127, .T. ) ;
#29523 = CARTESIAN_POINT ( 'NONE',  ( 15.49702763512084225, -4.962395293451320022, -1.554871187131938726 ) ) ;
#29525 = CARTESIAN_POINT ( 'NONE',  ( -57.14405989232411542, 2.944486372867106461, -1.700000000000190248 ) ) ;
#29524 = CIRCLE ( 'NONE', #18430, 0.09999999999999982514 ) ;
#29526 = CARTESIAN_POINT ( 'NONE',  ( 54.21235476094169314, 5.862613896911505584, -2.050000000000189004 ) ) ;
#29527 = CARTESIAN_POINT ( 'NONE',  ( 58.75000000000000711, 1.457351493771914086, 1.320164791810606975 ) ) ;
#29528 = DIRECTION ( 'NONE',  ( -1.000000000000000000, 0.000000000000000000, 0.000000000000000000 ) ) ;
#29529 = DIRECTION ( 'NONE',  ( 1.000000000000000000, 1.047444401652940007E-14, 0.000000000000000000 ) ) ;
#29530 = DIRECTION ( 'NONE',  ( 1.000000000000000000, 1.047444401652940007E-14, -0.000000000000000000 ) ) ;
#29531 = EDGE_CURVE ( 'NONE', #8120, #24812, #25615, .T. ) ;
#29532 = DIRECTION ( 'NONE',  ( 1.000000000000000000, 0.000000000000000000, 0.000000000000000000 ) ) ;
#29533 = DIRECTION ( 'NONE',  ( -1.000000000000000000, -3.053848253006669023E-16, 2.042510438544995415E-16 ) ) ;
#29535 = EDGE_CURVE ( 'NONE', #1037, #27064, #23107, .T. ) ;
#29534 = CARTESIAN_POINT ( 'NONE',  ( 51.13858604272873976, -1.070913481528389166, 1.222302725805714640 ) ) ;
#29536 =( BOUNDED_CURVE ( )  B_SPLINE_CURVE ( 2, ( #3947, #12976, #18365, #1248, #18524, #10910, #13587, #6030, #23277 ),
 .UNSPECIFIED., .F., .T. ) 
 B_SPLINE_CURVE_WITH_KNOTS ( ( 3, 2, 2, 2, 3 ),
 ( 0.1944444444444444475, 0.2037037037037036924, 0.2222222222222222099, 0.2407407407407407274, 0.2500000000000000000 ),
 .UNSPECIFIED. ) 
 CURVE ( )  GEOMETRIC_REPRESENTATION_ITEM ( )  RATIONAL_B_SPLINE_CURVE ( ( 0.9330127018922192983, 0.9330127018922194093, 1.000000000000000000, 0.8660254037844387076, 1.000000000000000000, 0.8660254037844387076, 1.000000000000000000, 0.9330127018922191873, 0.9330127018922192983 ) ) 
 REPRESENTATION_ITEM ( '' )  );
#29537 = ORIENTED_EDGE ( 'NONE', *, *, #26854, .T. ) ;
#29538 = TOROIDAL_SURFACE ( 'NONE', #15897, 4.800000000000000711, 0.05000000000000000278 ) ;
#29539 = CARTESIAN_POINT ( 'NONE',  ( 58.65000000000001990, 6.143261415694495821E-13, 3.111507638930570854E-58 ) ) ;
#29540 = CARTESIAN_POINT ( 'NONE',  ( 51.47729133425627168, -0.9526829978892299433, -1.321356857233840110 ) ) ;
#29541 = CARTESIAN_POINT ( 'NONE',  ( 54.17607972459842358, 5.677832729363556652, 2.049999999999814637 ) ) ;
#29542 = ORIENTED_EDGE ( 'NONE', *, *, #21332, .F. ) ;
#29543 = FACE_OUTER_BOUND ( 'NONE', #22300, .T. ) ;
#29544 = EDGE_LOOP ( 'NONE', ( #9175, #18175, #18574, #337 ) ) ;
#29545 = EDGE_CURVE ( 'NONE', #24288, #30697, #12372, .T. ) ;
#29546 = DIRECTION ( 'NONE',  ( 0.000000000000000000, 0.000000000000000000, 1.000000000000000000 ) ) ;
#29547 = CIRCLE ( 'NONE', #7811, 0.1500000000000003830 ) ;
#29548 = CARTESIAN_POINT ( 'NONE',  ( -54.34585481156724285, -1.184343223768585807, -3.558065644182726306 ) ) ;
#29550 = DIRECTION ( 'NONE',  ( 0.000000000000000000, 0.000000000000000000, -1.000000000000000000 ) ) ;
#29549 = CARTESIAN_POINT ( 'NONE',  ( 51.04089638944252272, -4.379721596991722699, 1.407221449367199506 ) ) ;
#29551 = ADVANCED_FACE ( 'NONE', ( #18675 ), #27715, .T. ) ;
#29552 = VERTEX_POINT ( 'NONE', #11065 ) ;
#29553 = CARTESIAN_POINT ( 'NONE',  ( 60.89136863770560382, -0.4999999999993600119, -1.718465794862841678 ) ) ;
#29554 = FACE_OUTER_BOUND ( 'NONE', #21787, .T. ) ;
#29555 = EDGE_LOOP ( 'NONE', ( #12140, #7603, #871, #29131 ) ) ;
#29557 = DIRECTION ( 'NONE',  ( -1.344447539785323523E-44, 1.000000000000000000, 3.491481338843137300E-15 ) ) ;
#29556 = DIRECTION ( 'NONE',  ( 1.000000000000000000, 0.000000000000000000, -1.047444401652940007E-14 ) ) ;
#29558 = AXIS2_PLACEMENT_3D ( 'NONE', #25827, #28215, #23457 ) ;
#29559 = ORIENTED_EDGE ( 'NONE', *, *, #9122, .F. ) ;
#29560 = CARTESIAN_POINT ( 'NONE',  ( -57.18749999999997158, -4.108500314926507357, 1.367561758111406345 ) ) ;
#29561 = DIRECTION ( 'NONE',  ( 1.000000000000000000, 3.053848253006669023E-16, -2.042510438544995415E-16 ) ) ;
#29562 = DIRECTION ( 'NONE',  ( 1.000000000000000000, 0.000000000000000000, 0.000000000000000000 ) ) ;
#29563 = CARTESIAN_POINT ( 'NONE',  ( -54.50000000000001421, -1.699814003251586492, -3.091037575173824603 ) ) ;
#29564 = CARTESIAN_POINT ( 'NONE',  ( -59.27326758270456253, -1.949102190723507100, -3.303506793698848476 ) ) ;
#29565 = CARTESIAN_POINT ( 'NONE',  ( -71.44999999999998863, -1.380331489585512972E-15, 2.906968604901091669E-15 ) ) ;
#29566 = CARTESIAN_POINT ( 'NONE',  ( 51.78364358464229866, -0.9002346248695359821, -1.360127766454889642 ) ) ;
#29568 = ORIENTED_EDGE ( 'NONE', *, *, #28491, .T. ) ;
#29567 = AXIS2_PLACEMENT_3D ( 'NONE', #21798, #29358, #15261 ) ;
#29569 = CARTESIAN_POINT ( 'NONE',  ( 15.48686146417447240, 3.146183597690325850, 4.141717300434360816 ) ) ;
#29570 = CIRCLE ( 'NONE', #12373, 0.05000000000000007216 ) ;
#29571 = ADVANCED_FACE ( 'NONE', ( #9004 ), #1946, .T. ) ;
#29572 = EDGE_CURVE ( 'NONE', #8781, #4844, #15500, .T. ) ;
#29573 = CARTESIAN_POINT ( 'NONE',  ( -60.61746561950877066, -2.507927281935157904, 0.9671963751729155678 ) ) ;
#29574 =( BOUNDED_SURFACE ( )  B_SPLINE_SURFACE ( 3, 2, ( 
 ( #25268, #27807, #23056 ),
 ( #20842, #8174, #6264 ),
 ( #25568, #16087, #8775 ),
 ( #15911, #13690, #23371 ),
 ( #1651, #1354, #17842 ),
 ( #25105, #27479, #5796 ),
 ( #15451, #3435, #8322 ),
 ( #17991, #15770, #22759 ),
 ( #1052, #10703, #27644 ),
 ( #6119, #11023, #30170 ) ),
 .UNSPECIFIED., .F., .F., .F. ) 
 B_SPLINE_SURFACE_WITH_KNOTS ( ( 4, 2, 2, 2, 4 ),
 ( 3, 3 ),
 ( -5.421010862427522170E-20, 0.0003534648051082245031, 0.0007069296102164490062, 0.001060394415324673618, 0.001413859220432898012 ),
 ( 0.000000000000000000, 1.000000000000000000 ),
 .UNSPECIFIED. ) 
 GEOMETRIC_REPRESENTATION_ITEM ( )  RATIONAL_B_SPLINE_SURFACE ( (
 ( 1.000000000000000000, 0.7071067811865467956, 1.000000000000000000),
 ( 1.000000000000000000, 0.6969521241106181320, 1.000000000000000000),
 ( 1.000000000000000000, 0.6903264600367975401, 1.000000000000000000),
 ( 1.000000000000000000, 0.6841066566212652411, 1.000000000000000000),
 ( 1.000000000000000000, 0.6845305055633155167, 1.000000000000000000),
 ( 1.000000000000000000, 0.6885489555143140539, 1.000000000000000000),
 ( 1.000000000000000000, 0.6920376555006676478, 1.000000000000000000),
 ( 1.000000000000000000, 0.6973723772399861298, 1.000000000000000000),
 ( 1.000000000000000000, 0.6992679762642822761, 1.000000000000000000),
 ( 1.000000000000000000, 0.6992058987801010872, 1.000000000000000000) ) ) 
 REPRESENTATION_ITEM ( '' )  SURFACE ( )  );
#29575 = CIRCLE ( 'NONE', #12898, 2.000000000000000000 ) ;
#29577 = ADVANCED_FACE ( 'NONE', ( #3629 ), #16135, .T. ) ;
#29576 = CARTESIAN_POINT ( 'NONE',  ( -71.49999999999998579, -1.395601618875910821E-15, 2.917180974979867506E-15 ) ) ;
#29578 = CARTESIAN_POINT ( 'NONE',  ( -58.88452994616202574, 2.622655696691028948E-14, -3.600000000000208811 ) ) ;
#29579 = DIRECTION ( 'NONE',  ( -1.000000000000000000, 1.219044193948983948E-29, -3.491481338843133355E-15 ) ) ;
#29580 = CARTESIAN_POINT ( 'NONE',  ( 26.90437805175149677, 5.347594907239942685, 2.049999999999904787 ) ) ;
#29581 = EDGE_LOOP ( 'NONE', ( #20647, #16261, #10610, #21664 ) ) ;
#29582 = CARTESIAN_POINT ( 'NONE',  ( -73.84999999999996589, -1.301636140808608788, -0.03242509391109853201 ) ) ;
#29583 = ORIENTED_EDGE ( 'NONE', *, *, #7513, .T. ) ;
#29584 = DIRECTION ( 'NONE',  ( 1.000000000000000000, 3.054025858079668409E-16, -2.042474015755241579E-16 ) ) ;
#29586 = CYLINDRICAL_SURFACE ( 'NONE', #12104, 4.100000000000000533 ) ;
#29585 = CARTESIAN_POINT ( 'NONE',  ( 15.67083574136752944, -3.495540671458118531, -4.131527132740935748 ) ) ;
#29587 = ORIENTED_EDGE ( 'NONE', *, *, #4979, .T. ) ;
#29588 = AXIS2_PLACEMENT_3D ( 'NONE', #25812, #8700, #2061 ) ;
#29589 = VERTEX_POINT ( 'NONE', #13123 ) ;
#29590 = CARTESIAN_POINT ( 'NONE',  ( 60.75000000000001421, 0.5000000000006363798, -1.718465885608440047 ) ) ;
#29591 = TOROIDAL_SURFACE ( 'NONE', #20011, 4.500000000000037303, 0.1000000000000000056 ) ;
#29592 = CARTESIAN_POINT ( 'NONE',  ( 51.98914612709258876, 0.7788013043309388594, 1.433123603079402786 ) ) ;
#29593 = ORIENTED_EDGE ( 'NONE', *, *, #22347, .F. ) ;
#29595 = DIRECTION ( 'NONE',  ( 0.000000000000000000, 0.000000000000000000, -1.000000000000000000 ) ) ;
#29594 = CARTESIAN_POINT ( 'NONE',  ( -58.82202994616202574, 2.078460969082674747, -3.600000000000199929 ) ) ;
#29596 = CARTESIAN_POINT ( 'NONE',  ( 69.20000000000003126, 5.529431079676072613E-15, -7.248315259438346108E-13 ) ) ;
#29597 = CARTESIAN_POINT ( 'NONE',  ( -36.80043232705877898, -5.283830060792408467, -1.151642405604301089 ) ) ;
#29598 = DIRECTION ( 'NONE',  ( 0.000000000000000000, 0.000000000000000000, 1.000000000000000000 ) ) ;
#29599 = AXIS2_PLACEMENT_3D ( 'NONE', #19093, #26506, #23689 ) ;
#29600 = CARTESIAN_POINT ( 'NONE',  ( 58.65838214097827574, -1.349359547237690693, -1.301971553119712688 ) ) ;
#29601 = COLOUR_RGB ( '', 0.66274510, 0.83137255, 0.94901961) ;
#29602 =( REPRESENTATION_RELATIONSHIP ('NONE','NONE', #7047, #3777 ) REPRESENTATION_RELATIONSHIP_WITH_TRANSFORMATION ( #27712 )SHAPE_REPRESENTATION_RELATIONSHIP( ) );
#29603 = ORIENTED_EDGE ( 'NONE', *, *, #28923, .T. ) ;
#29604 = CARTESIAN_POINT ( 'NONE',  ( -56.69702994616203284, -2.078460969082631227, -3.600000000000207923 ) ) ;
#29605 = CARTESIAN_POINT ( 'NONE',  ( 52.09213388422776347, 8.599999999993013233, -2.050000000000181011 ) ) ;
#29606 = CARTESIAN_POINT ( 'NONE',  ( -54.49999999999999289, -1.557046979865776448, 3.273565289174688253 ) ) ;
#29607 = CARTESIAN_POINT ( 'NONE',  ( 15.03925126672122836, -1.123735532908289647, 5.289358697221546279 ) ) ;
#29608 = EDGE_CURVE ( 'NONE', #4841, #20392, #16021, .T. ) ;
#29609 = AXIS2_PLACEMENT_3D ( 'NONE', #24979, #20271, #3472 ) ;
#29610 = CARTESIAN_POINT ( 'NONE',  ( 51.41735323613823994, -3.967853068034125741, 1.365472663300960177 ) ) ;
#29611 = EDGE_CURVE ( 'NONE', #20775, #7673, #9973, .T. ) ;
#29612 = AXIS2_PLACEMENT_3D ( 'NONE', #11394, #14086, #4265 ) ;
#29613 = CYLINDRICAL_SURFACE ( 'NONE', #21623, 3.399999999999999911 ) ;
#29615 = CARTESIAN_POINT ( 'NONE',  ( -36.27260443516959043, -0.1928884786869198564, -5.200000000471145079 ) ) ;
#29614 = CARTESIAN_POINT ( 'NONE',  ( 51.85262340636812439, 0.6891204047495628204, 1.750401715244590095 ) ) ;
#29616 = AXIS2_PLACEMENT_3D ( 'NONE', #25306, #22800, #15181 ) ;
#29617 = CARTESIAN_POINT ( 'NONE',  ( 58.75000000000000711, 1.800471618824943221, -1.039502773795712987 ) ) ;
#29618 = CARTESIAN_POINT ( 'NONE',  ( 48.40000000000002700, 0.7618928438397208902, -3.939512004971702730 ) ) ;
#29619 = VECTOR ( 'NONE', #17647, 1000.000000000000000 ) ;
#29621 = CARTESIAN_POINT ( 'NONE',  ( -71.44999999999998863, -1.380331489585512972E-15, 2.906968604901091669E-15 ) ) ;
#29620 = CARTESIAN_POINT ( 'NONE',  ( -67.34999999999998010, 2.149333209074759221, 0.05354209902869744991 ) ) ;
#29622 = VERTEX_POINT ( 'NONE', #23269 ) ;
#29623 = AXIS2_PLACEMENT_3D ( 'NONE', #17768, #15542, #15699 ) ;
#29624 = CARTESIAN_POINT ( 'NONE',  ( 50.46980263351819929, -1.141995257496313476, -3.938405479918980490 ) ) ;
#29625 = AXIS2_PLACEMENT_3D ( 'NONE', #5456, #12716, #22097 ) ;
#29626 = CYLINDRICAL_SURFACE ( 'NONE', #11289, 3.075000000000000622 ) ;
#29628 = LINE ( 'NONE', #511, #10084 ) ;
#29627 = CARTESIAN_POINT ( 'NONE',  ( 15.68751737981905947, 3.461789369942972705, -4.158232265984232789 ) ) ;
#29629 = DIRECTION ( 'NONE',  ( -0.5633368246415186853, 0.8262273428075416204, 0.000000000000000000 ) ) ;
#29630 = ORIENTED_EDGE ( 'NONE', *, *, #13138, .F. ) ;
#29631 = CARTESIAN_POINT ( 'NONE',  ( -59.92928932188130631, 0.9643027244899926576, -4.702139965541346278 ) ) ;
#29632 = CARTESIAN_POINT ( 'NONE',  ( 47.02986096046866749, -4.166824046520646974, 1.027859347733066198 ) ) ;
#29633 = ADVANCED_FACE ( 'NONE', ( #6020 ), #2127, .F. ) ;
#29634 = VECTOR ( 'NONE', #21578, 1000.000000000000000 ) ;
#29635 = ORIENTED_EDGE ( 'NONE', *, *, #15229, .T. ) ;
#29636 = CARTESIAN_POINT ( 'NONE',  ( 51.16541527693603797, 0.9540616519818778674, -1.477274982328775854 ) ) ;
#29637 = ORIENTED_EDGE ( 'NONE', *, *, #5495, .T. ) ;
#29638 = ORIENTED_EDGE ( 'NONE', *, *, #16418, .T. ) ;
#29639 = TOROIDAL_SURFACE ( 'NONE', #10924, 1.949999999999999956, 0.05000000000000000278 ) ;
#29640 = CARTESIAN_POINT ( 'NONE',  ( 15.03925126672132784, 5.086913985776138070, 1.171642053949162543 ) ) ;
#29641 = ORIENTED_EDGE ( 'NONE', *, *, #7870, .T. ) ;
#29642 = FILL_AREA_STYLE ('',( #13021 ) ) ;
#29643 = CARTESIAN_POINT ( 'NONE',  ( 28.61151848776741602, 5.704727522705969278, 1.949999999999900924 ) ) ;
#29644 = CARTESIAN_POINT ( 'NONE',  ( -54.26905989232411542, 2.023778652682504003E-14, -3.400000000000192646 ) ) ;
#29645 = EDGE_LOOP ( 'NONE', ( #12694, #14958, #28588, #26775 ) ) ;
#29646 = AXIS2_PLACEMENT_3D ( 'NONE', #29323, #29173, #5247 ) ;
#29647 = CARTESIAN_POINT ( 'NONE',  ( 47.00000000000002132, 2.428612866367529932E-14, -1.640996229256273308E-13 ) ) ;
#29648 = VERTEX_POINT ( 'NONE', #23740 ) ;
#29649 = CARTESIAN_POINT ( 'NONE',  ( 61.25000000000003553, -0.9999999999993586242, 1.586072192556190252 ) ) ;
#29650 = CARTESIAN_POINT ( 'NONE',  ( 25.06719628359775953, 5.330953183167972398, 2.049999999999911005 ) ) ;
#29651 = VERTEX_POINT ( 'NONE', #11697 ) ;
#29652 = TOROIDAL_SURFACE ( 'NONE', #23591, 1.949999999999999956, 0.05000000000000000278 ) ;
#29653 = AXIS2_PLACEMENT_3D ( 'NONE', #3337, #12987, #22674 ) ;
#29654 = CARTESIAN_POINT ( 'NONE',  ( -59.21142689504641510, -3.199784673776251864, 1.256733846063594839 ) ) ;
#29655 = CIRCLE ( 'NONE', #27649, 1.875000000000001776 ) ;
#29656 = CARTESIAN_POINT ( 'NONE',  ( 52.72388909184999761, 4.000582417204456398, -2.050000000000183675 ) ) ;
#29657 = FACE_OUTER_BOUND ( 'NONE', #7820, .T. ) ;
#29658 = LINE ( 'NONE', #15255, #29619 ) ;
#29659 = FACE_OUTER_BOUND ( 'NONE', #2231, .T. ) ;
#29660 = EDGE_CURVE ( 'NONE', #21368, #26143, #31224, .T. ) ;
#29662 = CARTESIAN_POINT ( 'NONE',  ( 47.00000000000001421, -3.657334280697314810, -2.105684202162497520 ) ) ;
#29661 = CARTESIAN_POINT ( 'NONE',  ( 51.80000000000001137, -3.637377585518695611, -2.099877210783217318 ) ) ;
#29663 = CIRCLE ( 'NONE', #16014, 0.1000000000000028644 ) ;
#29664 = CIRCLE ( 'NONE', #9467, 2.750000000000000444 ) ;
#29665 = AXIS2_PLACEMENT_3D ( 'NONE', #4835, #16256, #31121 ) ;
#29666 = CARTESIAN_POINT ( 'NONE',  ( 68.00000000000000000, -0.7500000000000000000, -1.988246715074068582 ) ) ;
#29667 = CYLINDRICAL_SURFACE ( 'NONE', #5369, 0.05000000000000002359 ) ;
#29668 = CARTESIAN_POINT ( 'NONE',  ( -54.48531357662248809, 1.514292094527452504, -3.309285685900293927 ) ) ;
#29670 = DIRECTION ( 'NONE',  ( 0.000000000000000000, 0.2008964009354148039, -0.9796124928211139560 ) ) ;
#29669 = CIRCLE ( 'NONE', #21614, 0.1000000000000028644 ) ;
#29671 = ORIENTED_EDGE ( 'NONE', *, *, #21938, .T. ) ;
#29672 = CARTESIAN_POINT ( 'NONE',  ( 52.15659655364830627, 0.5000000000005454526, 1.807104036850122331 ) ) ;
#29673 = AXIS2_PLACEMENT_3D ( 'NONE', #751, #10412, #22159 ) ;
#29674 = AXIS2_PLACEMENT_3D ( 'NONE', #20769, #1121, #13283 ) ;
#29675 = ORIENTED_EDGE ( 'NONE', *, *, #12439, .T. ) ;
#29676 = EDGE_CURVE ( 'NONE', #13776, #7345, #15071, .T. ) ;
#29677 = ORIENTED_EDGE ( 'NONE', *, *, #6459, .T. ) ;
#29678 = CIRCLE ( 'NONE', #16032, 3.000000000000000000 ) ;
#29679 = CIRCLE ( 'NONE', #30677, 0.04999999999999998890 ) ;
#29680 = FACE_OUTER_BOUND ( 'NONE', #9700, .T. ) ;
#29681 = CARTESIAN_POINT ( 'NONE',  ( -59.23542740578359656, -3.725040285533365747, 1.239922660687675871 ) ) ;
#29683 = CARTESIAN_POINT ( 'NONE',  ( -61.35992329370969856, -2.592651747033025700, 0.6797782513837864471 ) ) ;
#29682 = CARTESIAN_POINT ( 'NONE',  ( 15.18463186935387377, 4.683225679163116162, 2.703237727951770086 ) ) ;
#29684 = ORIENTED_EDGE ( 'NONE', *, *, #27266, .T. ) ;
#29685 = ORIENTED_EDGE ( 'NONE', *, *, #935, .F. ) ;
#29686 = CARTESIAN_POINT ( 'NONE',  ( 54.11548297085168713, 5.698162749561729079, -2.050000000000191225 ) ) ;
#29687 = ORIENTED_EDGE ( 'NONE', *, *, #1892, .F. ) ;
#29688 = CARTESIAN_POINT ( 'NONE',  ( 51.70000000000001705, 3.851905453475298113, -1.404572667215154835 ) ) ;
#29689 = VERTEX_POINT ( 'NONE', #21376 ) ;
#29690 = CARTESIAN_POINT ( 'NONE',  ( 28.70703846264934000, 5.747922415052726386, -2.049999999999577938 ) ) ;
#29691 = CARTESIAN_POINT ( 'NONE',  ( -58.06249999999996447, -0.7533615035078129463, 3.673546848079175309 ) ) ;
#29692 = CARTESIAN_POINT ( 'NONE',  ( 51.80000000000001847, 1.734723475976807094E-15, 0.000000000000000000 ) ) ;
#29693 = AXIS2_PLACEMENT_3D ( 'NONE', #10865, #30341, #10715 ) ;
#29694 = AXIS2_PLACEMENT_3D ( 'NONE', #9575, #30333, #8638 ) ;
#29695 = CARTESIAN_POINT ( 'NONE',  ( 15.29449157529455938, -5.068523420888935149, -1.228242390833362618 ) ) ;
#29696 = CARTESIAN_POINT ( 'NONE',  ( -60.51905989232411542, -2.944486372867088697, 1.699999999999773914 ) ) ;
#29697 = CARTESIAN_POINT ( 'NONE',  ( 53.93792434297149185, 7.473468098462470621, -2.050000000000187672 ) ) ;
#29698 = CARTESIAN_POINT ( 'NONE',  ( 47.49593195540760604, -3.900599430603016060, -1.266782962024618708 ) ) ;
#29699 = TOROIDAL_SURFACE ( 'NONE', #4416, 3.299999999999999822, 0.1000000000000000056 ) ;
#29700 = EDGE_CURVE ( 'NONE', #18051, #27277, #16560, .T. ) ;
#29701 = CARTESIAN_POINT ( 'NONE',  ( 48.48449022203101322, 1.386241252175322014, 3.851058308531627450 ) ) ;
#29702 = VECTOR ( 'NONE', #16729, 1000.000000000000000 ) ;
#29704 = VECTOR ( 'NONE', #25525, 1000.000000000000000 ) ;
#29703 = LINE ( 'NONE', #3582, #22598 ) ;
#29706 = EDGE_CURVE ( 'NONE', #11180, #28767, #3909, .T. ) ;
#29705 = DIRECTION ( 'NONE',  ( 1.047444401652940007E-14, 0.000000000000000000, 1.000000000000000000 ) ) ;
#29707 = EDGE_CURVE ( 'NONE', #6274, #17902, #21642, .T. ) ;
#29708 = CARTESIAN_POINT ( 'NONE',  ( -61.36283610645477182, -2.650144964772158218, 0.5164607106961540683 ) ) ;
#29709 = DIRECTION ( 'NONE',  ( 0.7313537016191670181, 0.6819983600625022513, -2.468850131082252327E-15 ) ) ;
#29710 = ORIENTED_EDGE ( 'NONE', *, *, #31306, .T. ) ;
#29711 = AXIS2_PLACEMENT_3D ( 'NONE', #8901, #18130, #1018 ) ;
#29712 = DIRECTION ( 'NONE',  ( -1.000000000000000000, -3.053848253006669023E-16, 2.042510438544995415E-16 ) ) ;
#29713 = VECTOR ( 'NONE', #19313, 1000.000000000000000 ) ;
#29714 = CARTESIAN_POINT ( 'NONE',  ( -36.43290890416665206, -2.776541361170759892, -4.646985486732256199 ) ) ;
#29715 = CARTESIAN_POINT ( 'NONE',  ( 54.41366571437519895, 6.718673005292167488, -1.625000000000181188 ) ) ;
#29716 = ORIENTED_EDGE ( 'NONE', *, *, #20965, .F. ) ;
#29717 = EDGE_CURVE ( 'NONE', #9056, #7143, #24093, .T. ) ;
#29718 = DIRECTION ( 'NONE',  ( -1.189524669241239263E-14, 0.000000000000000000, -1.000000000000000000 ) ) ;
#29719 = VECTOR ( 'NONE', #4917, 1000.000000000000000 ) ;
#29720 = ORIENTED_EDGE ( 'NONE', *, *, #27272, .T. ) ;
#29721 = CARTESIAN_POINT ( 'NONE',  ( 51.76844985144015254, 4.130398687517124579, 1.964667065638868726 ) ) ;
#29722 = CARTESIAN_POINT ( 'NONE',  ( -55.28335481156723574, -4.108500314926510022, 1.367561758111406789 ) ) ;
#29724 = DIRECTION ( 'NONE',  ( -0.000000000000000000, -0.000000000000000000, 1.000000000000000000 ) ) ;
#29723 = CARTESIAN_POINT ( 'NONE',  ( 48.30000000000003268, -0.7901969350669647563, -4.025772098418840983 ) ) ;
#29725 = ORIENTED_EDGE ( 'NONE', *, *, #22253, .T. ) ;
#29726 = CARTESIAN_POINT ( 'NONE',  ( -57.79806624327024878, 3.400000000000002576, 0.9110272542656324690 ) ) ;
#29727 = DIRECTION ( 'NONE',  ( 7.401486830834377462E-15, 0.000000000000000000, 1.000000000000000000 ) ) ;
#29729 = CARTESIAN_POINT ( 'NONE',  ( -60.59999999999997300, -2.421197128371385343, -1.061873357074170077 ) ) ;
#29728 = CARTESIAN_POINT ( 'NONE',  ( 65.00000000000002842, 1.401298464324817071E-42, -6.808388610744111684E-13 ) ) ;
#29730 = DIRECTION ( 'NONE',  ( 3.489354422748178582E-15, -1.218509414717996338E-16, 1.000000000000000000 ) ) ;
#29731 = VERTEX_POINT ( 'NONE', #136 ) ;
#29732 = CARTESIAN_POINT ( 'NONE',  ( -59.37499999999997158, -3.673546848079174421, -0.7533615035078058408 ) ) ;
#29733 = CARTESIAN_POINT ( 'NONE',  ( -56.18749999999997868, -3.399999999999991029, -2.152687225432237971E-13 ) ) ;
#29734 = EDGE_CURVE ( 'NONE', #518, #12299, #6422, .T. ) ;
#29735 = CARTESIAN_POINT ( 'NONE',  ( 58.66118217212530794, 1.615348343402911446, -0.9521303665439364572 ) ) ;
#29736 = CARTESIAN_POINT ( 'NONE',  ( -54.49999999999997868, -2.351239121950967181, -2.690277294116418361 ) ) ;
#29737 = DIRECTION ( 'NONE',  ( 0.000000000000000000, 0.000000000000000000, -1.000000000000000000 ) ) ;
#29738 = CARTESIAN_POINT ( 'NONE',  ( -55.44702994616206126, -2.078460969082657872, 3.599999999999794920 ) ) ;
#29739 = DIRECTION ( 'NONE',  ( 0.000000000000000000, -1.000000000000000000, 0.000000000000000000 ) ) ;
#29740 = ORIENTED_EDGE ( 'NONE', *, *, #6388, .F. ) ;
#29741 = CIRCLE ( 'NONE', #22169, 0.1000000000000000472 ) ;
#29742 = EDGE_CURVE ( 'NONE', #489, #24382, #12006, .T. ) ;
#29743 = CARTESIAN_POINT ( 'NONE',  ( 15.22780280894163241, 2.525801254963248699, 4.794550361020370133 ) ) ;
#29744 = EDGE_CURVE ( 'NONE', #9733, #27521, #4900, .T. ) ;
#29745 =( BOUNDED_CURVE ( )  B_SPLINE_CURVE ( 3, ( #27909, #15728, #3680, #13319 ),
 .UNSPECIFIED., .F., .T. ) 
 B_SPLINE_CURVE_WITH_KNOTS ( ( 4, 4 ),
 ( 4.816328208040331127, 4.921019051201621863 ),
 .UNSPECIFIED. ) 
 CURVE ( )  GEOMETRIC_REPRESENTATION_ITEM ( )  RATIONAL_B_SPLINE_CURVE ( ( 1.000000000000000000, 0.9990868608118155247, 0.9990868608118155247, 1.000000000000000000 ) ) 
 REPRESENTATION_ITEM ( '' )  );
#29746 = EDGE_CURVE ( 'NONE', #19238, #11901, #2567, .T. ) ;
#29747 = DIRECTION ( 'NONE',  ( 1.000000000000000000, 1.047444401652940007E-14, 0.000000000000000000 ) ) ;
#29748 = DIRECTION ( 'NONE',  ( 1.000000000000000000, -1.219044193948983948E-29, 3.491481338843133355E-15 ) ) ;
#29749 = CARTESIAN_POINT ( 'NONE',  ( -36.22818246778845719, 4.895960019030868082, -2.323379425334441084 ) ) ;
#29750 = CARTESIAN_POINT ( 'NONE',  ( 51.59739104186226655, 1.165722629542050193, -1.468576096419531352 ) ) ;
#29751 = FACE_OUTER_BOUND ( 'NONE', #7619, .T. ) ;
#29752 = ORIENTED_EDGE ( 'NONE', *, *, #10979, .F. ) ;
#29753 = DIRECTION ( 'NONE',  ( -3.696862594069181415E-15, -0.9356455129756988676, -0.3529411764705864263 ) ) ;
#29754 = ORIENTED_EDGE ( 'NONE', *, *, #26976, .T. ) ;
#29755 = CARTESIAN_POINT ( 'NONE',  ( 50.30000000000001847, -1.426739617975173013, 3.843750000000023093 ) ) ;
#29757 = DIRECTION ( 'NONE',  ( -0.000000000000000000, -0.000000000000000000, 1.000000000000000000 ) ) ;
#29756 = CARTESIAN_POINT ( 'NONE',  ( 57.03907689491666844, 0.7490795634100378964, -2.421870079683545285 ) ) ;
#29758 = VERTEX_POINT ( 'NONE', #22302 ) ;
#29759 = VECTOR ( 'NONE', #28511, 1000.000000000000000 ) ;
#29760 = ORIENTED_EDGE ( 'NONE', *, *, #27412, .T. ) ;
#29761 = DIRECTION ( 'NONE',  ( -2.581436205204234499E-16, 0.9796124928211140670, 0.2008964009354147762 ) ) ;
#29762 = AXIS2_PLACEMENT_3D ( 'NONE', #14717, #24379, #12195 ) ;
#29763 = CARTESIAN_POINT ( 'NONE',  ( 28.63101374161908907, 6.274379892050022001, 1.424999999999899458 ) ) ;
#29764 = ORIENTED_EDGE ( 'NONE', *, *, #18892, .F. ) ;
#29766 = CARTESIAN_POINT ( 'NONE',  ( 51.76087627324522344, -4.170474612306438011, 1.019817338724548383 ) ) ;
#29765 = CARTESIAN_POINT ( 'NONE',  ( -57.57202994616204705, -4.156921938165296204, -2.193920212522006445E-13 ) ) ;
#29767 = CARTESIAN_POINT ( 'NONE',  ( -54.79792740578361077, -2.256877952708263191, 2.542931754211923856 ) ) ;
#29768 = EDGE_CURVE ( 'NONE', #10001, #2526, #4404, .T. ) ;
#29769 = DIRECTION ( 'NONE',  ( 1.000000000000000000, 0.000000000000000000, -0.000000000000000000 ) ) ;
#29770 = CARTESIAN_POINT ( 'NONE',  ( 58.74999981196286569, -1.321459237640645767, -1.441661833134718407 ) ) ;
#29771 = EDGE_CURVE ( 'NONE', #14732, #16720, #30872, .T. ) ;
#29772 = ORIENTED_EDGE ( 'NONE', *, *, #29901, .F. ) ;
#29773 = DIRECTION ( 'NONE',  ( 0.000000000000000000, 0.000000000000000000, -1.000000000000000000 ) ) ;
#29774 = CARTESIAN_POINT ( 'NONE',  ( 53.71202192472753012, 7.447163568589559191, -2.050000000000249401 ) ) ;
#29775 = DIRECTION ( 'NONE',  ( -1.000000000000000000, -3.053848253006669023E-16, 2.042510438544995415E-16 ) ) ;
#29776 = FACE_OUTER_BOUND ( 'NONE', #11890, .T. ) ;
#29777 = ADVANCED_FACE ( 'NONE', ( #918 ), #17373, .T. ) ;
#29778 = PRESENTATION_LAYER_ASSIGNMENT (  '', '', ( #21721 ) ) ;
#29779 = CARTESIAN_POINT ( 'NONE',  ( -54.72099364905386665, -3.399999999999994138, 0.9110272542656107087 ) ) ;
#29780 = AXIS2_PLACEMENT_3D ( 'NONE', #26804, #5253, #24421 ) ;
#29782 = CARTESIAN_POINT ( 'NONE',  ( 58.75000000000004263, -1.932246131436200942, -0.4087173687850521042 ) ) ;
#29781 = CARTESIAN_POINT ( 'NONE',  ( 30.08242191457676995, 7.215531071606934965, -1.425000000000104849 ) ) ;
#29783 = PRODUCT_DEFINITION_SHAPE ( 'NONE', 'NONE',  #6040 ) ;
#29784 = CARTESIAN_POINT ( 'NONE',  ( -62.09962743728070933, -2.519971547655114108, 0.1593117589168163151 ) ) ;
#29785 = DIRECTION ( 'NONE',  ( -1.000000000000000000, -3.053848253006669023E-16, 2.042510438544995415E-16 ) ) ;
#29787 = CARTESIAN_POINT ( 'NONE',  ( -54.49999999999999289, 2.184125401144869194, -2.774890241360551624 ) ) ;
#29786 = CARTESIAN_POINT ( 'NONE',  ( 58.66107449606992219, 1.819875603894975491, -0.4525291603547138553 ) ) ;
#29788 = ORIENTED_EDGE ( 'NONE', *, *, #27741, .F. ) ;
#29789 = LINE ( 'NONE', #8104, #25053 ) ;
#29790 = DIRECTION ( 'NONE',  ( 1.000000000000000000, 3.053848253006669023E-16, -2.042510438544995415E-16 ) ) ;
#29791 = AXIS2_PLACEMENT_3D ( 'NONE', #25416, #22755, #13218 ) ;
#29793 = CARTESIAN_POINT ( 'NONE',  ( 65.00000000000001421, -1.025519176787267142E-28, -6.808388610744108654E-13 ) ) ;
#29792 = CARTESIAN_POINT ( 'NONE',  ( 15.48609859788814980, 3.148602930107248898, -4.139959549308847464 ) ) ;
#29794 = CARTESIAN_POINT ( 'NONE',  ( 57.03821272586434787, 0.7500000328843418052, 2.490438846756156899 ) ) ;
#29795 = ORIENTED_EDGE ( 'NONE', *, *, #18069, .F. ) ;
#29796 = CARTESIAN_POINT ( 'NONE',  ( -61.39046581447303197, -2.653474656127174924, 0.4959525385592167823 ) ) ;
#29797 = CARTESIAN_POINT ( 'NONE',  ( 50.55258015808398397, 5.293720379222080095E-13, -1.177580158083963546 ) ) ;
#29798 = CIRCLE ( 'NONE', #22747, 2.525000000000001243 ) ;
#29799 = ORIENTED_EDGE ( 'NONE', *, *, #15215, .F. ) ;
#29800 = CARTESIAN_POINT ( 'NONE',  ( 16.10667815269233216, -5.187083072802361805, 1.534568794951160609 ) ) ;
#29801 = VERTEX_POINT ( 'NONE', #2973 ) ;
#29802 = VERTEX_POINT ( 'NONE', #19770 ) ;
#29803 = EDGE_CURVE ( 'NONE', #17369, #91, #8446, .T. ) ;
#29804 = CARTESIAN_POINT ( 'NONE',  ( 15.48686146417451326, 4.979756346315124205, 1.501439362221289597 ) ) ;
#29805 = CARTESIAN_POINT ( 'NONE',  ( 58.66133336607637716, 1.607522887372764941, -0.9657121834148668649 ) ) ;
#29806 = STYLED_ITEM ( 'NONE', ( #19039 ), #12719 ) ;
#29807 = ORIENTED_EDGE ( 'NONE', *, *, #30042, .F. ) ;
#29808 = EDGE_CURVE ( 'NONE', #23361, #26099, #12302, .T. ) ;
#29809 = CARTESIAN_POINT ( 'NONE',  ( 51.96434559586250401, 4.380380852615003207, -1.404523007340313212 ) ) ;
#29810 = VECTOR ( 'NONE', #25667, 1000.000000000000000 ) ;
#29811 = CARTESIAN_POINT ( 'NONE',  ( -60.63452994616204705, -3.117691453623976816, 1.799999999999772671 ) ) ;
#29812 = ORIENTED_EDGE ( 'NONE', *, *, #10793, .F. ) ;
#29813 = CARTESIAN_POINT ( 'NONE',  ( -59.69464122902330416, 2.086944863889884871, 1.740854861534822273 ) ) ;
#29814 = DIRECTION ( 'NONE',  ( 0.000000000000000000, -0.9996898646859343485, -0.02490330187381123786 ) ) ;
#29815 = CARTESIAN_POINT ( 'NONE',  ( 22.61091062455514589, 6.637672123835637983, 1.949999999999954214 ) ) ;
#29816 = ORIENTED_EDGE ( 'NONE', *, *, #3407, .T. ) ;
#29817 = AXIS2_PLACEMENT_3D ( 'NONE', #9257, #3708, #1335 ) ;
#29818 = CARTESIAN_POINT ( 'NONE',  ( -54.74999999999997868, -2.944486372867089141, 1.699999999999794342 ) ) ;
#29819 = CARTESIAN_POINT ( 'NONE',  ( -57.22499999999997300, 0.9241234443029110457, -4.506217466977124886 ) ) ;
#29820 = CARTESIAN_POINT ( 'NONE',  ( 54.41366571437520605, 6.718673005292168376, -1.950000000000180256 ) ) ;
#29821 = FACE_OUTER_BOUND ( 'NONE', #18617, .T. ) ;
#29822 = CARTESIAN_POINT ( 'NONE',  ( 15.03925126672132961, -3.426725943139564912, 3.937891353488729429 ) ) ;
#29823 = EDGE_CURVE ( 'NONE', #29022, #590, #22621, .T. ) ;
#29825 = CARTESIAN_POINT ( 'NONE',  ( -54.68749999999997868, 0.7533615035078081723, -3.673546848079177973 ) ) ;
#29824 = LINE ( 'NONE', #27446, #1859 ) ;
#29826 = CARTESIAN_POINT ( 'NONE',  ( -59.19999999999997442, 8.366749974758448157E-15, -2.103076948839454410E-13 ) ) ;
#29827 = CARTESIAN_POINT ( 'NONE',  ( -55.81249999999997868, -0.7533615035078013999, 3.673546848079176641 ) ) ;
#29828 = VECTOR ( 'NONE', #11037, 1000.000000000000000 ) ;
#29829 = B_SPLINE_CURVE_WITH_KNOTS ( 'NONE', 3,
 ( #27556, #10634, #982, #22981, #5722, #10482, #29787, #13608, #20460, #8704, #25196, #23149, #1267, #5885, #6192, #17918, #18388, #6340 ),
 .UNSPECIFIED., .F., .F.,
 ( 4, 2, 2, 2, 2, 2, 2, 2, 4 ),
 ( 0.000000000000000000, 0.0007552462382147887140, 0.001510492476429577428, 0.002265738714644366034, 0.003020984952859154856, 0.003776231191073943678, 0.004531477429288733802, 0.005286723667503522191, 0.006041969905718312314 ),
 .UNSPECIFIED. ) ;
#29830 = CARTESIAN_POINT ( 'NONE',  ( 58.74999999305994436, 1.345908541130588221, -1.382203543031251813 ) ) ;
#29831 = LINE ( 'NONE', #22874, #12955 ) ;
#29832 = ORIENTED_EDGE ( 'NONE', *, *, #12025, .F. ) ;
#29833 = CARTESIAN_POINT ( 'NONE',  ( -54.49983832461118283, 1.542920080254278181, 3.327619142904491234 ) ) ;
#29834 = CIRCLE ( 'NONE', #19288, 2.000000000000000000 ) ;
#29835 = VERTEX_POINT ( 'NONE', #7714 ) ;
#29836 = EDGE_LOOP ( 'NONE', ( #19080, #9062, #8264, #23824 ) ) ;
#29837 = CARTESIAN_POINT ( 'NONE',  ( -59.10047575464341207, 2.308863783365080913, 1.300633787035090361 ) ) ;
#29838 = CARTESIAN_POINT ( 'NONE',  ( -59.36042740578360366, -0.7887156198831606346, 3.845940847736174284 ) ) ;
#29840 = CARTESIAN_POINT ( 'NONE',  ( -59.51187924496046833, 2.330100891901230487, 1.424301819445882744 ) ) ;
#29839 = CARTESIAN_POINT ( 'NONE',  ( -57.12499999999997868, -3.920666489018328579E-15, 3.399999999999796518 ) ) ;
#29841 = ORIENTED_EDGE ( 'NONE', *, *, #324, .F. ) ;
#29842 = ORIENTED_EDGE ( 'NONE', *, *, #23212, .T. ) ;
#29843 = DIRECTION ( 'NONE',  ( 2.614375865348240525E-16, -0.2008964009354147762, 0.9796124928211140670 ) ) ;
#29844 = VERTEX_POINT ( 'NONE', #3123 ) ;
#29845 = ADVANCED_FACE ( 'NONE', ( #19623 ), #2377, .T. ) ;
#29846 = CARTESIAN_POINT ( 'NONE',  ( 51.79999999999973426, 3.849999999998453770, -1.627286622740575339 ) ) ;
#29847 = ORIENTED_EDGE ( 'NONE', *, *, #4744, .T. ) ;
#29848 = CARTESIAN_POINT ( 'NONE',  ( 27.81683722849682638, 5.540920426342174743, -2.050000000000097078 ) ) ;
#29849 = CARTESIAN_POINT ( 'NONE',  ( -57.26905989232410832, 2.356882582050587835E-14, -3.400000000000203304 ) ) ;
#29850 = DIRECTION ( 'NONE',  ( 0.000000000000000000, 0.000000000000000000, -1.000000000000000000 ) ) ;
#29851 = EDGE_LOOP ( 'NONE', ( #7367, #21232, #13380, #30596 ) ) ;
#29852 = CARTESIAN_POINT ( 'NONE',  ( 16.10705563471231372, -5.191204783933229372, -1.522159526382844907 ) ) ;
#29853 = CARTESIAN_POINT ( 'NONE',  ( -57.26905989232410832, 2.023778652682507790E-14, -3.400000000000203304 ) ) ;
#29854 = CARTESIAN_POINT ( 'NONE',  ( 47.38141046868508965, -3.967542327744154829, 1.366354831956431370 ) ) ;
#29855 = CARTESIAN_POINT ( 'NONE',  ( 47.21128518863328338, -3.753741921856249331, -1.652517360674314206 ) ) ;
#29856 = AXIS2_PLACEMENT_3D ( 'NONE', #9804, #4890, #2198 ) ;
#29857 = EDGE_CURVE ( 'NONE', #15552, #10800, #18039, .T. ) ;
#29858 = DIRECTION ( 'NONE',  ( 1.047444401652940007E-14, 0.000000000000000000, 1.000000000000000000 ) ) ;
#29859 = LINE ( 'NONE', #24643, #30147 ) ;
#29861 = CARTESIAN_POINT ( 'NONE',  ( 34.56702326949724835, 8.213851659285209550, -1.950000000000119860 ) ) ;
#29860 = CARTESIAN_POINT ( 'NONE',  ( 61.00000000000002132, 6.389410850082937196E-13, 3.111507638930570854E-58 ) ) ;
#29862 = DIRECTION ( 'NONE',  ( -1.000000000000000000, 0.000000000000000000, 1.047444401652940007E-14 ) ) ;
#29863 = FACE_OUTER_BOUND ( 'NONE', #11699, .T. ) ;
#29864 =( BOUNDED_SURFACE ( )  B_SPLINE_SURFACE ( 3, 2, ( 
 ( #8902, #18899, #19225 ),
 ( #2098, #13795, #16206 ),
 ( #28542, #20957, #23658 ),
 ( #6852, #23807, #30589 ),
 ( #18589, #6544, #21438 ),
 ( #28866, #25854, #1951 ),
 ( #23478, #19061, #30765 ),
 ( #1772, #28715, #5103 ),
 ( #7776, #22057, #29461 ),
 ( #5413, #652, #353 ),
 ( #17152, #22216, #19980 ),
 ( #12230, #26646, #16994 ),
 ( #24114, #19688, #24415 ),
 ( #14754, #17444, #9854 ),
 ( #17294, #21913, #505 ),
 ( #2724, #12368, #16840 ) ),
 .UNSPECIFIED., .F., .F., .F. ) 
 B_SPLINE_SURFACE_WITH_KNOTS ( ( 4, 2, 2, 2, 2, 2, 2, 4 ),
 ( 3, 3 ),
 ( 0.001780502285214183430, 0.002558945925323759425, 0.002753556835351153587, 0.002948167745378547314, 0.003337389565433335203, 0.003726611385488123093, 0.004115833205542910982, 0.004894276845652486760 ),
 ( 0.000000000000000000, 1.000000000000000000 ),
 .UNSPECIFIED. ) 
 GEOMETRIC_REPRESENTATION_ITEM ( )  RATIONAL_B_SPLINE_SURFACE ( (
 ( 1.000000000000000000, 0.9418517008537252710, 1.000000000000000000),
 ( 1.000000000000000000, 0.9417987965885095125, 1.000000000000000000),
 ( 1.000000000000000000, 0.9418198861734097260, 1.000000000000000000),
 ( 1.000000000000000000, 0.9434060303845585027, 1.000000000000000000),
 ( 1.000000000000000000, 0.9437939819948245601, 1.000000000000000000),
 ( 1.000000000000000000, 0.9445989566712741370, 1.000000000000000000),
 ( 1.000000000000000000, 0.9450169930050026368, 1.000000000000000000),
 ( 1.000000000000000000, 0.9461610507673267056, 1.000000000000000000),
 ( 1.000000000000000000, 0.9467217966427221576, 1.000000000000000000),
 ( 1.000000000000000000, 0.9467345476124371384, 1.000000000000000000),
 ( 1.000000000000000000, 0.9461964028052947118, 1.000000000000000000),
 ( 1.000000000000000000, 0.9446801822473851473, 1.000000000000000000),
 ( 1.000000000000000000, 0.9437582546536329442, 1.000000000000000000),
 ( 1.000000000000000000, 0.9418129560296130132, 1.000000000000000000),
 ( 1.000000000000000000, 0.9418016889777165446, 1.000000000000000000),
 ( 1.000000000000000000, 0.9418517008537247159, 1.000000000000000000) ) ) 
 REPRESENTATION_ITEM ( '' )  SURFACE ( )  );
#29865 = FACE_OUTER_BOUND ( 'NONE', #6876, .T. ) ;
#29866 = ORIENTED_EDGE ( 'NONE', *, *, #5040, .T. ) ;
#29867 = B_SPLINE_CURVE_WITH_KNOTS ( 'NONE', 3,
 ( #18077, #23290, #11233, #20909 ),
 .UNSPECIFIED., .F., .F.,
 ( 4, 4 ),
 ( 5.935267624065755708E-05, 0.0002061672048306634642 ),
 .UNSPECIFIED. ) ;
#29868 = EDGE_CURVE ( 'NONE', #29651, #12157, #20089, .T. ) ;
#29869 = DIRECTION ( 'NONE',  ( 0.000000000000000000, 0.000000000000000000, 1.000000000000000000 ) ) ;
#29870 = CARTESIAN_POINT ( 'NONE',  ( 54.41366571437519895, 6.718673005292166600, -1.856154119295183591E-13 ) ) ;
#29871 = EDGE_LOOP ( 'NONE', ( #7762, #9129, #9543, #19211 ) ) ;
#29872 = CARTESIAN_POINT ( 'NONE',  ( -59.19495429951913223, -2.548385458854336871, -0.9469503383366065785 ) ) ;
#29873 = EDGE_LOOP ( 'NONE', ( #6836, #27396, #28761, #15429 ) ) ;
#29874 = CARTESIAN_POINT ( 'NONE',  ( 58.65000000000001990, 6.143261415694495821E-13, 3.111507638930570854E-58 ) ) ;
#29875 = DIRECTION ( 'NONE',  ( 1.000000000000000000, 1.047444401652940007E-14, 0.000000000000000000 ) ) ;
#29876 = CIRCLE ( 'NONE', #28369, 0.05000000000000008604 ) ;
#29878 = LINE ( 'NONE', #22616, #29828 ) ;
#29877 = FACE_OUTER_BOUND ( 'NONE', #16098, .T. ) ;
#29879 = VERTEX_POINT ( 'NONE', #17232 ) ;
#29880 = CARTESIAN_POINT ( 'NONE',  ( -35.85663232820584057, -0.9159215771353976798, -4.311190327365980401 ) ) ;
#29881 = AXIS2_PLACEMENT_3D ( 'NONE', #10420, #5830, #22165 ) ;
#29882 = ADVANCED_FACE ( 'NONE', ( #29877 ), #5170, .T. ) ;
#29883 = CARTESIAN_POINT ( 'NONE',  ( 68.00000000000001421, 3.252606517456513302E-16, -7.122621931239992550E-13 ) ) ;
#29884 = ORIENTED_EDGE ( 'NONE', *, *, #4116, .T. ) ;
#29886 = FACE_OUTER_BOUND ( 'NONE', #13228, .T. ) ;
#29885 = CARTESIAN_POINT ( 'NONE',  ( 51.94586206790092575, 3.919599533071086661, 2.045267139815340585 ) ) ;
#29887 = DIRECTION ( 'NONE',  ( 0.000000000000000000, 0.000000000000000000, -1.000000000000000000 ) ) ;
#29888 = VERTEX_POINT ( 'NONE', #8500 ) ;
#29889 = CARTESIAN_POINT ( 'NONE',  ( 50.75360625943720549, -0.3719558471739982108, 1.344678919698702568 ) ) ;
#29890 = CARTESIAN_POINT ( 'NONE',  ( -62.29999999999998295, 1.106939637198029038E-15, 2.238576962872695299E-15 ) ) ;
#29891 = CARTESIAN_POINT ( 'NONE',  ( 58.75000018803716983, 1.701355787207877501, -0.9251739982193851741 ) ) ;
#29892 = CARTESIAN_POINT ( 'NONE',  ( -36.92398358572908990, -3.410993390446888096, 4.205682099886847602 ) ) ;
#29893 = CARTESIAN_POINT ( 'NONE',  ( -62.06710100716625789, -2.624587610216423172, -0.3274367013645053115 ) ) ;
#29894 = CARTESIAN_POINT ( 'NONE',  ( -54.82202994616206126, 2.078460969082646770, 3.599999999999812683 ) ) ;
#29895 = VERTEX_POINT ( 'NONE', #16104 ) ;
#29896 = AXIS2_PLACEMENT_3D ( 'NONE', #12923, #18179, #29546 ) ;
#29897 = EDGE_CURVE ( 'NONE', #27932, #24984, #11184, .T. ) ;
#29898 = CARTESIAN_POINT ( 'NONE',  ( 15.95705409078442294, -2.672993279333548688, 4.702725322014869924 ) ) ;
#29899 = DIRECTION ( 'NONE',  ( 0.000000000000000000, 0.4102564102564100201, -0.9119702176296790030 ) ) ;
#29900 = FACE_OUTER_BOUND ( 'NONE', #13984, .T. ) ;
#29901 = EDGE_CURVE ( 'NONE', #22384, #27011, #5425, .T. ) ;
#29902 = CARTESIAN_POINT ( 'NONE',  ( -57.38452994616203284, 2.446306557613808189E-14, -3.600000000000203926 ) ) ;
#29903 = CARTESIAN_POINT ( 'NONE',  ( 58.65000000000004121, -1.872332544500628915, 0.09997921184680889917 ) ) ;
#29904 = ORIENTED_EDGE ( 'NONE', *, *, #16997, .F. ) ;
#29905 = AXIS2_PLACEMENT_3D ( 'NONE', #11644, #21322, #30952 ) ;
#29906 = CARTESIAN_POINT ( 'NONE',  ( -35.85663232820584057, -4.804073783693452171, -2.042134687550364092 ) ) ;
#29907 = EDGE_LOOP ( 'NONE', ( #21002, #5477, #2117, #30608 ) ) ;
#29908 = CARTESIAN_POINT ( 'NONE',  ( -59.10063086800197851, 2.465840246069578523, -0.9706348447806306678 ) ) ;
#29910 = CARTESIAN_POINT ( 'NONE',  ( 47.10000000000002984, -3.637377585518695611, 2.099877210782872261 ) ) ;
#29909 = CARTESIAN_POINT ( 'NONE',  ( -54.49542095125566732, -2.304164661794668945, -2.707651631953783333 ) ) ;
#29911 = ORIENTED_EDGE ( 'NONE', *, *, #18414, .T. ) ;
#29912 = VERTEX_POINT ( 'NONE', #3596 ) ;
#29913 = CARTESIAN_POINT ( 'NONE',  ( -59.28559899066483041, 3.161828374300069466, 1.250136525132556020 ) ) ;
#29914 = AXIS2_PLACEMENT_3D ( 'NONE', #3922, #23252, #30203 ) ;
#29915 = ADVANCED_FACE ( 'NONE', ( #30020 ), #25123, .F. ) ;
#29916 = DIRECTION ( 'NONE',  ( 0.000000000000000000, 0.9996898646859344595, 0.02490330187381124133 ) ) ;
#29917 = VERTEX_POINT ( 'NONE', #3903 ) ;
#29919 = FACE_OUTER_BOUND ( 'NONE', #12384, .T. ) ;
#29918 = CARTESIAN_POINT ( 'NONE',  ( -58.00952994616203284, 3.117691453623994580, -1.800000000000192557 ) ) ;
#29920 = CARTESIAN_POINT ( 'NONE',  ( -58.92292740578360366, 2.256877952708268964, -2.542931754211924744 ) ) ;
#29921 = ADVANCED_FACE ( 'NONE', ( #5813 ), #3453, .F. ) ;
#29922 = DIRECTION ( 'NONE',  ( 0.000000000000000000, 0.2008964009354143876, -0.9796124928211140670 ) ) ;
#29923 = SHAPE_REPRESENTATION ( 'Twister Head', ( #9018 ), #15625 ) ;
#29924 = DIRECTION ( 'NONE',  ( 1.000000000000000000, 0.000000000000000000, 0.000000000000000000 ) ) ;
#29925 = CARTESIAN_POINT ( 'NONE',  ( 58.72204580543404262, -1.341784641881615725, -1.309860786662260024 ) ) ;
#29926 =( BOUNDED_SURFACE ( )  B_SPLINE_SURFACE ( 3, 2, ( 
 ( #3608, #3750, #10261 ),
 ( #3464, #20409, #5669 ),
 ( #755, #25444, #19932 ),
 ( #8349, #25296, #30199 ),
 ( #5827, #10417, #29735 ),
 ( #8048, #5515, #7878 ),
 ( #29891, #8202, #17718 ),
 ( #8514, #1216, #15484 ),
 ( #18024, #13243, #13099 ),
 ( #27360, #24968, #27676 ) ),
 .UNSPECIFIED., .F., .F., .F. ) 
 B_SPLINE_SURFACE_WITH_KNOTS ( ( 4, 2, 2, 2, 4 ),
 ( 3, 3 ),
 ( 0.0001706658715691184651, 0.0002229276920778214721, 0.0002751895125865245063, 0.0003274513330952275405, 0.0003797131536039305747 ),
 ( 0.000000000000000000, 1.000000000000000000 ),
 .UNSPECIFIED. ) 
 GEOMETRIC_REPRESENTATION_ITEM ( )  RATIONAL_B_SPLINE_SURFACE ( (
 ( 1.000000000000000000, 0.7071067811865455743, 1.000000000000000000),
 ( 1.000000000000000000, 0.7375607040701674944, 1.000000000000000000),
 ( 1.000000000000000000, 0.7730431127431096616, 1.000000000000000000),
 ( 1.000000000000000000, 0.8321012486992810375, 1.000000000000000000),
 ( 1.000000000000000000, 0.8541932017417851464, 1.000000000000000000),
 ( 1.000000000000000000, 0.8545723906072691944, 1.000000000000000000),
 ( 1.000000000000000000, 0.8327032135053918926, 1.000000000000000000),
 ( 1.000000000000000000, 0.7734559727069735269, 1.000000000000000000),
 ( 1.000000000000000000, 0.7377766653994330959, 1.000000000000000000),
 ( 1.000000000000000000, 0.7071067811865439090, 1.000000000000000000) ) ) 
 REPRESENTATION_ITEM ( '' )  SURFACE ( )  );
#29927 = EDGE_LOOP ( 'NONE', ( #28794, #17456, #24243, #5949, #29568, #25074, #11584, #27058, #1401, #2849, #26202, #28686, #21052, #23983, #5156, #12585, #26093, #11214, #5287, #15177, #26035, #14680, #26904, #26387, #30050, #7648, #19787, #17363, #382, #17976, #8153, #14767 ) ) ;
#29928 = EDGE_CURVE ( 'NONE', #24531, #8907, #12483, .T. ) ;
#29929 = CARTESIAN_POINT ( 'NONE',  ( 47.00970077834632121, -4.153760649298012808, -1.055564289358534635 ) ) ;
#29930 = CARTESIAN_POINT ( 'NONE',  ( 53.89553379148919277, 6.017104844469294278, -2.050000000000187228 ) ) ;
#29931 = CARTESIAN_POINT ( 'NONE',  ( 48.43418025728714582, -1.399739523915389583, -3.853780793998481169 ) ) ;
#29932 = VECTOR ( 'NONE', #24184, 1000.000000000000000 ) ;
#29933 = CARTESIAN_POINT ( 'NONE',  ( 16.10624235918717417, -0.1627367787821556444, 5.407318510437581160 ) ) ;
#29934 = CARTESIAN_POINT ( 'NONE',  ( 57.04707324256202128, -0.7500000000000492939, -2.421260002560643443 ) ) ;
#29936 = CARTESIAN_POINT ( 'NONE',  ( 58.66122797211827589, -1.806862593128205630, -0.5011487553405924444 ) ) ;
#29935 = DIRECTION ( 'NONE',  ( 0.000000000000000000, 0.000000000000000000, 1.000000000000000000 ) ) ;
#29937 = ADVANCED_FACE ( 'NONE', ( #18481 ), #22775, .T. ) ;
#29938 = DIRECTION ( 'NONE',  ( 1.000000000000000000, 3.054025858079668409E-16, -2.042474015755241579E-16 ) ) ;
#29939 = DIRECTION ( 'NONE',  ( 0.000000000000000000, -0.3333333333333488580, -0.9428090415820578052 ) ) ;
#29941 = CARTESIAN_POINT ( 'NONE',  ( -54.49999999999999289, -1.600000000000004530, 3.363870538531237298 ) ) ;
#29940 = CARTESIAN_POINT ( 'NONE',  ( -45.15971931043468146, -4.700000000000000178, 5.808909232612072777E-16 ) ) ;
#29942 = EDGE_LOOP ( 'NONE', ( #25676, #25207, #25838, #29074 ) ) ;
#29943 = CARTESIAN_POINT ( 'NONE',  ( 50.25000000000003553, -1.323060376181892872, 1.499837071478349326 ) ) ;
#29944 = ADVANCED_FACE ( 'NONE', ( #8337 ), #22917, .T. ) ;
#29945 = CARTESIAN_POINT ( 'NONE',  ( -36.89831264271880684, 2.941172302009069206, -4.539591111929616396 ) ) ;
#29946 = VECTOR ( 'NONE', #14009, 1000.000000000000114 ) ;
#29948 = CARTESIAN_POINT ( 'NONE',  ( -59.63821477905805324, -2.352792697908255182, -1.234285180173736451 ) ) ;
#29947 = DIRECTION ( 'NONE',  ( 1.000000000000000000, -0.000000000000000000, -1.047444401652940007E-14 ) ) ;
#29949 = DIRECTION ( 'NONE',  ( 1.000000000000000000, 0.000000000000000000, 0.000000000000000000 ) ) ;
#29950 = VERTEX_POINT ( 'NONE', #6132 ) ;
#29951 = CARTESIAN_POINT ( 'NONE',  ( 52.02336772807330334, 3.827384603151627207, 2.049999999999818190 ) ) ;
#29952 = CARTESIAN_POINT ( 'NONE',  ( -60.61395381780661751, -2.454888324004492972, -1.087441295755433579 ) ) ;
#29953 = ORIENTED_EDGE ( 'NONE', *, *, #12892, .F. ) ;
#29954 = ADVANCED_FACE ( 'NONE', ( #18182, #1206 ), #20554, .T. ) ;
#29955 = CARTESIAN_POINT ( 'NONE',  ( 51.18805119203790355, 0.9696852903241819366, -1.451974857136960395 ) ) ;
#29956 = ORIENTED_EDGE ( 'NONE', *, *, #16946, .T. ) ;
#29957 = EDGE_CURVE ( 'NONE', #16445, #3208, #27963, .T. ) ;
#29958 = CARTESIAN_POINT ( 'NONE',  ( 16.10667815269233216, 3.294441450831234075, -4.290383166762102185 ) ) ;
#29959 = DIRECTION ( 'NONE',  ( 0.000000000000000000, 1.000000000000000000, 0.000000000000000000 ) ) ;
#29960 = VERTEX_POINT ( 'NONE', #30486 ) ;
#29961 = CARTESIAN_POINT ( 'NONE',  ( -73.90999999999998238, -2.438578184542714499E-15, 4.609931582023435380E-15 ) ) ;
#29962 = CARTESIAN_POINT ( 'NONE',  ( -54.76905989232412963, 2.944486372867092250, 1.699999999999816769 ) ) ;
#29963 = ORIENTED_EDGE ( 'NONE', *, *, #6941, .T. ) ;
#29964 = CARTESIAN_POINT ( 'NONE',  ( 57.00357781822870606, 0.7683521053270409018, -1.737709711729638729 ) ) ;
#29965 = CARTESIAN_POINT ( 'NONE',  ( 61.25000000000000711, 1.470078920828157498, -1.320078920826817992 ) ) ;
#29966 = CARTESIAN_POINT ( 'NONE',  ( 23.88937650878824925, 5.720041404659278683, 2.049999999999714717 ) ) ;
#29967 = VERTEX_POINT ( 'NONE', #8789 ) ;
#29968 = CARTESIAN_POINT ( 'NONE',  ( -55.74999999999997868, 2.944486372867092250, 1.699999999999813438 ) ) ;
#29969 = CARTESIAN_POINT ( 'NONE',  ( 60.75000000000001421, 0.5000000000006363798, -1.546164609606622831 ) ) ;
#29970 = CARTESIAN_POINT ( 'NONE',  ( 51.90000000000001279, 1.734723475976807094E-15, 0.000000000000000000 ) ) ;
#29971 = CARTESIAN_POINT ( 'NONE',  ( 47.06312566212015724, 8.366466760780054912, -2.050000000000163691 ) ) ;
#29972 = DIRECTION ( 'NONE',  ( 0.000000000000000000, -4.336808689942006692E-15, 1.000000000000000000 ) ) ;
#29973 = ADVANCED_FACE ( 'NONE', ( #28764 ), #11508, .T. ) ;
#29974 = CARTESIAN_POINT ( 'NONE',  ( -54.44999999999997442, 0.000000000000000000, 4.299999999999998046 ) ) ;
#29975 = FACE_OUTER_BOUND ( 'NONE', #19452, .T. ) ;
#29976 = ADVANCED_FACE ( 'NONE', ( #11813 ), #28287, .T. ) ;
#29977 = CARTESIAN_POINT ( 'NONE',  ( 58.75000000000003553, -1.760622601995821102, 0.8948927608039443093 ) ) ;
#29978 = CARTESIAN_POINT ( 'NONE',  ( -54.48833221701376317, 1.517896399908648108, -3.311598511235000153 ) ) ;
#29979 = CARTESIAN_POINT ( 'NONE',  ( 48.33000880451179881, -1.140870969100513888, 3.938727831757874664 ) ) ;
#29980 = EDGE_CURVE ( 'NONE', #23272, #29040, #19275, .T. ) ;
#29981 = VERTEX_POINT ( 'NONE', #6598 ) ;
#29982 = FACE_OUTER_BOUND ( 'NONE', #16842, .T. ) ;
#29983 = ORIENTED_EDGE ( 'NONE', *, *, #28388, .T. ) ;
#29984 = ORIENTED_EDGE ( 'NONE', *, *, #6230, .F. ) ;
#29985 = CARTESIAN_POINT ( 'NONE',  ( -59.14374655978132722, 2.337443148762131440, 1.267909066924384875 ) ) ;
#29986 = CIRCLE ( 'NONE', #7744, 2.624999999999998668 ) ;
#29987 = CARTESIAN_POINT ( 'NONE',  ( -59.73542740578360366, 0.7887156198831659637, -3.845940847736173840 ) ) ;
#29989 = CARTESIAN_POINT ( 'NONE',  ( 47.00000000000002132, -3.726179070414207928, -1.710435481158852467 ) ) ;
#29988 = CARTESIAN_POINT ( 'NONE',  ( -55.49999999999997868, -2.944486372867089141, 1.699999999999791678 ) ) ;
#29990 = ORIENTED_EDGE ( 'NONE', *, *, #26761, .F. ) ;
#29991 = VERTEX_POINT ( 'NONE', #23535 ) ;
#29992 = CARTESIAN_POINT ( 'NONE',  ( 61.00000000000001421, 0.8666666666673055186, 1.374595900215364930 ) ) ;
#29993 = ORIENTED_EDGE ( 'NONE', *, *, #12654, .F. ) ;
#29994 = DIRECTION ( 'NONE',  ( -1.000000000000000000, -0.000000000000000000, 3.491481338843133355E-15 ) ) ;
#29995 = ORIENTED_EDGE ( 'NONE', *, *, #10383, .F. ) ;
#29996 = FACE_OUTER_BOUND ( 'NONE', #5815, .T. ) ;
#29997 = CARTESIAN_POINT ( 'NONE',  ( 69.25000000000001421, 5.529431079676072613E-15, -7.253552481446610839E-13 ) ) ;
#29998 = CARTESIAN_POINT ( 'NONE',  ( -61.34999999999997300, -2.565134197206211386, 0.6652717868084008224 ) ) ;
#29999 = CARTESIAN_POINT ( 'NONE',  ( -44.49999999999997868, 1.400000000000009681, -1.540948453285710255E-13 ) ) ;
#30000 = CARTESIAN_POINT ( 'NONE',  ( -58.76905989232410832, 2.023778652682509368E-14, -3.400000000000208189 ) ) ;
#30001 = CARTESIAN_POINT ( 'NONE',  ( 47.86779985288954009, -4.031600731540144977, 1.173113608404348529 ) ) ;
#30002 = LINE ( 'NONE', #13070, #2501 ) ;
#30003 = CARTESIAN_POINT ( 'NONE',  ( 58.66120520918118331, -0.4851952615757724185, 1.811135157337471879 ) ) ;
#30005 = CARTESIAN_POINT ( 'NONE',  ( -59.69999999999997442, 8.366749974758454467E-15, -2.120534355533670266E-13 ) ) ;
#30004 = DIRECTION ( 'NONE',  ( 4.730068669893459805E-15, -0.4531102586349080030, -0.8914544820235112965 ) ) ;
#30006 = AXIS2_PLACEMENT_3D ( 'NONE', #24951, #27016, #10243 ) ;
#30007 = DIRECTION ( 'NONE',  ( 0.000000000000000000, -1.000000000000000000, -3.491481338843134933E-15 ) ) ;
#30008 = EDGE_CURVE ( 'NONE', #11459, #26071, #19099, .T. ) ;
#30009 = CARTESIAN_POINT ( 'NONE',  ( -58.90835481156722864, -3.238593381231842816, -2.874284765127022023 ) ) ;
#30010 = B_SPLINE_CURVE_WITH_KNOTS ( 'NONE', 3,
 ( #25744, #18633, #25894, #13834, #19732, #17490, #26518, #398, #14649, #90, #21950, #17192, #22104 ),
 .UNSPECIFIED., .F., .F.,
 ( 4, 3, 3, 3, 4 ),
 ( 0.000000000000000000, 4.994367907428545029E-05, 9.982969917211881056E-05, 0.0001505119896697729815, 0.0001857353029103987188 ),
 .UNSPECIFIED. ) ;
#30011 = DIRECTION ( 'NONE',  ( 1.282749433769087582E-30, 1.000000000000000000, 1.224646799147353207E-16 ) ) ;
#30012 = ORIENTED_EDGE ( 'NONE', *, *, #817, .F. ) ;
#30013 = CARTESIAN_POINT ( 'NONE',  ( 51.19148447764912646, -0.9872860527319672341, -1.295557643792433433 ) ) ;
#30014 = CARTESIAN_POINT ( 'NONE',  ( 54.39855553801235288, 5.984306564616975521, 1.990863471608376845 ) ) ;
#30015 = ORIENTED_EDGE ( 'NONE', *, *, #6217, .T. ) ;
#30016 = CARTESIAN_POINT ( 'NONE',  ( 50.80000000000002558, -3.908336260473454615, 1.238913909465742424 ) ) ;
#30017 = ORIENTED_EDGE ( 'NONE', *, *, #19680, .F. ) ;
#30018 = CARTESIAN_POINT ( 'NONE',  ( 15.44631504820156209, -0.2166734227622303666, -5.199999998324986272 ) ) ;
#30019 = DIRECTION ( 'NONE',  ( 0.000000000000000000, 0.000000000000000000, 1.000000000000000000 ) ) ;
#30021 = CARTESIAN_POINT ( 'NONE',  ( -44.49999999999996447, -1.399999999999979039, -3.959797974644846619 ) ) ;
#30020 = FACE_OUTER_BOUND ( 'NONE', #72, .T. ) ;
#30022 = ORIENTED_EDGE ( 'NONE', *, *, #21112, .T. ) ;
#30023 = DIRECTION ( 'NONE',  ( 1.000000000000000000, 0.000000000000000000, -0.000000000000000000 ) ) ;
#30024 = EDGE_CURVE ( 'NONE', #19660, #8146, #14513, .T. ) ;
#30025 = CARTESIAN_POINT ( 'NONE',  ( 63.50000000000005684, 1.401298464324817071E-42, 2.624999999999333422 ) ) ;
#30026 = VERTEX_POINT ( 'NONE', #25903 ) ;
#30028 = DIRECTION ( 'NONE',  ( 0.000000000000000000, 1.000000000000000000, 0.000000000000000000 ) ) ;
#30027 = CARTESIAN_POINT ( 'NONE',  ( 59.00000000000002132, 1.401298464324817071E-42, -6.179921969752347932E-13 ) ) ;
#30029 = DIRECTION ( 'NONE',  ( -1.000000000000000000, 1.219044193948984088E-29, -3.491481338843133750E-15 ) ) ;
#30030 = ORIENTED_EDGE ( 'NONE', *, *, #1766, .T. ) ;
#30031 = CIRCLE ( 'NONE', #17906, 0.2500000000000000000 ) ;
#30032 = CARTESIAN_POINT ( 'NONE',  ( -35.85663232820584057, -4.804073783693452171, -2.042134687550364092 ) ) ;
#30033 = DIRECTION ( 'NONE',  ( 1.000000000000000000, -1.219044193948983948E-29, 3.491481338843133355E-15 ) ) ;
#30034 = CARTESIAN_POINT ( 'NONE',  ( 58.75000000000002132, 6.153735859711025284E-13, 3.111507638930570854E-58 ) ) ;
#30035 = CARTESIAN_POINT ( 'NONE',  ( -59.92928932188130631, 0.9743475445367641985, -4.751120590182401848 ) ) ;
#30036 = CARTESIAN_POINT ( 'NONE',  ( -55.50952994616206126, -4.643455692769921685E-15, 3.599999999999801581 ) ) ;
#30038 = VERTEX_POINT ( 'NONE', #11664 ) ;
#30037 = CIRCLE ( 'NONE', #1223, 0.09999999999999867328 ) ;
#30039 =( BOUNDED_CURVE ( )  B_SPLINE_CURVE ( 2, ( #21478, #14174, #28275, #28586, #30633, #18788, #6588, #28753, #2465 ),
 .UNSPECIFIED., .F., .T. ) 
 B_SPLINE_CURVE_WITH_KNOTS ( ( 3, 2, 2, 2, 3 ),
 ( 0.1944444444444444475, 0.2037037037037036924, 0.2222222222222222099, 0.2407407407407407274, 0.2500000000000000000 ),
 .UNSPECIFIED. ) 
 CURVE ( )  GEOMETRIC_REPRESENTATION_ITEM ( )  RATIONAL_B_SPLINE_CURVE ( ( 0.9330127018922192983, 0.9330127018922194093, 1.000000000000000000, 0.8660254037844387076, 1.000000000000000000, 0.8660254037844387076, 1.000000000000000000, 0.9330127018922191873, 0.9330127018922192983 ) ) 
 REPRESENTATION_ITEM ( '' )  );
#30040 = CARTESIAN_POINT ( 'NONE',  ( 15.03925126672132961, -2.199885893005964377, 4.939696249117675464 ) ) ;
#30041 = CARTESIAN_POINT ( 'NONE',  ( -54.61042740578361077, -2.936324665650201116, -2.606018187048499080 ) ) ;
#30042 = EDGE_CURVE ( 'NONE', #25236, #7825, #856, .T. ) ;
#30043 = CARTESIAN_POINT ( 'NONE',  ( 53.54945414537598936, 7.685533664402775855, -1.865296808329178102 ) ) ;
#30044 = CIRCLE ( 'NONE', #6803, 0.2500000000000000000 ) ;
#30045 = CYLINDRICAL_SURFACE ( 'NONE', #17386, 1.000000000000000000 ) ;
#30046 = EDGE_CURVE ( 'NONE', #19199, #27197, #30686, .T. ) ;
#30047 = CARTESIAN_POINT ( 'NONE',  ( -56.50952994616203995, 3.117691453623998132, -1.800000000000180123 ) ) ;
#30048 = FACE_OUTER_BOUND ( 'NONE', #6401, .T. ) ;
#30049 = CARTESIAN_POINT ( 'NONE',  ( 31.44395763972472579, 7.534587386684770571, 2.049999999999888800 ) ) ;
#30050 = ORIENTED_EDGE ( 'NONE', *, *, #8366, .T. ) ;
#30051 = CARTESIAN_POINT ( 'NONE',  ( 69.20000000000000284, 0.8558823529411767606, -2.268940368966791077 ) ) ;
#30052 = ORIENTED_EDGE ( 'NONE', *, *, #14039, .T. ) ;
#30053 = UNCERTAINTY_MEASURE_WITH_UNIT (LENGTH_MEASURE( 1.000000000000000082E-05 ), #16501, 'distance_accuracy_value', 'NONE');
#30054 = DIRECTION ( 'NONE',  ( 1.000000000000000000, 1.047444401652940007E-14, 0.000000000000000000 ) ) ;
#30056 = CARTESIAN_POINT ( 'NONE',  ( -59.29999999999997584, 2.330309927981285032E-15, 4.253626757584724400E-16 ) ) ;
#30055 = CARTESIAN_POINT ( 'NONE',  ( 48.37884656342667711, 0.9200365198983960768, 3.998286360709680576 ) ) ;
#30057 = ORIENTED_EDGE ( 'NONE', *, *, #15952, .T. ) ;
#30058 = VERTEX_POINT ( 'NONE', #9617 ) ;
#30059 = DIRECTION ( 'NONE',  ( 0.000000000000000000, -0.2008964009354162750, 0.9796124928211136229 ) ) ;
#30060 = ADVANCED_FACE ( 'NONE', ( #11973 ), #6745, .T. ) ;
#30061 = FACE_OUTER_BOUND ( 'NONE', #18767, .T. ) ;
#30062 = ORIENTED_EDGE ( 'NONE', *, *, #16853, .T. ) ;
#30064 = DIRECTION ( 'NONE',  ( -1.000000000000000000, -0.000000000000000000, -0.000000000000000000 ) ) ;
#30063 = CARTESIAN_POINT ( 'NONE',  ( -58.07202994616203995, 2.078460969082674747, -3.600000000000197709 ) ) ;
#30065 = CARTESIAN_POINT ( 'NONE',  ( -55.86042740578360366, 3.725040285533370632, -1.239922660687676315 ) ) ;
#30066 = AXIS2_PLACEMENT_3D ( 'NONE', #19117, #13051, #26983 ) ;
#30067 = AXIS2_PLACEMENT_3D ( 'NONE', #26212, #9436, #18630 ) ;
#30068 = CARTESIAN_POINT ( 'NONE',  ( -36.11187263677958015, -4.822464347459074929, -1.985534350301396911 ) ) ;
#30069 = CARTESIAN_POINT ( 'NONE',  ( 46.90000000000001279, 2.258259982612300799E-15, -4.275000000000000355 ) ) ;
#30070 = VECTOR ( 'NONE', #27786, 1000.000000000000000 ) ;
#30071 = ORIENTED_EDGE ( 'NONE', *, *, #7831, .F. ) ;
#30072 = CARTESIAN_POINT ( 'NONE',  ( 47.02303712724481244, -4.162962223351915902, -1.036150832289954193 ) ) ;
#30073 = AXIS2_PLACEMENT_3D ( 'NONE', #19353, #4757, #30901 ) ;
#30074 = CARTESIAN_POINT ( 'NONE',  ( 52.38400031671216794, 8.538946093000149062, -2.050000000000181899 ) ) ;
#30075 = CARTESIAN_POINT ( 'NONE',  ( 51.23644008536121675, 1.080112125196981410, -1.214076932077873039 ) ) ;
#30076 = CARTESIAN_POINT ( 'NONE',  ( -74.39999999999997726, -2.588216748940040213E-15, 4.710014593512140639E-15 ) ) ;
#30077 = CYLINDRICAL_SURFACE ( 'NONE', #4392, 3.750000000000000444 ) ;
#30078 = EDGE_CURVE ( 'NONE', #22071, #26766, #7401, .T. ) ;
#30079 = CARTESIAN_POINT ( 'NONE',  ( 58.75000018595672913, -1.883137918659851806, -0.4528999722754138424 ) ) ;
#30080 = B_SPLINE_CURVE_WITH_KNOTS ( 'NONE', 3,
 ( #2277, #28888, #11941, #2450 ),
 .UNSPECIFIED., .F., .F.,
 ( 4, 4 ),
 ( 0.000000000000000000, 0.0003845111068534253374 ),
 .UNSPECIFIED. ) ;
#30081 = ADVANCED_FACE ( 'NONE', ( #21660 ), #7441, .T. ) ;
#30082 = AXIS2_PLACEMENT_3D ( 'NONE', #5879, #10929, #8556 ) ;
#30083 = CARTESIAN_POINT ( 'NONE',  ( 58.75000000000003553, -1.470078920827193825, -1.320078920827526758 ) ) ;
#30084 = CARTESIAN_POINT ( 'NONE',  ( -61.09509470490394278, -2.484918463451591730, -0.8819564647444799732 ) ) ;
#30086 = CARTESIAN_POINT ( 'NONE',  ( -59.65431995858129710, 2.042084323596708995, 1.713960027490288862 ) ) ;
#30085 = DIRECTION ( 'NONE',  ( -1.047444401652940007E-14, 0.000000000000000000, -1.000000000000000000 ) ) ;
#30087 = VECTOR ( 'NONE', #6510, 1000.000000000000114 ) ;
#30088 = ORIENTED_EDGE ( 'NONE', *, *, #6824, .F. ) ;
#30089 = DIRECTION ( 'NONE',  ( 0.000000000000000000, 0.000000000000000000, -1.000000000000000000 ) ) ;
#30091 = DIRECTION ( 'NONE',  ( 0.000000000000000000, 0.000000000000000000, 1.000000000000000000 ) ) ;
#30090 = PLANE ( 'NONE',  #31193 ) ;
#30092 = VERTEX_POINT ( 'NONE', #23708 ) ;
#30093 = CARTESIAN_POINT ( 'NONE',  ( 52.48717296556563383, 8.620750214766543351, 2.049999999999817302 ) ) ;
#30094 = CARTESIAN_POINT ( 'NONE',  ( -60.64959257988790853, -2.458630613964993383, -1.115856434191108359 ) ) ;
#30095 = AXIS2_PLACEMENT_3D ( 'NONE', #13993, #8935, #1644 ) ;
#30096 = ADVANCED_FACE ( 'NONE', ( #18952 ), #21342, .F. ) ;
#30097 = ORIENTED_EDGE ( 'NONE', *, *, #12096, .F. ) ;
#30098 = AXIS2_PLACEMENT_3D ( 'NONE', #9374, #6832, #16499 ) ;
#30099 = DIRECTION ( 'NONE',  ( 0.000000000000000000, 0.000000000000000000, -1.000000000000000000 ) ) ;
#30100 = ORIENTED_EDGE ( 'NONE', *, *, #25537, .T. ) ;
#30101 = DIRECTION ( 'NONE',  ( 0.7071067811865549002, -0.7071067811865402453, 8.659560562354930393E-17 ) ) ;
#30102 = CARTESIAN_POINT ( 'NONE',  ( 51.59739104186227365, 1.010292945603182169, -1.272765950230260401 ) ) ;
#30103 = EDGE_LOOP ( 'NONE', ( #16458, #10867, #21745, #26404, #16889 ) ) ;
#30104 = CARTESIAN_POINT ( 'NONE',  ( 52.08333333333334991, 4.368973594129894167, -1.439468559502902645 ) ) ;
#30105 = CARTESIAN_POINT ( 'NONE',  ( -58.58155989232412253, 3.925981830489463142, -1.937197393286790192E-13 ) ) ;
#30106 = ORIENTED_EDGE ( 'NONE', *, *, #11955, .T. ) ;
#30107 = DIRECTION ( 'NONE',  ( -1.047444401652940007E-14, 0.000000000000000000, -1.000000000000000000 ) ) ;
#30108 = EDGE_CURVE ( 'NONE', #15114, #4338, #15529, .T. ) ;
#30109 = AXIS2_PLACEMENT_3D ( 'NONE', #20114, #29748, #5680 ) ;
#30110 = ORIENTED_EDGE ( 'NONE', *, *, #5952, .F. ) ;
#30111 = CIRCLE ( 'NONE', #24554, 160.6997717543497686 ) ;
#30112 = CARTESIAN_POINT ( 'NONE',  ( -56.18749999999997158, -3.925981830489445379, -2.137374967025826226E-13 ) ) ;
#30113 = CARTESIAN_POINT ( 'NONE',  ( 61.16289782575175593, 0.6851579758935786302, 1.477831714898440341 ) ) ;
#30114 = CARTESIAN_POINT ( 'NONE',  ( -61.34999999999997300, -2.528827883897363904, -0.7921676171260561006 ) ) ;
#30115 = CARTESIAN_POINT ( 'NONE',  ( 56.95000000000001705, -0.6917305289283675052, -1.769637370168020141 ) ) ;
#30116 = AXIS2_PLACEMENT_3D ( 'NONE', #941, #3619, #5837 ) ;
#30117 = CARTESIAN_POINT ( 'NONE',  ( -54.49999999999997158, -1.370882916971243537, -3.219442999905937075 ) ) ;
#30118 = AXIS2_PLACEMENT_3D ( 'NONE', #25995, #28228, #9068 ) ;
#30119 = EDGE_CURVE ( 'NONE', #618, #1564, #12036, .T. ) ;
#30120 = AXIS2_PLACEMENT_3D ( 'NONE', #21773, #4490, #31252 ) ;
#30122 = CARTESIAN_POINT ( 'NONE',  ( -35.85663232820584057, 4.817150320979497913, 2.203324261490556157 ) ) ;
#30121 = FACE_OUTER_BOUND ( 'NONE', #24483, .T. ) ;
#30123 = ADVANCED_FACE ( 'NONE', ( #26379 ), #7222, .F. ) ;
#30124 = EDGE_CURVE ( 'NONE', #3567, #30652, #18391, .T. ) ;
#30125 = DIRECTION ( 'NONE',  ( 0.000000000000000000, -1.000000000000000000, -3.491481338843136116E-15 ) ) ;
#30126 = CARTESIAN_POINT ( 'NONE',  ( -59.68054851456403753, 2.392282282077082378, -1.229557205448917445 ) ) ;
#30127 = DIRECTION ( 'NONE',  ( -2.117927888850090838E-16, 0.02490330187381123786, -0.9996898646859343485 ) ) ;
#30128 = CARTESIAN_POINT ( 'NONE',  ( 58.75000000694006275, 1.381609951798780767, -1.346330794793079155 ) ) ;
#30129 = CIRCLE ( 'NONE', #15474, 4.100000000000022737 ) ;
#30130 = CARTESIAN_POINT ( 'NONE',  ( 50.59602332238209499, -0.1408342061598474304, 1.125000000000000888 ) ) ;
#30131 = EDGE_LOOP ( 'NONE', ( #16057, #27613, #2700, #23782, #761 ) ) ;
#30132 = CARTESIAN_POINT ( 'NONE',  ( -54.49999999999997158, -3.476573872757579231, -0.4722677507125554452 ) ) ;
#30133 = AXIS2_PLACEMENT_3D ( 'NONE', #19528, #29174, #506 ) ;
#30134 = CARTESIAN_POINT ( 'NONE',  ( 58.65000000000003411, -0.9947034709615889536, 1.589751505945788956 ) ) ;
#30135 = ORIENTED_EDGE ( 'NONE', *, *, #11641, .F. ) ;
#30136 = CIRCLE ( 'NONE', #15990, 4.384222560975607585 ) ;
#30137 = EDGE_LOOP ( 'NONE', ( #19875, #16495, #1932, #7956 ) ) ;
#30138 = PRESENTATION_STYLE_ASSIGNMENT (( #20815 ) ) ;
#30139 = FACE_OUTER_BOUND ( 'NONE', #30223, .T. ) ;
#30141 = CARTESIAN_POINT ( 'NONE',  ( -61.35193852616566090, -2.578113109134980707, 0.6701466704936713814 ) ) ;
#30140 = CARTESIAN_POINT ( 'NONE',  ( -57.18749999999998579, 1.962990915244722689, 3.399999999999804956 ) ) ;
#30142 = ORIENTED_EDGE ( 'NONE', *, *, #29734, .F. ) ;
#30143 = TOROIDAL_SURFACE ( 'NONE', #28652, 1.975000000000001865, 0.1000000000000000056 ) ;
#30144 = ORIENTED_EDGE ( 'NONE', *, *, #13783, .T. ) ;
#30145 = CARTESIAN_POINT ( 'NONE',  ( -44.59999999999998721, 1.514093959731539263, 3.183260039818184062 ) ) ;
#30146 = EDGE_LOOP ( 'NONE', ( #25869, #22639, #17060, #12331 ) ) ;
#30147 = VECTOR ( 'NONE', #27477, 1000.000000000000000 ) ;
#30149 = CARTESIAN_POINT ( 'NONE',  ( 51.50435016707358926, 0.9265794315412880788, -1.339215852266871565 ) ) ;
#30148 = AXIS2_PLACEMENT_3D ( 'NONE', #17916, #20772, #13150 ) ;
#30150 = VERTEX_POINT ( 'NONE', #14799 ) ;
#30151 = CARTESIAN_POINT ( 'NONE',  ( 23.07431837327370161, 6.199584068344814902, -2.050000000000079758 ) ) ;
#30152 = AXIS2_PLACEMENT_3D ( 'NONE', #14614, #2107, #24280 ) ;
#30153 = ORIENTED_EDGE ( 'NONE', *, *, #19523, .F. ) ;
#30154 = DIRECTION ( 'NONE',  ( 0.000000000000000000, 1.000000000000000000, 0.000000000000000000 ) ) ;
#30155 = EDGE_CURVE ( 'NONE', #21818, #29917, #23655, .T. ) ;
#30156 = FACE_OUTER_BOUND ( 'NONE', #1039, .T. ) ;
#30157 = B_SPLINE_CURVE_WITH_KNOTS ( 'NONE', 3,
 ( #26077, #21205, #11528, #9475, #25921, #21032, #4226, #11348, #23556, #1856, #4391, #30837, #18816, #21360, #14038, #3400 ),
 .UNSPECIFIED., .F., .F.,
 ( 4, 2, 2, 2, 2, 2, 2, 4 ),
 ( 2.168404344971008868E-19, 0.0007944403960943761467, 0.001191660594141564274, 0.001390270693165157959, 0.001489575742676953717, 0.001539228267432849644, 0.001564054529810800318, 0.001588880792188750992 ),
 .UNSPECIFIED. ) ;
#30158 = FACE_OUTER_BOUND ( 'NONE', #6775, .T. ) ;
#30159 = EDGE_CURVE ( 'NONE', #363, #18295, #20111, .T. ) ;
#30160 = AXIS2_PLACEMENT_3D ( 'NONE', #10804, #13485, #15576 ) ;
#30161 = CARTESIAN_POINT ( 'NONE',  ( -59.01905989232412253, -2.944486372867088697, 1.699999999999779243 ) ) ;
#30162 = CARTESIAN_POINT ( 'NONE',  ( 47.20240392245177219, -3.813771782910507557, 1.508835477669279168 ) ) ;
#30163 = CIRCLE ( 'NONE', #336, 4.299999999999954525 ) ;
#30164 = CARTESIAN_POINT ( 'NONE',  ( 58.65838214097819048, 1.349359547238225376, 1.301971553120433001 ) ) ;
#30165 = VECTOR ( 'NONE', #9860, 1000.000000000000000 ) ;
#30166 = CARTESIAN_POINT ( 'NONE',  ( 58.65000000000001279, 0.5811678240991626776, -1.782657835994492457 ) ) ;
#30167 = AXIS2_PLACEMENT_3D ( 'NONE', #4270, #30730, #18862 ) ;
#30168 = DIRECTION ( 'NONE',  ( -0.9993908270190957621, 0.03489949670250106634, 3.490838185622846777E-15 ) ) ;
#30170 = CARTESIAN_POINT ( 'NONE',  ( 50.80000000000002558, -4.319730106884872356, 1.256953381662059055 ) ) ;
#30169 = CARTESIAN_POINT ( 'NONE',  ( 51.14630318392396902, -0.9364487020628400327, 1.503522130792752209 ) ) ;
#30171 = AXIS2_PLACEMENT_3D ( 'NONE', #25345, #3651, #13724 ) ;
#30172 = AXIS2_PLACEMENT_3D ( 'NONE', #15062, #5098, #22209 ) ;
#30173 = DIRECTION ( 'NONE',  ( 1.000000000000000000, -1.219044193948983948E-29, 3.491481338843133355E-15 ) ) ;
#30174 = CARTESIAN_POINT ( 'NONE',  ( -58.84585481156723574, -1.184343223768586473, -3.558065644182725418 ) ) ;
#30175 = AXIS2_PLACEMENT_3D ( 'NONE', #23014, #17951, #27293 ) ;
#30176 = CARTESIAN_POINT ( 'NONE',  ( 51.38214458811558671, -1.084857585945107505, 1.209959298770751923 ) ) ;
#30177 = CIRCLE ( 'NONE', #15012, 2.600000000000000089 ) ;
#30178 = ORIENTED_EDGE ( 'NONE', *, *, #10400, .F. ) ;
#30179 = CARTESIAN_POINT ( 'NONE',  ( 54.40301487434273753, 5.980869423001016649, -0.9750000000001823874 ) ) ;
#30180 = EDGE_LOOP ( 'NONE', ( #11420, #20595, #15632, #1790 ) ) ;
#30181 = FACE_OUTER_BOUND ( 'NONE', #24174, .T. ) ;
#30182 = ORIENTED_EDGE ( 'NONE', *, *, #27509, .T. ) ;
#30183 = CARTESIAN_POINT ( 'NONE',  ( 52.05393800078983446, 4.345106731198570493, 1.549654688285104331 ) ) ;
#30184 = CARTESIAN_POINT ( 'NONE',  ( -57.22085481156723574, 2.489203624310592389, -2.804704140674919355 ) ) ;
#30186 = FACE_OUTER_BOUND ( 'NONE', #18922, .T. ) ;
#30185 = CARTESIAN_POINT ( 'NONE',  ( 60.88854248453768747, -0.6773709096934548146, 1.477839832418263333 ) ) ;
#30187 = AXIS2_PLACEMENT_3D ( 'NONE', #21737, #9691, #7298 ) ;
#30188 = VERTEX_POINT ( 'NONE', #27311 ) ;
#30189 = CARTESIAN_POINT ( 'NONE',  ( 47.05963571244990362, 8.266527678078146479, -2.050000000000163691 ) ) ;
#30190 = AXIS2_PLACEMENT_3D ( 'NONE', #24810, #10247, #7864 ) ;
#30191 = CARTESIAN_POINT ( 'NONE',  ( 57.03513260258041839, -0.7477432062408043700, -1.780365573899210574 ) ) ;
#30192 = AXIS2_PLACEMENT_3D ( 'NONE', #17083, #7707, #14361 ) ;
#30193 = ORIENTED_EDGE ( 'NONE', *, *, #24967, .F. ) ;
#30194 = DIRECTION ( 'NONE',  ( 1.000000000000000000, 0.000000000000000000, -1.047444401652940007E-14 ) ) ;
#30195 = DIRECTION ( 'NONE',  ( 1.000000000000000000, -0.000000000000000000, -0.000000000000000000 ) ) ;
#30196 = ORIENTED_EDGE ( 'NONE', *, *, #8696, .T. ) ;
#30197 = CARTESIAN_POINT ( 'NONE',  ( -36.58413561666694847, 5.174628573245025898, -1.572974725650795991 ) ) ;
#30198 = ADVANCED_FACE ( 'NONE', ( #29064 ), #12418, .T. ) ;
#30199 = CARTESIAN_POINT ( 'NONE',  ( 58.65838214097848180, 1.606847897768966860, -0.9664062014978758164 ) ) ;
#30200 = EDGE_CURVE ( 'NONE', #21439, #10001, #24154, .T. ) ;
#30201 = AXIS2_PLACEMENT_3D ( 'NONE', #140, #17547, #746 ) ;
#30202 = DIRECTION ( 'NONE',  ( 1.000000000000000000, 3.053848253006669023E-16, -2.042510438544995415E-16 ) ) ;
#30203 = DIRECTION ( 'NONE',  ( 0.000000000000000000, 0.000000000000000000, -1.000000000000000000 ) ) ;
#30204 = VECTOR ( 'NONE', #28020, 999.9999999999998863 ) ;
#30205 = EDGE_CURVE ( 'NONE', #15656, #25275, #3425, .T. ) ;
#30206 = VECTOR ( 'NONE', #18271, 1000.000000000000000 ) ;
#30207 = CARTESIAN_POINT ( 'NONE',  ( 51.69060524974067050, -0.7995873297236903987, 1.427997211815761780 ) ) ;
#30208 = ORIENTED_EDGE ( 'NONE', *, *, #8941, .T. ) ;
#30209 = CARTESIAN_POINT ( 'NONE',  ( 15.49702763512084402, 3.100731772197714342, 4.174739983989972814 ) ) ;
#30210 = AXIS2_PLACEMENT_3D ( 'NONE', #22783, #30494, #15646 ) ;
#30211 = AXIS2_PLACEMENT_3D ( 'NONE', #21993, #31007, #9328 ) ;
#30212 = SPHERICAL_SURFACE ( 'NONE', #30116, 0.05000000000000000278 ) ;
#30213 = ADVANCED_FACE ( 'NONE', ( #15274, #7823 ), #7539, .T. ) ;
#30214 = CIRCLE ( 'NONE', #11011, 1.000000000000000000 ) ;
#30215 = APPLICATION_CONTEXT ( 'automotive_design' ) ;
#30216 = LINE ( 'NONE', #8360, #26078 ) ;
#30217 = CARTESIAN_POINT ( 'NONE',  ( -58.25952994616203284, -3.117691453623959497, -1.800000000000225198 ) ) ;
#30218 = CARTESIAN_POINT ( 'NONE',  ( 58.65000045311414567, -1.873226731663665712, -0.08323357347563117847 ) ) ;
#30219 = CARTESIAN_POINT ( 'NONE',  ( 48.46694841591348535, 1.365427245289844826, -3.854926352964885172 ) ) ;
#30220 = EDGE_LOOP ( 'NONE', ( #28756, #30309, #24667, #27581 ) ) ;
#30221 = AXIS2_PLACEMENT_3D ( 'NONE', #4843, #15124, #25250 ) ;
#30222 = CARTESIAN_POINT ( 'NONE',  ( 58.75000000000000711, 1.652350234724653477, 1.065927491745260358 ) ) ;
#30223 = EDGE_LOOP ( 'NONE', ( #20974, #366, #12802, #17585 ) ) ;
#30224 = CARTESIAN_POINT ( 'NONE',  ( -59.16814806244811109, 2.503608436921294533, -0.9454277352718696292 ) ) ;
#30226 = DIRECTION ( 'NONE',  ( 1.000000000000000000, 3.054025858079668409E-16, -2.042474015755241579E-16 ) ) ;
#30225 = CARTESIAN_POINT ( 'NONE',  ( 58.75000000000000711, 0.8948927608039201065, -1.760622601996761682 ) ) ;
#30227 = ORIENTED_EDGE ( 'NONE', *, *, #20143, .T. ) ;
#30228 = ORIENTED_EDGE ( 'NONE', *, *, #6537, .F. ) ;
#30229 = FACE_BOUND ( 'NONE', #7449, .T. ) ;
#30230 = CARTESIAN_POINT ( 'NONE',  ( 31.20024169076946308, 7.859880411735725048, 1.424999999999890798 ) ) ;
#30232 = LINE ( 'NONE', #11073, #26149 ) ;
#30231 = CARTESIAN_POINT ( 'NONE',  ( 56.95000000000001705, 0.6820512820512819596, -1.773360101234998210 ) ) ;
#30233 = CARTESIAN_POINT ( 'NONE',  ( -56.61042740578360366, 3.725040285533371076, -1.239922660687675871 ) ) ;
#30234 = DIRECTION ( 'NONE',  ( 1.000000000000000000, 1.047444401652940007E-14, 0.000000000000000000 ) ) ;
#30235 = AXIS2_PLACEMENT_3D ( 'NONE', #925, #445, #10577 ) ;
#30236 = ADVANCED_FACE ( 'NONE', ( #2936 ), #24776, .T. ) ;
#30237 = B_SPLINE_CURVE_WITH_KNOTS ( 'NONE', 3,
 ( #29360, #10200, #17330, #232, #12409, #22400 ),
 .UNSPECIFIED., .F., .F.,
 ( 4, 2, 4 ),
 ( 0.000000000000000000, 0.0001000270069609034211, 0.0002000540139218068422 ),
 .UNSPECIFIED. ) ;
#30238 = CARTESIAN_POINT ( 'NONE',  ( 53.19737178513464215, 4.872051914464355704, -1.602904050740938890 ) ) ;
#30239 =( BOUNDED_SURFACE ( )  B_SPLINE_SURFACE ( 3, 2, ( 
 ( #24733, #7498, #10169 ),
 ( #26946, #19838, #12689 ),
 ( #8257, #29794, #6056 ),
 ( #3358, #8566, #22844 ) ),
 .UNSPECIFIED., .F., .F., .F. ) 
 B_SPLINE_SURFACE_WITH_KNOTS ( ( 4, 4 ),
 ( 3, 3 ),
 ( 7.146054570217184225E-05, 0.0002313930902385299038 ),
 ( 0.000000000000000000, 1.000000000000000000 ),
 .UNSPECIFIED. ) 
 GEOMETRIC_REPRESENTATION_ITEM ( )  RATIONAL_B_SPLINE_SURFACE ( (
 ( 1.000000000000000000, 0.7071067811864972796, 1.000000000000000000),
 ( 1.000000000000000000, 0.6583912147046423469, 1.000000000000000000),
 ( 1.000000000000000000, 0.5850387677749523396, 1.000000000000000000),
 ( 1.000000000000000000, 0.5857791861290068125, 1.000000000000000000) ) ) 
 REPRESENTATION_ITEM ( '' )  SURFACE ( )  );
#30240 =( NAMED_UNIT ( * ) PLANE_ANGLE_UNIT ( ) SI_UNIT ( $, .RADIAN. ) );
#30241 = ORIENTED_EDGE ( 'NONE', *, *, #864, .T. ) ;
#30242 = DIRECTION ( 'NONE',  ( -0.9993908270190952070, 0.03489949670251432656, 3.492791461889839594E-15 ) ) ;
#30243 = FACE_OUTER_BOUND ( 'NONE', #30413, .T. ) ;
#30244 = DIRECTION ( 'NONE',  ( 0.000000000000000000, 0.000000000000000000, 1.000000000000000000 ) ) ;
#30245 = CARTESIAN_POINT ( 'NONE',  ( 15.41586008885035142, 0.2667568399900541176, 5.200000000294856761 ) ) ;
#30246 = DIRECTION ( 'NONE',  ( -1.000000000000000000, -0.000000000000000000, 3.491481338843133355E-15 ) ) ;
#30247 = ADVANCED_FACE ( 'NONE', ( #12580 ), #3239, .F. ) ;
#30249 = CARTESIAN_POINT ( 'NONE',  ( 50.25000000000003553, -1.470078920828004732, 1.470078920827824209 ) ) ;
#30248 = CARTESIAN_POINT ( 'NONE',  ( 50.87826055314399554, 8.733544086820096197, 1.949999999999822320 ) ) ;
#30250 = TOROIDAL_SURFACE ( 'NONE', #17639, 1.949999999999999956, 0.05000000000000000278 ) ;
#30251 = AXIS2_PLACEMENT_3D ( 'NONE', #26959, #4973, #12552 ) ;
#30252 = CARTESIAN_POINT ( 'NONE',  ( -44.59999999999998721, 1.399999999999996136, 3.959797974644455376 ) ) ;
#30254 = CARTESIAN_POINT ( 'NONE',  ( 51.25000000000001421, 5.368152558471320595E-13, 3.111507638930570854E-58 ) ) ;
#30253 = CYLINDRICAL_SURFACE ( 'NONE', #6424, 0.1000000000000000472 ) ;
#30255 = ORIENTED_EDGE ( 'NONE', *, *, #11598, .T. ) ;
#30256 = CARTESIAN_POINT ( 'NONE',  ( 58.65000000000001990, 6.143261415694495821E-13, 3.111507638930570854E-58 ) ) ;
#30257 = FACE_OUTER_BOUND ( 'NONE', #16814, .T. ) ;
#30259 = CARTESIAN_POINT ( 'NONE',  ( 58.65000000000004121, -0.9941784314380475163, -1.590093208332685082 ) ) ;
#30258 = CARTESIAN_POINT ( 'NONE',  ( 15.03925126672132961, -1.793057972834775970, -4.026191436120402756 ) ) ;
#30260 = CARTESIAN_POINT ( 'NONE',  ( 47.10000000000002274, -4.179189514726508570, 0.8999999999999996891 ) ) ;
#30261 = EDGE_LOOP ( 'NONE', ( #18399, #24856 ) ) ;
#30262 = ADVANCED_FACE ( 'NONE', ( #17053 ), #24459, .T. ) ;
#30263 = FACE_OUTER_BOUND ( 'NONE', #27674, .T. ) ;
#30264 = CARTESIAN_POINT ( 'NONE',  ( -60.62155403265821718, -2.458719867916568269, -1.094860189600118439 ) ) ;
#30265 = ORIENTED_EDGE ( 'NONE', *, *, #22364, .F. ) ;
#30266 = CARTESIAN_POINT ( 'NONE',  ( 58.75000000000003553, -1.470078920827206925, -1.470078920827526892 ) ) ;
#30267 = EDGE_LOOP ( 'NONE', ( #4992, #4754, #24745, #14014, #11033, #21813, #23743, #1927 ) ) ;
#30268 = CYLINDRICAL_SURFACE ( 'NONE', #18917, 4.849999999999999645 ) ;
#30269 = CARTESIAN_POINT ( 'NONE',  ( 51.24551381660813831, -1.093420264358021532, -1.202138525661323731 ) ) ;
#30270 = ORIENTED_EDGE ( 'NONE', *, *, #3503, .T. ) ;
#30271 = CARTESIAN_POINT ( 'NONE',  ( -35.85663232820584767, 3.817150320980632561, 2.203324261490556157 ) ) ;
#30272 = ADVANCED_FACE ( 'NONE', ( #553 ), #18322, .T. ) ;
#30273 = CARTESIAN_POINT ( 'NONE',  ( -58.39405989232412963, -3.920666489018312013E-15, 3.399999999999791633 ) ) ;
#30274 = VERTEX_POINT ( 'NONE', #30231 ) ;
#30275 = VERTEX_POINT ( 'NONE', #27861 ) ;
#30276 = ORIENTED_EDGE ( 'NONE', *, *, #9715, .T. ) ;
#30277 = AXIS2_PLACEMENT_3D ( 'NONE', #25068, #26408, #3403 ) ;
#30278 = CARTESIAN_POINT ( 'NONE',  ( -56.12499999999996447, -2.944486372867076707, -1.700000000000210010 ) ) ;
#30279 = CARTESIAN_POINT ( 'NONE',  ( 60.75000000000001421, 0.5000000000006363798, 1.718465885608440047 ) ) ;
#30280 = CARTESIAN_POINT ( 'NONE',  ( -59.29999999999997584, 0.7533615035078071731, -3.673546848079177085 ) ) ;
#30281 = CARTESIAN_POINT ( 'NONE',  ( 50.50000000000002132, 5.291762632692320630E-13, -1.996089927833914146 ) ) ;
#30282 = CARTESIAN_POINT ( 'NONE',  ( -59.09999999999998010, -2.331118226142294247, 1.260312586522342349 ) ) ;
#30283 = ADVANCED_FACE ( 'NONE', ( #8831 ), #15968, .T. ) ;
#30285 = SPHERICAL_SURFACE ( 'NONE', #11352, 0.1000000000000000056 ) ;
#30284 = DIRECTION ( 'NONE',  ( 0.000000000000000000, -1.000000000000000000, 0.000000000000000000 ) ) ;
#30286 = AXIS2_PLACEMENT_3D ( 'NONE', #17839, #6116, #5793 ) ;
#30287 = SURFACE_SIDE_STYLE ('',( #20661 ) ) ;
#30288 = CARTESIAN_POINT ( 'NONE',  ( -54.49999999999997868, 4.751120590182407177, 0.9743475445367620891 ) ) ;
#30289 = CARTESIAN_POINT ( 'NONE',  ( 61.25000000000000000, 1.800471618824969422, -1.039502773795712987 ) ) ;
#30290 = CARTESIAN_POINT ( 'NONE',  ( 54.04962709127944720, 6.684747557764787906, 2.023090456646976509 ) ) ;
#30291 = LINE ( 'NONE', #12725, #11988 ) ;
#30292 = DIRECTION ( 'NONE',  ( -3.002035892788117952E-16, 0.9996898646859344595, 0.02490330187381124133 ) ) ;
#30293 = ORIENTED_EDGE ( 'NONE', *, *, #14437, .F. ) ;
#30294 = CARTESIAN_POINT ( 'NONE',  ( 15.03925126672133139, -4.804073783693452171, 2.042134687550334338 ) ) ;
#30295 = EDGE_CURVE ( 'NONE', #1451, #30275, #4929, .T. ) ;
#30296 = DIRECTION ( 'NONE',  ( -1.344447539785323523E-44, 1.000000000000000000, 3.491481338843137300E-15 ) ) ;
#30297 = AXIS2_PLACEMENT_3D ( 'NONE', #7758, #12980, #27240 ) ;
#30298 = AXIS2_PLACEMENT_3D ( 'NONE', #2070, #4747, #31209 ) ;
#30299 = ORIENTED_EDGE ( 'NONE', *, *, #18744, .F. ) ;
#30300 = DIRECTION ( 'NONE',  ( -1.000000000000000000, -3.053848253006669023E-16, 2.042510438544995415E-16 ) ) ;
#30302 = CARTESIAN_POINT ( 'NONE',  ( 47.02574391948114396, -4.052343190076495461, 1.949685991417499764 ) ) ;
#30301 = CARTESIAN_POINT ( 'NONE',  ( -56.62499999999996447, 2.944486372867106905, -1.700000000000188471 ) ) ;
#30303 = ORIENTED_EDGE ( 'NONE', *, *, #2930, .T. ) ;
#30304 = ORIENTED_EDGE ( 'NONE', *, *, #20530, .T. ) ;
#30305 = CARTESIAN_POINT ( 'NONE',  ( 51.60192307426172675, -4.191416138886287612, -1.624134901684648913 ) ) ;
#30306 = EDGE_LOOP ( 'NONE', ( #7741, #29429, #23599, #24027 ) ) ;
#30307 = CARTESIAN_POINT ( 'NONE',  ( 58.73379417893125520, -1.582215608938960072, 1.006340787080793220 ) ) ;
#30308 = EDGE_CURVE ( 'NONE', #23733, #22781, #2920, .T. ) ;
#30309 = ORIENTED_EDGE ( 'NONE', *, *, #20722, .T. ) ;
#30310 = CARTESIAN_POINT ( 'NONE',  ( 22.18976255005414444, 7.481058471420858780, -2.050000000000077094 ) ) ;
#30311 = ADVANCED_FACE ( 'NONE', ( #28332 ), #15050, .T. ) ;
#30312 = DIRECTION ( 'NONE',  ( 1.000000000000000000, 0.000000000000000000, 0.000000000000000000 ) ) ;
#30313 = ADVANCED_FACE ( 'NONE', ( #23425 ), #19615, .T. ) ;
#30314 = DIRECTION ( 'NONE',  ( 1.000000000000000000, 3.054025858079668409E-16, -2.042474015755241579E-16 ) ) ;
#30315 = VERTEX_POINT ( 'NONE', #6483 ) ;
#30316 = CARTESIAN_POINT ( 'NONE',  ( 47.10000000000002274, -4.259946800035237402, -1.000000000000000222 ) ) ;
#30317 = CARTESIAN_POINT ( 'NONE',  ( -62.09999999999997300, -2.737615117699082834, 0.2585595776647297561 ) ) ;
#30318 = CARTESIAN_POINT ( 'NONE',  ( 51.23018762252620917, -0.9889900474263613184, 1.419502710324607841 ) ) ;
#30319 = CARTESIAN_POINT ( 'NONE',  ( 48.00000000000002132, -4.031600731908414836, 1.173113608511506367 ) ) ;
#30320 = CARTESIAN_POINT ( 'NONE',  ( 58.66122797211841799, 1.314214529126963793, 1.337438849765042681 ) ) ;
#30321 = TOROIDAL_SURFACE ( 'NONE', #4546, 1.975000000000001865, 0.1000000000000000056 ) ;
#30322 = CARTESIAN_POINT ( 'NONE',  ( 51.49472959044965137, 1.070956530528825557, 1.224612562803249594 ) ) ;
#30323 = AXIS2_PLACEMENT_3D ( 'NONE', #13281, #20449, #1722 ) ;
#30324 = CARTESIAN_POINT ( 'NONE',  ( 57.04171473382086077, 0.7493275531345221507, -1.778946371510476077 ) ) ;
#30326 = DIRECTION ( 'NONE',  ( 0.000000000000000000, 1.000000000000000000, 3.491481338843130594E-15 ) ) ;
#30325 = CARTESIAN_POINT ( 'NONE',  ( 58.75000000000000711, 1.470078920827434965, 1.470078920828533420 ) ) ;
#30327 = AXIS2_PLACEMENT_3D ( 'NONE', #7195, #26669, #26195 ) ;
#30328 = CARTESIAN_POINT ( 'NONE',  ( 61.25000000000003553, -0.9999999999993586242, -1.655766640118113031 ) ) ;
#30329 = DIRECTION ( 'NONE',  ( 0.000000000000000000, -1.000000000000000000, 0.000000000000000000 ) ) ;
#30330 = DIRECTION ( 'NONE',  ( 0.000000000000000000, 0.000000000000000000, 1.000000000000000000 ) ) ;
#30331 = EDGE_LOOP ( 'NONE', ( #26192, #15427, #28685, #8157 ) ) ;
#30332 = EDGE_CURVE ( 'NONE', #11640, #12796, #28200, .T. ) ;
#30333 = DIRECTION ( 'NONE',  ( -1.000000000000000000, -0.000000000000000000, -0.000000000000000000 ) ) ;
#30334 = EDGE_LOOP ( 'NONE', ( #29638, #8671, #19937, #26016, #8365, #15752 ) ) ;
#30335 = CARTESIAN_POINT ( 'NONE',  ( -59.18029295939872014, -2.385974606001367349, 1.241011964822052782 ) ) ;
#30336 = AXIS2_PLACEMENT_3D ( 'NONE', #5304, #20830, #25878 ) ;
#30337 = ORIENTED_EDGE ( 'NONE', *, *, #8697, .F. ) ;
#30338 = ADVANCED_FACE ( 'NONE', ( #25945 ), #5453, .T. ) ;
#30339 = CARTESIAN_POINT ( 'NONE',  ( 53.94136487687671178, 6.599443998687474000, 2.049999999999811529 ) ) ;
#30340 = CARTESIAN_POINT ( 'NONE',  ( -59.09585481156723574, -2.489203624310587504, 2.804704140674918911 ) ) ;
#30342 = LINE ( 'NONE', #15785, #22753 ) ;
#30341 = DIRECTION ( 'NONE',  ( 1.000000000000000000, 1.047444401652940007E-14, 0.000000000000000000 ) ) ;
#30343 = VERTEX_POINT ( 'NONE', #30380 ) ;
#30344 = CARTESIAN_POINT ( 'NONE',  ( 30.17845427745894682, 6.795635868401290303, -2.050000000000105516 ) ) ;
#30345 = DIRECTION ( 'NONE',  ( 3.491481338843133355E-15, 3.491481338843133355E-15, -1.000000000000000000 ) ) ;
#30346 = ORIENTED_EDGE ( 'NONE', *, *, #29219, .T. ) ;
#30348 = DIRECTION ( 'NONE',  ( -0.9993908270191184107, 0.03489949670185085034, 3.491481338843133355E-15 ) ) ;
#30347 = FACE_OUTER_BOUND ( 'NONE', #9507, .T. ) ;
#30349 = CARTESIAN_POINT ( 'NONE',  ( 48.30000000000001847, 2.428612866367529932E-14, 0.000000000000000000 ) ) ;
#30350 = EDGE_CURVE ( 'NONE', #20749, #7153, #1395, .T. ) ;
#30351 = ORIENTED_EDGE ( 'NONE', *, *, #23923, .T. ) ;
#30352 = CARTESIAN_POINT ( 'NONE',  ( -36.11780688638203429, 5.377732434016818885, -0.5657657146887259403 ) ) ;
#30353 = EDGE_CURVE ( 'NONE', #6738, #8886, #22643, .T. ) ;
#30354 = CARTESIAN_POINT ( 'NONE',  ( 58.65263613458538572, 1.792763816755340356, -0.5494533739919623683 ) ) ;
#30355 = TOROIDAL_SURFACE ( 'NONE', #16727, 1.975000000000001865, 0.1000000000000000056 ) ;
#30356 = B_SPLINE_CURVE_WITH_KNOTS ( 'NONE', 3,
 ( #3497, #15978, #28175, #25180, #21069, #18071, #20606, #27714, #25640, #1568, #13745, #20902, #30238, #5865, #16148, #30532, #8838, #6180, #18533, #6034, #6490 ),
 .UNSPECIFIED., .F., .F.,
 ( 4, 2, 2, 1, 2, 2, 1, 1, 2, 2, 2, 4 ),
 ( 0.5844128917508384369, 0.6883096688131545848, 0.7402580573443117151, 0.7467516059107093263, 0.7499983801939079653, 0.7516217673355072293, 0.7532451544771066043, 0.7662322516098910574, 0.7922064458754600746, 0.8441548344065958887, 0.8961032229377317027, 1.000000000000000000 ),
 .UNSPECIFIED. ) ;
#30357 = DIRECTION ( 'NONE',  ( -2.095850865446309212E-30, -1.000000000000000000, -2.891205793294679411E-15 ) ) ;
#30358 = DIRECTION ( 'NONE',  ( 0.000000000000000000, 0.000000000000000000, -1.000000000000000000 ) ) ;
#30359 = DIRECTION ( 'NONE',  ( 1.054009200593503061E-14, 0.000000000000000000, 1.000000000000000000 ) ) ;
#30360 = CARTESIAN_POINT ( 'NONE',  ( 41.48619405471883681, -151.3359592902621955, -1.550000000000163469 ) ) ;
#30361 = CARTESIAN_POINT ( 'NONE',  ( -57.61042740578359656, -2.936324665650192234, -2.606018187048508850 ) ) ;
#30362 = CARTESIAN_POINT ( 'NONE',  ( -56.65835481156722864, -3.238593381231841928, -2.874284765127022467 ) ) ;
#30363 = EDGE_CURVE ( 'NONE', #4089, #28405, #389, .T. ) ;
#30364 = DIRECTION ( 'NONE',  ( 0.000000000000000000, -1.000000000000000000, 2.168404344971008128E-16 ) ) ;
#30366 = CIRCLE ( 'NONE', #27850, 0.1000000000000028644 ) ;
#30365 = CARTESIAN_POINT ( 'NONE',  ( 58.66122797211820483, -1.875002085569718258, -0.01642207461113097053 ) ) ;
#30367 = CARTESIAN_POINT ( 'NONE',  ( 58.75000000000000711, 1.800471618824943221, -1.039502773795712987 ) ) ;
#30368 = EDGE_CURVE ( 'NONE', #16027, #19841, #19125, .T. ) ;
#30369 = ORIENTED_EDGE ( 'NONE', *, *, #10974, .F. ) ;
#30370 = CARTESIAN_POINT ( 'NONE',  ( 63.50000000000000000, -0.7500000000000000000, -1.988246715074021731 ) ) ;
#30371 = VERTEX_POINT ( 'NONE', #9179 ) ;
#30372 = EDGE_CURVE ( 'NONE', #9980, #24584, #28646, .T. ) ;
#30373 = SURFACE_STYLE_USAGE ( .BOTH. , #16293 ) ;
#30375 = DIRECTION ( 'NONE',  ( 0.000000000000000000, -2.168404344971008868E-16, -1.000000000000000000 ) ) ;
#30374 = CARTESIAN_POINT ( 'NONE',  ( -59.69999999999997442, 8.366749974758454467E-15, -2.120534355533670266E-13 ) ) ;
#30376 = ORIENTED_EDGE ( 'NONE', *, *, #16787, .T. ) ;
#30377 = ORIENTED_EDGE ( 'NONE', *, *, #16789, .T. ) ;
#30378 = CARTESIAN_POINT ( 'NONE',  ( 50.40000000000001990, -0.6304760106459033064, -3.950000000000022826 ) ) ;
#30379 = DIRECTION ( 'NONE',  ( 0.000000000000000000, -0.3333333333333235449, 0.9428090415820667980 ) ) ;
#30381 = LINE ( 'NONE', #28003, #11987 ) ;
#30380 = CARTESIAN_POINT ( 'NONE',  ( -35.85663232820584057, 0.4576450603546802220, -5.200000000000000178 ) ) ;
#30382 =( BOUNDED_SURFACE ( )  B_SPLINE_SURFACE ( 3, 2, ( 
 ( #10102, #29263, #10248 ),
 ( #14834, #17543, #5504 ),
 ( #21697, #26563, #17233 ),
 ( #26741, #5330, #9654 ) ),
 .UNSPECIFIED., .F., .F., .F. ) 
 B_SPLINE_SURFACE_WITH_KNOTS ( ( 4, 4 ),
 ( 3, 3 ),
 ( 4.828596150434655954, 4.929762646526004488 ),
 ( 0.000000000000000000, 1.000000000000000000 ),
 .UNSPECIFIED. ) 
 GEOMETRIC_REPRESENTATION_ITEM ( )  RATIONAL_B_SPLINE_SURFACE ( (
 ( 1.000000000000000000, 0.6674753128239091504, 1.000000000000000000),
 ( 1.000000000000000000, 0.6556866267091900902, 1.000000000000000000),
 ( 1.000000000000000000, 0.6436549836476661568, 1.000000000000000000),
 ( 1.000000000000000000, 0.6314033579135635010, 1.000000000000000000) ) ) 
 REPRESENTATION_ITEM ( '' )  SURFACE ( )  );
#30383 = VERTEX_POINT ( 'NONE', #24359 ) ;
#30384 = CARTESIAN_POINT ( 'NONE',  ( -57.67292740578359656, -3.330682475591783209, -0.6830477631804108274 ) ) ;
#30385 = DIRECTION ( 'NONE',  ( 0.000000000000000000, 0.000000000000000000, 1.000000000000000000 ) ) ;
#30386 = APPLICATION_PROTOCOL_DEFINITION ( 'draft international standard', 'automotive_design', 1998, #31246 ) ;
#30387 = CARTESIAN_POINT ( 'NONE',  ( -59.36246495612066809, 2.315842144512513023, 1.288740169525656176 ) ) ;
#30388 = VERTEX_POINT ( 'NONE', #16448 ) ;
#30389 = CARTESIAN_POINT ( 'NONE',  ( -60.63452994616204705, -3.117691453623976816, 1.799999999999772671 ) ) ;
#30390 = CARTESIAN_POINT ( 'NONE',  ( -35.85663232820596846, 3.779372838781794641, -3.883777296072516094 ) ) ;
#30391 = DIRECTION ( 'NONE',  ( 0.000000000000000000, 0.000000000000000000, -1.000000000000000000 ) ) ;
#30392 = CARTESIAN_POINT ( 'NONE',  ( 61.25000000000000000, 1.960427193528887280, -0.3958853607737569114 ) ) ;
#30393 = CARTESIAN_POINT ( 'NONE',  ( -59.68658240507107138, -2.223882124562203799, 1.531065007683262591 ) ) ;
#30395 = CARTESIAN_POINT ( 'NONE',  ( 58.75000000000002132, 6.153735859711025284E-13, 3.111507638930570854E-58 ) ) ;
#30394 = DIRECTION ( 'NONE',  ( -1.000000000000000000, -2.586136946169074517E-16, 0.000000000000000000 ) ) ;
#30396 = CARTESIAN_POINT ( 'NONE',  ( -54.39999999999996305, -1.557046979865753356, -3.273565289175142556 ) ) ;
#30398 = CARTESIAN_POINT ( 'NONE',  ( 50.25000000000000000, 1.499837071477871042, 1.323060376182421782 ) ) ;
#30397 = DIRECTION ( 'NONE',  ( -1.000000000000000000, -0.000000000000000000, -0.000000000000000000 ) ) ;
#30399 = ADVANCED_FACE ( 'NONE', ( #24044 ), #14547, .F. ) ;
#30400 = ORIENTED_EDGE ( 'NONE', *, *, #30535, .T. ) ;
#30401 = AXIS2_PLACEMENT_3D ( 'NONE', #1340, #25881, #30462 ) ;
#30402 = CARTESIAN_POINT ( 'NONE',  ( -62.06598287454225726, -2.648582569373490347, -0.3347775276703480740 ) ) ;
#30403 = B_SPLINE_CURVE_WITH_KNOTS ( 'NONE', 3,
 ( #10984, #11132, #8740, #30290, #15877, #27917 ),
 .UNSPECIFIED., .F., .F.,
 ( 4, 2, 4 ),
 ( 0.000000000000000000, 0.4999999999999995559, 1.000000000000000000 ),
 .UNSPECIFIED. ) ;
#30404 = DIRECTION ( 'NONE',  ( -1.047444401652940007E-14, -8.673617379884032317E-15, -1.000000000000000000 ) ) ;
#30406 = CARTESIAN_POINT ( 'NONE',  ( -59.68054851456403753, -2.392282282077057065, -1.229557205448934099 ) ) ;
#30405 = CARTESIAN_POINT ( 'NONE',  ( 58.75000000000000000, 1.877732920581272946, 0.6121634413844393441 ) ) ;
#30407 = FACE_OUTER_BOUND ( 'NONE', #22814, .T. ) ;
#30408 = ORIENTED_EDGE ( 'NONE', *, *, #2445, .F. ) ;
#30409 = CARTESIAN_POINT ( 'NONE',  ( 53.31611809544275360, 8.197428291949846013, 2.049999999999814193 ) ) ;
#30410 = FACE_OUTER_BOUND ( 'NONE', #8874, .T. ) ;
#30411 =( BOUNDED_CURVE ( )  B_SPLINE_CURVE ( 3, ( #11700, #9500, #4714, #12018 ),
 .UNSPECIFIED., .F., .T. ) 
 B_SPLINE_CURVE_WITH_KNOTS ( ( 4, 4 ),
 ( 4.094114376165666869, 4.828985806059314712 ),
 .UNSPECIFIED. ) 
 CURVE ( )  GEOMETRIC_REPRESENTATION_ITEM ( )  RATIONAL_B_SPLINE_CURVE ( ( 1.000000000000000000, 0.9555010429016489448, 0.9555010429016489448, 1.000000000000000000 ) ) 
 REPRESENTATION_ITEM ( '' )  );
#30412 = EDGE_LOOP ( 'NONE', ( #26697, #5222 ) ) ;
#30413 = EDGE_LOOP ( 'NONE', ( #20632, #697, #25557, #12646 ) ) ;
#30414 = DIRECTION ( 'NONE',  ( 0.000000000000000000, 0.2008964009354141933, -0.9796124928211140670 ) ) ;
#30415 = CARTESIAN_POINT ( 'NONE',  ( 58.66107449606996482, 1.640741681271480124, -0.9081280691409446826 ) ) ;
#30416 = ORIENTED_EDGE ( 'NONE', *, *, #11359, .F. ) ;
#30417 = CARTESIAN_POINT ( 'NONE',  ( 23.28297127712496106, 6.056087685919490760, 1.949999999999917577 ) ) ;
#30418 = ADVANCED_FACE ( 'NONE', ( #2670 ), #26686, .T. ) ;
#30419 = VECTOR ( 'NONE', #8439, 1000.000000000000000 ) ;
#30420 = CARTESIAN_POINT ( 'NONE',  ( -55.76905989232411542, 2.023778652682505897E-14, -3.400000000000197975 ) ) ;
#30421 = ORIENTED_EDGE ( 'NONE', *, *, #20266, .F. ) ;
#30422 = VERTEX_POINT ( 'NONE', #21700 ) ;
#30423 = ORIENTED_EDGE ( 'NONE', *, *, #5441, .T. ) ;
#30424 = AXIS2_PLACEMENT_3D ( 'NONE', #28007, #1566, #6970 ) ;
#30425 = B_SPLINE_CURVE_WITH_KNOTS ( 'NONE', 3,
 ( #19661, #21570, #29143, #19805, #16663, #26455, #2224, #173, #9541, #9994 ),
 .UNSPECIFIED., .F., .F.,
 ( 4, 2, 2, 2, 4 ),
 ( 2.528772284819897467E-18, 9.757673230185597056E-05, 0.0001951534646037094746, 0.0002927301969055630328, 0.0003903069292074165639 ),
 .UNSPECIFIED. ) ;
#30426 = AXIS2_PLACEMENT_3D ( 'NONE', #4811, #2128, #9739 ) ;
#30427 = CARTESIAN_POINT ( 'NONE',  ( -56.68749999999996447, 1.962990915244749557, -3.400000000000192646 ) ) ;
#30428 = CARTESIAN_POINT ( 'NONE',  ( 58.73307976133189356, 0.5681412931396376820, -1.786904874454019465 ) ) ;
#30429 = CARTESIAN_POINT ( 'NONE',  ( 52.20711756518984714, -0.7499999999994533262, -1.718465885608440935 ) ) ;
#30430 = CARTESIAN_POINT ( 'NONE',  ( 69.20000000000003126, 1.401298464324817071E-42, -7.248315259438346108E-13 ) ) ;
#30431 = CARTESIAN_POINT ( 'NONE',  ( -59.43987571604603914, -2.221192970515155629, 1.449404383176176037 ) ) ;
#30433 = DIRECTION ( 'NONE',  ( 2.614381936396368743E-16, -0.2008964009354147762, 0.9796124928211139560 ) ) ;
#30432 = SURFACE_STYLE_FILL_AREA ( #18745 ) ;
#30434 = CARTESIAN_POINT ( 'NONE',  ( -54.49999999999997868, 8.366749974758489177E-15, -2.216533082070116467E-13 ) ) ;
#30435 = CARTESIAN_POINT ( 'NONE',  ( 59.00000000000002132, 1.401298464324817071E-42, -6.179921969752347932E-13 ) ) ;
#30436 = CARTESIAN_POINT ( 'NONE',  ( -59.69997404044342915, 2.118290196927814062, 1.750091561861647493 ) ) ;
#30437 = EDGE_CURVE ( 'NONE', #9147, #19884, #7986, .T. ) ;
#30438 = CARTESIAN_POINT ( 'NONE',  ( 57.00057550097274373, 0.8023623105721646720, 2.473098203180232879 ) ) ;
#30439 = CARTESIAN_POINT ( 'NONE',  ( 57.00000000000001421, 0.6999999999999999556, -2.452039967047845437 ) ) ;
#30440 = CARTESIAN_POINT ( 'NONE',  ( -59.29999999999998295, -0.6915043170233550196, 3.445813225535238278 ) ) ;
#30441 = VERTEX_POINT ( 'NONE', #29106 ) ;
#30442 = CARTESIAN_POINT ( 'NONE',  ( 58.75000000000002132, 6.153735859711025284E-13, 3.111507638930570854E-58 ) ) ;
#30443 = CARTESIAN_POINT ( 'NONE',  ( 58.66133336607565241, -0.9092995659213525261, 1.640092727267363770 ) ) ;
#30444 = ORIENTED_EDGE ( 'NONE', *, *, #2949, .F. ) ;
#30445 = DIRECTION ( 'NONE',  ( 0.000000000000000000, 1.000000000000000000, 0.000000000000000000 ) ) ;
#30446 = CARTESIAN_POINT ( 'NONE',  ( 58.75000000000002132, 6.153735859711025284E-13, 3.111507638930570854E-58 ) ) ;
#30448 = DIRECTION ( 'NONE',  ( 0.000000000000000000, 0.000000000000000000, -1.000000000000000000 ) ) ;
#30447 = CARTESIAN_POINT ( 'NONE',  ( -56.06249999999995737, -1.962990915244707368, -3.400000000000206413 ) ) ;
#30449 = EDGE_LOOP ( 'NONE', ( #31295, #14861, #10530, #8071 ) ) ;
#30450 = VERTEX_POINT ( 'NONE', #14222 ) ;
#30451 = CARTESIAN_POINT ( 'NONE',  ( 51.70000000000000995, -4.020776289669855785, -2.234582293948758291 ) ) ;
#30452 = ORIENTED_EDGE ( 'NONE', *, *, #26346, .T. ) ;
#30453 = CARTESIAN_POINT ( 'NONE',  ( 51.19148447764911225, 0.9872860527330414859, -1.295557643792421443 ) ) ;
#30454 = EDGE_CURVE ( 'NONE', #5258, #25335, #7423, .T. ) ;
#30455 = CARTESIAN_POINT ( 'NONE',  ( 51.80000000000001847, -3.726179070414207928, -1.100000000000000089 ) ) ;
#30456 = ORIENTED_EDGE ( 'NONE', *, *, #24711, .F. ) ;
#30457 = CARTESIAN_POINT ( 'NONE',  ( 24.79111845547821247, 5.500805180497733815, -2.050000000000085976 ) ) ;
#30458 = AXIS2_PLACEMENT_3D ( 'NONE', #30964, #6432, #18789 ) ;
#30459 = CARTESIAN_POINT ( 'NONE',  ( -61.34999999999997300, -2.600201727571727517, 0.4583662226975599441 ) ) ;
#30460 = CARTESIAN_POINT ( 'NONE',  ( -54.48571443722132557, -2.918663338619467140, -2.077054936585725819 ) ) ;
#30461 = ORIENTED_EDGE ( 'NONE', *, *, #7127, .T. ) ;
#30462 = DIRECTION ( 'NONE',  ( 1.047444401652940007E-14, 0.000000000000000000, 1.000000000000000000 ) ) ;
#30463 = LINE ( 'NONE', #3877, #30618 ) ;
#30464 = CARTESIAN_POINT ( 'NONE',  ( 57.04415282905778639, -0.8156862745098041323, -2.468735688885368873 ) ) ;
#30465 = EDGE_CURVE ( 'NONE', #14068, #30753, #26569, .T. ) ;
#30466 = CARTESIAN_POINT ( 'NONE',  ( 53.60047708782985154, 7.640852521089521510, -1.861455469535500340 ) ) ;
#30467 = CARTESIAN_POINT ( 'NONE',  ( 58.64999999999999858, 1.253243060177670287, 1.394635017528978782 ) ) ;
#30468 = CARTESIAN_POINT ( 'NONE',  ( 41.48619405471885102, -151.3359592902622239, 1.949999999999835865 ) ) ;
#30469 = CARTESIAN_POINT ( 'NONE',  ( 57.04534525700438508, 0.7498361808180106225, -1.778489416763646025 ) ) ;
#30471 = DIRECTION ( 'NONE',  ( -1.047444401652940007E-14, 0.000000000000000000, -1.000000000000000000 ) ) ;
#30470 = CARTESIAN_POINT ( 'NONE',  ( -60.83824777938932726, -2.565600044710441008, 0.8496564960046820714 ) ) ;
#30472 = CARTESIAN_POINT ( 'NONE',  ( 22.04321716858593661, 7.679566743993218481, -2.050000000000076650 ) ) ;
#30473 = CYLINDRICAL_SURFACE ( 'NONE', #6433, 0.2500000000000000000 ) ;
#30474 = ADVANCED_FACE ( 'NONE', ( #26420 ), #28949, .T. ) ;
#30475 = CARTESIAN_POINT ( 'NONE',  ( 51.45655683570191741, -0.9591657938390834026, 1.611094652690528095 ) ) ;
#30476 = EDGE_CURVE ( 'NONE', #26264, #3572, #9504, .T. ) ;
#30477 = AXIS2_PLACEMENT_3D ( 'NONE', #10864, #19918, #25122 ) ;
#30478 = ORIENTED_EDGE ( 'NONE', *, *, #6158, .F. ) ;
#30479 = EDGE_CURVE ( 'NONE', #22240, #2603, #12514, .T. ) ;
#30480 = CARTESIAN_POINT ( 'NONE',  ( 54.17609772354683884, 5.677826690772942442, -2.050000000000186784 ) ) ;
#30481 = EDGE_LOOP ( 'NONE', ( #3704, #12786, #26089, #24342 ) ) ;
#30482 = CARTESIAN_POINT ( 'NONE',  ( 51.58871481136676351, -3.753741921856246222, 1.652517360673975588 ) ) ;
#30483 = ORIENTED_EDGE ( 'NONE', *, *, #30988, .F. ) ;
#30484 = CARTESIAN_POINT ( 'NONE',  ( 53.55869261961972683, 7.702978059423483792, 2.049999999999813305 ) ) ;
#30485 = CARTESIAN_POINT ( 'NONE',  ( -57.78335481156724285, 3.238593381231847257, 2.874284765127022911 ) ) ;
#30487 = LINE ( 'NONE', #13703, #6580 ) ;
#30486 = CARTESIAN_POINT ( 'NONE',  ( 61.25000000000003553, -1.039502773796089796, -1.650471618824325359 ) ) ;
#30488 = ORIENTED_EDGE ( 'NONE', *, *, #19091, .T. ) ;
#30489 = CARTESIAN_POINT ( 'NONE',  ( 26.00383130008247079, 5.312289655708096525, -2.050000000000089972 ) ) ;
#30490 = LINE ( 'NONE', #24465, #15056 ) ;
#30491 = EDGE_CURVE ( 'NONE', #15816, #17715, #21131, .T. ) ;
#30492 = ORIENTED_EDGE ( 'NONE', *, *, #22977, .F. ) ;
#30494 = DIRECTION ( 'NONE',  ( 0.000000000000000000, 1.000000000000000000, 0.000000000000000000 ) ) ;
#30493 = CYLINDRICAL_SURFACE ( 'NONE', #31266, 1.250000000000000222 ) ;
#30495 = DIRECTION ( 'NONE',  ( 0.000000000000000000, 1.000000000000000000, 0.000000000000000000 ) ) ;
#30496 = ORIENTED_EDGE ( 'NONE', *, *, #18817, .F. ) ;
#30497 = CARTESIAN_POINT ( 'NONE',  ( -36.23324115033479131, 5.027926281937889819, -1.353187539901933967 ) ) ;
#30498 = CARTESIAN_POINT ( 'NONE',  ( 58.74999981196283017, 1.909245389982500818, -0.4235863532939667664 ) ) ;
#30499 = CARTESIAN_POINT ( 'NONE',  ( 56.99139336475067807, 0.7078862301243328270, 1.763423818528686349 ) ) ;
#30501 = CARTESIAN_POINT ( 'NONE',  ( -58.57202994616204705, 2.078460969082646770, 3.599999999999799805 ) ) ;
#30500 = VECTOR ( 'NONE', #19451, 1000.000000000000000 ) ;
#30502 = CONICAL_SURFACE ( 'NONE', #13287, 4.299999999999998934, 0.7853981633974466137 ) ;
#30503 = ADVANCED_FACE ( 'NONE', ( #14698 ), #4419, .T. ) ;
#30504 = CARTESIAN_POINT ( 'NONE',  ( 60.99941465888825576, -0.5621240721069680202, -1.858165151418244010 ) ) ;
#30505 = CARTESIAN_POINT ( 'NONE',  ( -58.92292740578360366, 2.256877952708275625, -2.542931754211918527 ) ) ;
#30506 = EDGE_CURVE ( 'NONE', #5154, #16857, #11514, .T. ) ;
#30507 = CARTESIAN_POINT ( 'NONE',  ( -54.49999999999996447, 1.557046979865791991, -3.273565289175131454 ) ) ;
#30508 = EDGE_CURVE ( 'NONE', #24848, #1900, #27104, .T. ) ;
#30509 = B_SPLINE_CURVE_WITH_KNOTS ( 'NONE', 3,
 ( #29424, #7137, #7733, #28969, #12638, #4733, #24065, #2378, #21717, #8, #19333, #7277, #16947, #26591, #4901, #14566, #24230, #2540, #12191 ),
 .UNSPECIFIED., .F., .F.,
 ( 4, 3, 3, 3, 3, 3, 4 ),
 ( 0.000000000000000000, 1.590918590077522167E-05, 3.217562587127302352E-05, 4.946895718673912572E-05, 6.849224166005159653E-05, 8.924830576836555271E-05, 9.321254545577940852E-05 ),
 .UNSPECIFIED. ) ;
#30510 = EDGE_CURVE ( 'NONE', #15123, #9856, #14373, .T. ) ;
#30511 = CARTESIAN_POINT ( 'NONE',  ( 58.45000000000001705, -0.7500000000000000000, 1.745709025009609228 ) ) ;
#30512 = DIRECTION ( 'NONE',  ( -0.5633368246415004776, -0.8262273428075539439, 0.000000000000000000 ) ) ;
#30513 = CARTESIAN_POINT ( 'NONE',  ( -77.28999999999996362, -0.2499224661714871121, -0.006225825468447511619 ) ) ;
#30514 = ORIENTED_EDGE ( 'NONE', *, *, #17955, .F. ) ;
#30515 = CARTESIAN_POINT ( 'NONE',  ( -57.18749999999997868, 1.962990915244718915, 3.399999999999805844 ) ) ;
#30516 = ORIENTED_EDGE ( 'NONE', *, *, #2655, .T. ) ;
#30517 = DIRECTION ( 'NONE',  ( 0.000000000000000000, -0.2008964009354147484, 0.9796124928211138450 ) ) ;
#30518 = AXIS2_PLACEMENT_3D ( 'NONE', #18476, #28282, #6128 ) ;
#30520 = CARTESIAN_POINT ( 'NONE',  ( 58.74154451056426751, -1.390058629627632936, 1.258335925860512461 ) ) ;
#30519 = DIRECTION ( 'NONE',  ( 1.000000000000000000, 3.053848253006669023E-16, -2.042510438544995415E-16 ) ) ;
#30521 = ORIENTED_EDGE ( 'NONE', *, *, #8821, .F. ) ;
#30522 = EDGE_LOOP ( 'NONE', ( #17973, #18771, #18927, #9003 ) ) ;
#30523 = DIRECTION ( 'NONE',  ( 1.000000000000000000, 1.047444401652940007E-14, 0.000000000000000000 ) ) ;
#30524 = DIRECTION ( 'NONE',  ( -1.000000000000000000, 1.219044193948983948E-29, -3.491481338843133355E-15 ) ) ;
#30526 = DIRECTION ( 'NONE',  ( 1.000000000000000000, -0.000000000000000000, -0.000000000000000000 ) ) ;
#30525 = CARTESIAN_POINT ( 'NONE',  ( -61.13452994616202574, 2.093608279459375190E-14, -3.600000000000216804 ) ) ;
#30527 = ORIENTED_EDGE ( 'NONE', *, *, #3320, .T. ) ;
#30528 = CARTESIAN_POINT ( 'NONE',  ( -56.36042740578360366, -0.7887156198831599685, 3.845940847736173840 ) ) ;
#30529 = CIRCLE ( 'NONE', #11319, 2.525000000001611511 ) ;
#30530 = DIRECTION ( 'NONE',  ( 0.000000000000000000, 0.000000000000000000, -1.000000000000000000 ) ) ;
#30531 = APPLICATION_PROTOCOL_DEFINITION ( 'draft international standard', 'automotive_design', 1998, #4261 ) ;
#30532 = CARTESIAN_POINT ( 'NONE',  ( 52.88901726360196420, 4.646846922877157837, -1.580885370238881427 ) ) ;
#30533 = DIRECTION ( 'NONE',  ( 0.000000000000000000, -1.000000000000000000, -1.734723475976807094E-15 ) ) ;
#30534 = CARTESIAN_POINT ( 'NONE',  ( -54.49999999999997868, 1.549598385535858380, -4.064203588144675194 ) ) ;
#30535 = EDGE_CURVE ( 'NONE', #27508, #14261, #15555, .T. ) ;
#30536 = EDGE_CURVE ( 'NONE', #10254, #24129, #21572, .T. ) ;
#30537 = CARTESIAN_POINT ( 'NONE',  ( 57.02118883257515591, -0.7413508443325595998, 1.786034507790101866 ) ) ;
#30538 = ADVANCED_FACE ( 'NONE', ( #15476 ), #18619, .F. ) ;
#30539 = VERTEX_POINT ( 'NONE', #8042 ) ;
#30540 = CARTESIAN_POINT ( 'NONE',  ( -35.98994760229851408, 3.426725948577779679, -3.937891352654224963 ) ) ;
#30541 = DIRECTION ( 'NONE',  ( 0.000000000000000000, 0.000000000000000000, 1.000000000000000000 ) ) ;
#30542 = VECTOR ( 'NONE', #1410, 1000.000000000000000 ) ;
#30543 = CARTESIAN_POINT ( 'NONE',  ( 51.80000000000002558, -3.936726248589973221, 1.145507068359712388 ) ) ;
#30544 = DIRECTION ( 'NONE',  ( 0.000000000000000000, -0.9996898646859344595, -0.02490330187381124480 ) ) ;
#30546 = DIRECTION ( 'NONE',  ( 1.000000000000000000, 0.000000000000000000, 0.000000000000000000 ) ) ;
#30545 = DIRECTION ( 'NONE',  ( 0.000000000000000000, 0.2008964009354148039, -0.9796124928211139560 ) ) ;
#30547 = PRODUCT_DEFINITION_SHAPE ( 'NONE', 'NONE',  #31335 ) ;
#30548 = CIRCLE ( 'NONE', #16929, 0.2000000000000000944 ) ;
#30549 = CARTESIAN_POINT ( 'NONE',  ( 47.49367672221800518, -4.280384112421974585, -1.378579207634685222 ) ) ;
#30551 = CARTESIAN_POINT ( 'NONE',  ( 60.97408713704744088, -0.7545809820792435119, 1.439897579195098309 ) ) ;
#30550 = CARTESIAN_POINT ( 'NONE',  ( 52.06628335902946247, -0.5434431642975677823, -1.996089927833914146 ) ) ;
#30552 = VERTEX_POINT ( 'NONE', #12931 ) ;
#30553 = CARTESIAN_POINT ( 'NONE',  ( -62.06710100716625789, -2.624587610216423172, -0.3274367013645053115 ) ) ;
#30554 =( BOUNDED_SURFACE ( )  B_SPLINE_SURFACE ( 3, 2, ( 
 ( #19898, #24060, #15136 ),
 ( #24793, #3101, #10550 ),
 ( #22428, #8316, #13069 ),
 ( #7272, #29698, #571 ),
 ( #12902, #720, #20227 ),
 ( #26585, #894, #17987 ),
 ( #29855, #15290, #17684 ),
 ( #5638, #14389, #22284 ),
 ( #10379, #1047, #8169 ),
 ( #3430, #17838, #5792 ) ),
 .UNSPECIFIED., .F., .F., .F. ) 
 B_SPLINE_SURFACE_WITH_KNOTS ( ( 4, 2, 2, 2, 4 ),
 ( 3, 3 ),
 ( -5.421010862427522170E-20, 0.0003537438758377275429, 0.0007074877516754551942, 0.001061231627513182845, 0.001414975503350910388 ),
 ( 0.000000000000000000, 1.000000000000000000 ),
 .UNSPECIFIED. ) 
 GEOMETRIC_REPRESENTATION_ITEM ( )  RATIONAL_B_SPLINE_SURFACE ( (
 ( 1.000000000000000000, 0.7154752000627009334, 1.000000000000000000),
 ( 1.000000000000000000, 0.7154106121887914282, 1.000000000000000000),
 ( 1.000000000000000000, 0.7173719856081617330, 1.000000000000000000),
 ( 1.000000000000000000, 0.7229186815313275449, 1.000000000000000000),
 ( 1.000000000000000000, 0.7264660769266189089, 1.000000000000000000),
 ( 1.000000000000000000, 0.7305267549325924481, 1.000000000000000000),
 ( 1.000000000000000000, 0.7309418327394059389, 1.000000000000000000),
 ( 1.000000000000000000, 0.7246992783962609153, 1.000000000000000000),
 ( 1.000000000000000000, 0.7179850693091097691, 1.000000000000000000),
 ( 1.000000000000000000, 0.7071067811865482389, 1.000000000000000000) ) ) 
 REPRESENTATION_ITEM ( '' )  SURFACE ( )  );
#30555 = CARTESIAN_POINT ( 'NONE',  ( 47.10000000000002274, -4.179189514726506793, -0.9000000000000000222 ) ) ;
#30557 = DIRECTION ( 'NONE',  ( -1.000000000000000000, 0.000000000000000000, 1.047444401652940007E-14 ) ) ;
#30556 = FACE_OUTER_BOUND ( 'NONE', #19008, .T. ) ;
#30558 = CARTESIAN_POINT ( 'NONE',  ( 15.44631504820154433, -4.878538113278835020, 1.812957040858152569 ) ) ;
#30559 = CONICAL_SURFACE ( 'NONE', #24509, 1.600000000000000533, 0.7853981633974497223 ) ;
#30560 = ORIENTED_EDGE ( 'NONE', *, *, #12073, .T. ) ;
#30561 = CARTESIAN_POINT ( 'NONE',  ( 53.60227722476025747, 4.617096236911464757, 2.049999999999812861 ) ) ;
#30562 = LINE ( 'NONE', #8870, #3723 ) ;
#30563 = VERTEX_POINT ( 'NONE', #20253 ) ;
#30564 = CIRCLE ( 'NONE', #24492, 1.524417381223824197 ) ;
#30565 = CARTESIAN_POINT ( 'NONE',  ( -54.49999999999999289, -1.500000000000006883, 4.029888335921739895 ) ) ;
#30566 = VERTEX_POINT ( 'NONE', #29268 ) ;
#30567 = CARTESIAN_POINT ( 'NONE',  ( -59.69999999999996021, -2.194112688547747325, -2.851241005161186504 ) ) ;
#30568 = ORIENTED_EDGE ( 'NONE', *, *, #10429, .T. ) ;
#30569 = CARTESIAN_POINT ( 'NONE',  ( -54.75952994616206837, -4.643455692769931152E-15, 3.599999999999804245 ) ) ;
#30570 = CARTESIAN_POINT ( 'NONE',  ( -57.95655989232411542, 1.962990915244748891, -3.400000000000197087 ) ) ;
#30571 = ORIENTED_EDGE ( 'NONE', *, *, #24738, .F. ) ;
#30572 = TOROIDAL_SURFACE ( 'NONE', #17429, -24.59258869922086888, 30.00000000000000000 ) ;
#30573 = VERTEX_POINT ( 'NONE', #3459 ) ;
#30574 = PRODUCT_DEFINITION_SHAPE ( 'NONE', 'NONE',  #10272 ) ;
#30575 = EDGE_CURVE ( 'NONE', #25126, #11599, #12746, .T. ) ;
#30576 = ORIENTED_EDGE ( 'NONE', *, *, #26993, .T. ) ;
#30577 = EDGE_CURVE ( 'NONE', #4452, #1083, #6976, .T. ) ;
#30578 = CARTESIAN_POINT ( 'NONE',  ( -58.43749999999997158, -3.925981830489445379, -2.215933297149796442E-13 ) ) ;
#30579 = EDGE_CURVE ( 'NONE', #4844, #355, #1925, .T. ) ;
#30580 = CARTESIAN_POINT ( 'NONE',  ( 56.95000000000001705, -0.7227197132926967971, 2.497551541979256218 ) ) ;
#30581 = CARTESIAN_POINT ( 'NONE',  ( 22.58884618656103882, 6.655783678991572749, -1.425000000000078648 ) ) ;
#30582 = DIRECTION ( 'NONE',  ( 1.000000000000000000, 5.172273892338149033E-16, 0.000000000000000000 ) ) ;
#30583 = AXIS2_PLACEMENT_3D ( 'NONE', #13792, #1948, #28232 ) ;
#30584 = CARTESIAN_POINT ( 'NONE',  ( 57.04413099161754985, 0.7497394063391640273, 2.421432380119032501 ) ) ;
#30586 = CARTESIAN_POINT ( 'NONE',  ( -58.06249999999996447, -0.7533615035078129463, 3.673546848079175309 ) ) ;
#30585 = FILL_AREA_STYLE_COLOUR ( '', #23124 ) ;
#30587 =( LENGTH_UNIT ( ) NAMED_UNIT ( * ) SI_UNIT ( .MILLI., .METRE. ) );
#30588 = CARTESIAN_POINT ( 'NONE',  ( -59.61160122551025609, 2.340542558125672912, -1.243912201914818771 ) ) ;
#30589 = CARTESIAN_POINT ( 'NONE',  ( 15.39414421509789932, 5.035245099686891379, -1.330662535294792281 ) ) ;
#30590 = EDGE_CURVE ( 'NONE', #6559, #20284, #17109, .T. ) ;
#30591 = FACE_OUTER_BOUND ( 'NONE', #13990, .T. ) ;
#30592 =( BOUNDED_SURFACE ( )  B_SPLINE_SURFACE ( 3, 2, ( 
 ( #6417, #25729, #4037 ),
 ( #29566, #13356, #23049 ),
 ( #22167, #1341, #456 ),
 ( #24677, #11014, #606 ) ),
 .UNSPECIFIED., .F., .F., .F. ) 
 B_SPLINE_SURFACE_WITH_KNOTS ( ( 4, 4 ),
 ( 3, 3 ),
 ( 4.041453792691655167, 4.300872134317203610 ),
 ( 0.000000000000000000, 1.000000000000000000 ),
 .UNSPECIFIED. ) 
 GEOMETRIC_REPRESENTATION_ITEM ( )  RATIONAL_B_SPLINE_SURFACE ( (
 ( 1.000000000000000000, 0.8699658093904940603, 1.000000000000000000),
 ( 1.000000000000000000, 0.8538860448759170163, 1.000000000000000000),
 ( 1.000000000000000000, 0.8356979842195467745, 1.000000000000000000),
 ( 1.000000000000000000, 0.8156258140602883344, 1.000000000000000000) ) ) 
 REPRESENTATION_ITEM ( '' )  SURFACE ( )  );
#30593 = CARTESIAN_POINT ( 'NONE',  ( 47.00000000000000711, 7.037983420167852921E-14, -4.500000000000199840 ) ) ;
#30594 = CIRCLE ( 'NONE', #19509, 0.1000000000000000472 ) ;
#30595 = CARTESIAN_POINT ( 'NONE',  ( 49.04999999999999716, 1.401298464324817071E-42, -2.875000000000512923 ) ) ;
#30596 = ORIENTED_EDGE ( 'NONE', *, *, #14517, .F. ) ;
#30598 = DIRECTION ( 'NONE',  ( 0.000000000000000000, -0.2008964009354162750, 0.9796124928211136229 ) ) ;
#30597 = DIRECTION ( 'NONE',  ( -1.000000000000000000, -3.054025858079668409E-16, 2.042474015755241579E-16 ) ) ;
#30599 = FILL_AREA_STYLE_COLOUR ( '', #23071 ) ;
#30600 = VERTEX_POINT ( 'NONE', #12465 ) ;
#30601 = SPHERICAL_SURFACE ( 'NONE', #2771, 0.05000000000000000278 ) ;
#30602 = FACE_OUTER_BOUND ( 'NONE', #1517, .T. ) ;
#30603 = CARTESIAN_POINT ( 'NONE',  ( -55.19702994616203284, -2.078460969082631227, -3.600000000000202593 ) ) ;
#30604 = EDGE_LOOP ( 'NONE', ( #29630, #13167, #23427 ) ) ;
#30605 = ORIENTED_EDGE ( 'NONE', *, *, #13044, .T. ) ;
#30606 = AXIS2_PLACEMENT_3D ( 'NONE', #14715, #5361, #10124 ) ;
#30607 = DIRECTION ( 'NONE',  ( 0.000000000000000000, 0.000000000000000000, -1.000000000000000000 ) ) ;
#30608 = ORIENTED_EDGE ( 'NONE', *, *, #30577, .F. ) ;
#30609 = CIRCLE ( 'NONE', #19004, 4.000000000000022204 ) ;
#30610 = CARTESIAN_POINT ( 'NONE',  ( 58.75000000000003553, -1.652371589363308413, 1.066009655020056845 ) ) ;
#30611 = CARTESIAN_POINT ( 'NONE',  ( 48.00000000000002842, -4.291790910095608425, 1.352971095042313499 ) ) ;
#30612 = ORIENTED_EDGE ( 'NONE', *, *, #17955, .T. ) ;
#30613 = CARTESIAN_POINT ( 'NONE',  ( 22.10122560051033602, 7.779108733371300488, -2.050000000000076206 ) ) ;
#30614 = AXIS2_PLACEMENT_3D ( 'NONE', #8634, #28432, #1989 ) ;
#30615 = CARTESIAN_POINT ( 'NONE',  ( -59.92928932188130631, 2.138123341857387114E-15, 5.538933845919563674E-16 ) ) ;
#30616 = ORIENTED_EDGE ( 'NONE', *, *, #26286, .F. ) ;
#30617 = ORIENTED_EDGE ( 'NONE', *, *, #19294, .T. ) ;
#30618 = VECTOR ( 'NONE', #1503, 1000.000000000000000 ) ;
#30619 = EDGE_CURVE ( 'NONE', #14261, #7542, #25695, .T. ) ;
#30620 = CARTESIAN_POINT ( 'NONE',  ( 51.80000000000002558, -4.319730106884873244, 1.256953381662055724 ) ) ;
#30621 = VECTOR ( 'NONE', #28656, 1000.000000000000114 ) ;
#30622 = EDGE_CURVE ( 'NONE', #2736, #15656, #27201, .T. ) ;
#30623 = CARTESIAN_POINT ( 'NONE',  ( -62.09999999999997300, -2.636465585633694264, 0.1493792525119592707 ) ) ;
#30624 = CARTESIAN_POINT ( 'NONE',  ( 56.95606009725792518, -0.7486802684473473635, -2.489875068279050918 ) ) ;
#30625 = CARTESIAN_POINT ( 'NONE',  ( 15.18463186935387021, 2.199885893005444348, 4.939696249117986326 ) ) ;
#30626 = CARTESIAN_POINT ( 'NONE',  ( -59.29999999999997584, 2.330309927981285032E-15, 4.253626757584724400E-16 ) ) ;
#30627 = DIRECTION ( 'NONE',  ( 0.000000000000000000, 0.000000000000000000, -1.000000000000000000 ) ) ;
#30629 = CARTESIAN_POINT ( 'NONE',  ( 58.65000000000003411, -1.793030239489117994, -0.5493518053820871661 ) ) ;
#30628 = DIRECTION ( 'NONE',  ( 1.000000000000000000, 9.742518634745087578E-17, -4.338815227902166479E-17 ) ) ;
#30630 = AXIS2_PLACEMENT_3D ( 'NONE', #7179, #13835, #21763 ) ;
#30631 = DIRECTION ( 'NONE',  ( -1.000000000000000000, 0.000000000000000000, 0.000000000000000000 ) ) ;
#30632 = CIRCLE ( 'NONE', #26079, 0.1000000000000000472 ) ;
#30633 = CARTESIAN_POINT ( 'NONE',  ( -55.99999999999997868, 3.673546848079180638, 0.7533615035078075062 ) ) ;
#30634 = ADVANCED_FACE ( 'NONE', ( #17863 ), #3132, .F. ) ;
#30636 = CYLINDRICAL_SURFACE ( 'NONE', #28440, 2.000000000000000000 ) ;
#30635 = AXIS2_PLACEMENT_3D ( 'NONE', #19409, #9894, #396 ) ;
#30637 = FACE_OUTER_BOUND ( 'NONE', #4054, .T. ) ;
#30638 = CIRCLE ( 'NONE', #13422, 160.1997717543138720 ) ;
#30639 = VERTEX_POINT ( 'NONE', #16264 ) ;
#30640 = AXIS2_PLACEMENT_3D ( 'NONE', #689, #17956, #17653 ) ;
#30641 = CIRCLE ( 'NONE', #21068, 2.700000000000000178 ) ;
#30642 = ORIENTED_EDGE ( 'NONE', *, *, #8113, .T. ) ;
#30643 = VERTEX_POINT ( 'NONE', #3914 ) ;
#30644 = CIRCLE ( 'NONE', #1828, 0.2500000000000000000 ) ;
#30645 = CARTESIAN_POINT ( 'NONE',  ( 51.41454121074928452, -3.877603133525080903, 1.337216932410616010 ) ) ;
#30646 = ORIENTED_EDGE ( 'NONE', *, *, #3366, .F. ) ;
#30647 = VECTOR ( 'NONE', #8321, 1000.000000000000000 ) ;
#30648 = CARTESIAN_POINT ( 'NONE',  ( 52.80835374156199435, 4.037528258991556207, 2.049999999999815969 ) ) ;
#30649 = CARTESIAN_POINT ( 'NONE',  ( -58.53335481156722864, 3.238593381231847257, 2.874284765127022911 ) ) ;
#30650 = CARTESIAN_POINT ( 'NONE',  ( -35.85663232820579793, 4.018128179617487916, 3.618665901676695107 ) ) ;
#30651 = ORIENTED_EDGE ( 'NONE', *, *, #686, .F. ) ;
#30652 = VERTEX_POINT ( 'NONE', #8974 ) ;
#30653 = FACE_OUTER_BOUND ( 'NONE', #10992, .T. ) ;
#30654 = VERTEX_POINT ( 'NONE', #15790 ) ;
#30655 = FACE_OUTER_BOUND ( 'NONE', #2443, .T. ) ;
#30656 = VERTEX_POINT ( 'NONE', #11336 ) ;
#30658 = CARTESIAN_POINT ( 'NONE',  ( -60.49999999999997868, 1.656632322739229403E-15, 1.870925083934595927E-15 ) ) ;
#30657 = CARTESIAN_POINT ( 'NONE',  ( 47.00000000000002132, 1.391941090707534023, 3.750000000000022649 ) ) ;
#30659 = CIRCLE ( 'NONE', #27710, 3.399999999999999911 ) ;
#30660 = CARTESIAN_POINT ( 'NONE',  ( -55.95655989232413674, -3.399999999999990585, -2.144552914728849520E-13 ) ) ;
#30661 = ORIENTED_EDGE ( 'NONE', *, *, #8570, .F. ) ;
#30662 = DIRECTION ( 'NONE',  ( -1.000000000000000000, -3.053848253006669023E-16, 2.042510438544995415E-16 ) ) ;
#30663 = TOROIDAL_SURFACE ( 'NONE', #18499, 3.648039984012787063, 0.05000000000000000278 ) ;
#30664 = PLANE ( 'NONE',  #13852 ) ;
#30665 = TOROIDAL_SURFACE ( 'NONE', #15582, 4.000000000000022204, 0.1000000000000000056 ) ;
#30666 = ADVANCED_FACE ( 'NONE', ( #15933, #1071 ), #8654, .T. ) ;
#30667 = CARTESIAN_POINT ( 'NONE',  ( -54.47754877553799702, -1.508273929415538062, -3.305418158118663463 ) ) ;
#30668 = AXIS2_PLACEMENT_3D ( 'NONE', #22980, #13446, #13001 ) ;
#30669 = DIRECTION ( 'NONE',  ( -4.670714851210922627E-16, -0.9333474217026305197, -0.3589743589743593088 ) ) ;
#30670 = CARTESIAN_POINT ( 'NONE',  ( -59.44702994616203995, 4.156921938165313080, -1.958927657850919798E-13 ) ) ;
#30671 = ADVANCED_FACE ( 'NONE', ( #1531 ), #27830, .T. ) ;
#30672 = VECTOR ( 'NONE', #11360, 1000.000000000000000 ) ;
#30673 = CARTESIAN_POINT ( 'NONE',  ( -62.29999999999998295, 2.799131621120617641, 0.06972924524667370449 ) ) ;
#30674 = VECTOR ( 'NONE', #14815, 1000.000000000000000 ) ;
#30675 = CIRCLE ( 'NONE', #17049, 0.1000000000000001721 ) ;
#30677 = AXIS2_PLACEMENT_3D ( 'NONE', #28897, #23842, #2459 ) ;
#30676 = CARTESIAN_POINT ( 'NONE',  ( 15.03925126672132961, 3.426725943139509845, 3.937891353488782276 ) ) ;
#30678 = DIRECTION ( 'NONE',  ( -1.000000000000000000, -3.053848253006669023E-16, 2.042510438544995415E-16 ) ) ;
#30679 = CARTESIAN_POINT ( 'NONE',  ( -57.17292740578359656, 1.073804522883514023, 3.225979517392339346 ) ) ;
#30680 = EDGE_CURVE ( 'NONE', #26503, #16594, #16604, .T. ) ;
#30681 = CARTESIAN_POINT ( 'NONE',  ( -64.31974649313019654, -2.248654970328749947, -0.05601630617084708830 ) ) ;
#30682 = EDGE_LOOP ( 'NONE', ( #25596, #28438, #15883, #6798 ) ) ;
#30683 = AXIS2_PLACEMENT_3D ( 'NONE', #5082, #8083, #12659 ) ;
#30684 = CARTESIAN_POINT ( 'NONE',  ( 47.00000000000002132, 2.478823385132571406E-14, 4.100000000000022737 ) ) ;
#30685 = CARTESIAN_POINT ( 'NONE',  ( 51.24551381660811700, 1.093420264359095784, 1.202138525661322843 ) ) ;
#30686 = CIRCLE ( 'NONE', #3394, 2.000000000000000000 ) ;
#30687 = CARTESIAN_POINT ( 'NONE',  ( -36.11187263677869197, -0.3981319440505055596, 5.199999999410220397 ) ) ;
#30688 = DIRECTION ( 'NONE',  ( 1.000000000000000000, 1.047444401652940007E-14, 0.000000000000000000 ) ) ;
#30689 = ORIENTED_EDGE ( 'NONE', *, *, #15153, .F. ) ;
#30690 = LINE ( 'NONE', #6015, #23429 ) ;
#30691 = AXIS2_PLACEMENT_3D ( 'NONE', #20849, #16847, #15917 ) ;
#30692 = ORIENTED_EDGE ( 'NONE', *, *, #7359, .F. ) ;
#30693 = CARTESIAN_POINT ( 'NONE',  ( 22.07280086217093640, 8.086143481909154218, -1.425000000000076650 ) ) ;
#30695 = DIRECTION ( 'NONE',  ( -0.9993908270190953180, 0.03489949670251430575, 3.490905158897711881E-15 ) ) ;
#30694 = CARTESIAN_POINT ( 'NONE',  ( 48.46709009337374141, 1.365599538210783281, 3.854893000251051749 ) ) ;
#30696 = ADVANCED_FACE ( 'NONE', ( #11191 ), #30493, .T. ) ;
#30697 = VERTEX_POINT ( 'NONE', #18488 ) ;
#30698 = ORIENTED_EDGE ( 'NONE', *, *, #9940, .T. ) ;
#30699 = CARTESIAN_POINT ( 'NONE',  ( 50.40000000000001990, -1.409787217987148233, 3.950000000000022826 ) ) ;
#30700 = CLOSED_SHELL ( 'NONE', ( #31104, #9962, #15328, #17524, #8467, #6327, #9305, #10362, #26400, #18998, #866, #10053, #30696, #13331, #8969, #22611, #9463, #27180, #14786, #7281, #15402, #20357, #30213, #21839, #1217, #15640, #13212, #8701, #5387, #4220, #7739, #4783, #5454, #13136, #5114, #3783, #27666, #20108, #15662, #3979, #12720, #21834, #8282, #17269, #9640, #21643, #29551, #27167, #11902, #25734, #24059, #10556, #30418, #6883, #26691, #1473, #1702, #15053, #6008, #5151, #7554, #3775, #23815, #20060, #20677, #6185, #16817, #1234, #18620 ) ) ;
#30701 = CIRCLE ( 'NONE', #28189, 0.1500000000000001887 ) ;
#30702 = CARTESIAN_POINT ( 'NONE',  ( 50.59602332238209499, -0.1408342061598471806, -0.8215393206232035617 ) ) ;
#30704 = CARTESIAN_POINT ( 'NONE',  ( 58.65838214097809100, 0.9664062014978274107, 1.606847897768749700 ) ) ;
#30703 = CARTESIAN_POINT ( 'NONE',  ( -59.92928932188130631, 2.138123341857387114E-15, 5.538933845919563674E-16 ) ) ;
#30705 = AXIS2_PLACEMENT_3D ( 'NONE', #4474, #21430, #7316 ) ;
#30706 = EDGE_LOOP ( 'NONE', ( #8292, #20922, #11483, #2775 ) ) ;
#30707 = CARTESIAN_POINT ( 'NONE',  ( -55.56249999999997158, -3.238593381231840151, -2.874284765127021579 ) ) ;
#30708 = CARTESIAN_POINT ( 'NONE',  ( -36.92398358572908990, 2.945786441214503171, 4.543674732827777341 ) ) ;
#30709 = ITEM_DEFINED_TRANSFORMATION ( 'NONE', 'NONE', #14121,  #9018 ) ;
#30710 = ADVANCED_FACE ( 'NONE', ( #30347 ), #28129, .F. ) ;
#30711 = DIRECTION ( 'NONE',  ( 0.000000000000000000, 1.000000000000000000, 1.224646799147353207E-16 ) ) ;
#30712 = CARTESIAN_POINT ( 'NONE',  ( -54.39999999999997726, 8.366749974758487600E-15, -2.213041600731273397E-13 ) ) ;
#30713 = EDGE_CURVE ( 'NONE', #236, #26849, #4947, .T. ) ;
#30714 = CARTESIAN_POINT ( 'NONE',  ( -62.09999999999998010, -2.742892450101797053, 0.2063307189744075232 ) ) ;
#30715 = CIRCLE ( 'NONE', #20628, 160.5997717543497743 ) ;
#30716 = EDGE_CURVE ( 'NONE', #30654, #20368, #25761, .T. ) ;
#30717 = ORIENTED_EDGE ( 'NONE', *, *, #5661, .T. ) ;
#30718 = AXIS2_PLACEMENT_3D ( 'NONE', #13892, #1412, #11072 ) ;
#30719 = CARTESIAN_POINT ( 'NONE',  ( 57.04767748491563140, -0.7500000000000049960, 1.778341924377874639 ) ) ;
#30720 = CIRCLE ( 'NONE', #5931, 0.04999999999999991257 ) ;
#30721 = CARTESIAN_POINT ( 'NONE',  ( -35.98952425903317476, 2.686240675664352207, -4.475885398016837158 ) ) ;
#30722 = CARTESIAN_POINT ( 'NONE',  ( 51.21021026411726496, 1.041641720705850149, -1.248302399389048079 ) ) ;
#30723 = DIRECTION ( 'NONE',  ( 0.000000000000000000, 0.000000000000000000, -1.000000000000000000 ) ) ;
#30724 = CARTESIAN_POINT ( 'NONE',  ( 15.59140265158955962, 0.9780988077348221621, -5.318542208600380405 ) ) ;
#30725 = TOROIDAL_SURFACE ( 'NONE', #28726, 159.7997717543496776, 0.1000000000000000056 ) ;
#30726 = VECTOR ( 'NONE', #21333, 1000.000000000000000 ) ;
#30728 = DIRECTION ( 'NONE',  ( 0.000000000000000000, 1.000000000000000000, 0.000000000000000000 ) ) ;
#30727 = CARTESIAN_POINT ( 'NONE',  ( -56.18749999999997868, 0.7533615035078126132, -3.673546848079176641 ) ) ;
#30729 = CARTESIAN_POINT ( 'NONE',  ( 51.80000000000001137, -4.031600731908413948, -1.173113608511855421 ) ) ;
#30731 = DIRECTION ( 'NONE',  ( 0.000000000000000000, 1.000000000000000000, -1.224646799147353207E-16 ) ) ;
#30730 = DIRECTION ( 'NONE',  ( 3.002035892788116966E-16, -0.9996898646859343485, -0.02490330187381123786 ) ) ;
#30732 = ORIENTED_EDGE ( 'NONE', *, *, #28181, .T. ) ;
#30733 = PLANE ( 'NONE',  #15094 ) ;
#30734 = AXIS2_PLACEMENT_3D ( 'NONE', #4471, #7015, #14124 ) ;
#30736 = CARTESIAN_POINT ( 'NONE',  ( -36.11122220296842045, 5.068511731019554212, 1.228278365481957790 ) ) ;
#30735 = CARTESIAN_POINT ( 'NONE',  ( -59.19999999999996732, 2.569786949633446671, -0.9498634748674490424 ) ) ;
#30737 = CARTESIAN_POINT ( 'NONE',  ( 61.25000000000001421, 1.000000000000641709, -1.863080903343375061 ) ) ;
#30738 = EDGE_CURVE ( 'NONE', #28523, #171, #24679, .T. ) ;
#30739 = ORIENTED_EDGE ( 'NONE', *, *, #29928, .T. ) ;
#30740 = ORIENTED_EDGE ( 'NONE', *, *, #11447, .T. ) ;
#30741 = CARTESIAN_POINT ( 'NONE',  ( -36.31440869660541892, -4.962395293451386635, 1.554871187131941834 ) ) ;
#30742 = CARTESIAN_POINT ( 'NONE',  ( 50.31550977796904789, -1.386241252175274496, 3.851058308531627894 ) ) ;
#30743 = AXIS2_PLACEMENT_3D ( 'NONE', #9461, #9145, #24013 ) ;
#30744 = AXIS2_PLACEMENT_3D ( 'NONE', #18820, #26081, #31146 ) ;
#30745 = ORIENTED_EDGE ( 'NONE', *, *, #6499, .T. ) ;
#30746 = ADVANCED_FACE ( 'NONE', ( #3602 ), #23083, .F. ) ;
#30747 = DIRECTION ( 'NONE',  ( 0.000000000000000000, 0.000000000000000000, -1.000000000000000000 ) ) ;
#30748 = EDGE_LOOP ( 'NONE', ( #3235, #26757, #6413, #10677 ) ) ;
#30749 = CARTESIAN_POINT ( 'NONE',  ( 58.74160516400051790, 1.872695119589735668, -0.09319124196165359808 ) ) ;
#30750 = ORIENTED_EDGE ( 'NONE', *, *, #83, .T. ) ;
#30751 = CARTESIAN_POINT ( 'NONE',  ( -55.69702994616204705, 4.156921938165313968, -1.817815585352543609E-13 ) ) ;
#30752 = CARTESIAN_POINT ( 'NONE',  ( -58.83155989232410832, -1.962990915244706924, -3.400000000000215294 ) ) ;
#30753 = VERTEX_POINT ( 'NONE', #1676 ) ;
#30754 = ORIENTED_EDGE ( 'NONE', *, *, #9670, .F. ) ;
#30755 = ORIENTED_EDGE ( 'NONE', *, *, #3383, .F. ) ;
#30756 = CARTESIAN_POINT ( 'NONE',  ( -59.68749999999995737, 1.962990915244749557, -3.400000000000203304 ) ) ;
#30757 = CARTESIAN_POINT ( 'NONE',  ( -62.09999999999997300, -2.520404473256288469, 0.1522704540930145123 ) ) ;
#30758 = DIRECTION ( 'NONE',  ( 0.000000000000000000, 0.000000000000000000, 1.000000000000000000 ) ) ;
#30759 = CARTESIAN_POINT ( 'NONE',  ( 51.36308620441100459, -1.097739233405183201, -1.198394850649635801 ) ) ;
#30760 = CARTESIAN_POINT ( 'NONE',  ( -61.10430241999912937, -2.555382569520581626, -0.8803594241308302371 ) ) ;
#30761 = CARTESIAN_POINT ( 'NONE',  ( -57.72099364905386665, -0.2309624077928972563, -3.875409454552788624 ) ) ;
#30762 =( BOUNDED_CURVE ( )  B_SPLINE_CURVE ( 3, ( #3954, #23286, #29347, #7658 ),
 .UNSPECIFIED., .F., .T. ) 
 B_SPLINE_CURVE_WITH_KNOTS ( ( 4, 4 ),
 ( 1.169545686397452711, 1.279118582711132435 ),
 .UNSPECIFIED. ) 
 CURVE ( )  GEOMETRIC_REPRESENTATION_ITEM ( )  RATIONAL_B_SPLINE_CURVE ( ( 1.000000000000000000, 0.9989997319336324511, 0.9989997319336324511, 1.000000000000000000 ) ) 
 REPRESENTATION_ITEM ( '' )  );
#30763 = SURFACE_SIDE_STYLE ('',( #28389 ) ) ;
#30764 = DIRECTION ( 'NONE',  ( 1.000000000000000000, -0.000000000000000000, -0.000000000000000000 ) ) ;
#30765 = CARTESIAN_POINT ( 'NONE',  ( 15.45522337368516297, 5.005099703116323795, -1.423440526321878563 ) ) ;
#30766 = CARTESIAN_POINT ( 'NONE',  ( 57.03828022491683924, 0.8151581666669124315, 2.468910358759941914 ) ) ;
#30767 = FACE_OUTER_BOUND ( 'NONE', #13937, .T. ) ;
#30768 = APPLICATION_CONTEXT ( 'automotive_design' ) ;
#30769 = CARTESIAN_POINT ( 'NONE',  ( 50.40000000000003411, 0.7619326981554777056, -3.939508824314740032 ) ) ;
#30770 = ORIENTED_EDGE ( 'NONE', *, *, #12811, .T. ) ;
#30772 = CARTESIAN_POINT ( 'NONE',  ( 50.32795105345940812, -1.409900792624644739, 3.850000304694922271 ) ) ;
#30771 = CARTESIAN_POINT ( 'NONE',  ( 51.02976068049119363, -1.019450805964126516, -1.268081568884226407 ) ) ;
#30773 = ADVANCED_FACE ( 'NONE', ( #21020 ), #3743, .T. ) ;
#30774 = LINE ( 'NONE', #9083, #2855 ) ;
#30775 = EDGE_CURVE ( 'NONE', #5953, #5818, #22670, .T. ) ;
#30776 = ORIENTED_EDGE ( 'NONE', *, *, #7473, .F. ) ;
#30777 = ADVANCED_FACE ( 'NONE', ( #13239 ), #8408, .T. ) ;
#30778 = DIRECTION ( 'NONE',  ( -0.000000000000000000, -1.000000000000000000, 0.000000000000000000 ) ) ;
#30779 = CARTESIAN_POINT ( 'NONE',  ( -59.43749999999997868, 1.962990915244722689, 3.399999999999796962 ) ) ;
#30780 = ORIENTED_EDGE ( 'NONE', *, *, #15008, .T. ) ;
#30781 = ORIENTED_EDGE ( 'NONE', *, *, #10687, .T. ) ;
#30782 = LINE ( 'NONE', #16539, #16968 ) ;
#30783 = VERTEX_POINT ( 'NONE', #31132 ) ;
#30784 = CARTESIAN_POINT ( 'NONE',  ( 51.36283714269074352, 1.001673184508090397, -1.284520656909115877 ) ) ;
#30785 = VECTOR ( 'NONE', #7996, 1000.000000000000000 ) ;
#30786 = CARTESIAN_POINT ( 'NONE',  ( 50.35762544161294585, 8.151359338959888845, -2.050000000000174794 ) ) ;
#30787 = ORIENTED_EDGE ( 'NONE', *, *, #19982, .F. ) ;
#30788 = CARTESIAN_POINT ( 'NONE',  ( 47.10000000000002274, -4.276948333784438283, -0.9210526315789475671 ) ) ;
#30789 = DIRECTION ( 'NONE',  ( 1.000000000000000000, 1.047444401652940007E-14, 0.000000000000000000 ) ) ;
#30790 = DIRECTION ( 'NONE',  ( -1.000000000000000000, -3.053848253006669023E-16, 2.042510438544995415E-16 ) ) ;
#30791 = ORIENTED_EDGE ( 'NONE', *, *, #13867, .F. ) ;
#30792 = ORIENTED_EDGE ( 'NONE', *, *, #17751, .F. ) ;
#30793 = EDGE_CURVE ( 'NONE', #10647, #30371, #13036, .T. ) ;
#30794 = DIRECTION ( 'NONE',  ( 0.000000000000000000, 0.9996898646859344595, 0.02490330187381124480 ) ) ;
#30795 = CARTESIAN_POINT ( 'NONE',  ( 52.20711756518982583, 0.7500000000005468959, 1.718465885608440491 ) ) ;
#30796 = CARTESIAN_POINT ( 'NONE',  ( -54.99986116251336199, 1.737685414808520790, -3.471684241605567323 ) ) ;
#30797 = VERTEX_POINT ( 'NONE', #4541 ) ;
#30798 = DIRECTION ( 'NONE',  ( 0.000000000000000000, -0.9996898646859343485, -0.02490330187381123786 ) ) ;
#30799 = CARTESIAN_POINT ( 'NONE',  ( 16.00221665700883023, 3.629052419422171827, 4.014440194077253388 ) ) ;
#30800 = DIRECTION ( 'NONE',  ( 2.614381936396368743E-16, -0.2008964009354147762, 0.9796124928211139560 ) ) ;
#30801 = FACE_OUTER_BOUND ( 'NONE', #3323, .T. ) ;
#30803 = CARTESIAN_POINT ( 'NONE',  ( 58.75000000694009117, -0.9860766835994869695, 1.658042653848745607 ) ) ;
#30802 = DIRECTION ( 'NONE',  ( 0.000000000000000000, -1.000000000000000000, 0.000000000000000000 ) ) ;
#30804 = AXIS2_PLACEMENT_3D ( 'NONE', #24543, #17595, #10459 ) ;
#30805 = FACE_OUTER_BOUND ( 'NONE', #1115, .T. ) ;
#30806 = LINE ( 'NONE', #26214, #22655 ) ;
#30807 = TOROIDAL_SURFACE ( 'NONE', #8069, 1.975000000000001865, 0.1000000000000000056 ) ;
#30808 = CARTESIAN_POINT ( 'NONE',  ( 52.06628335902944826, 0.5434431642986571331, -1.794517909405660694 ) ) ;
#30809 = DIRECTION ( 'NONE',  ( 0.000000000000000000, 1.000000000000000000, -1.224646799147353207E-16 ) ) ;
#30810 = ORIENTED_EDGE ( 'NONE', *, *, #22402, .T. ) ;
#30811 = ORIENTED_EDGE ( 'NONE', *, *, #2225, .T. ) ;
#30812 = EDGE_CURVE ( 'NONE', #18266, #18396, #31248, .T. ) ;
#30813 = LINE ( 'NONE', #14013, #29501 ) ;
#30814 = ORIENTED_EDGE ( 'NONE', *, *, #12781, .T. ) ;
#30815 = EDGE_CURVE ( 'NONE', #26954, #22739, #16492, .T. ) ;
#30816 = CARTESIAN_POINT ( 'NONE',  ( 53.16217804548205805, 8.131925109091699966, 2.049999999999814637 ) ) ;
#30817 = CARTESIAN_POINT ( 'NONE',  ( -55.72085481156724285, 2.489203624310592833, -2.804704140674919799 ) ) ;
#30819 = DIRECTION ( 'NONE',  ( 2.117927888850091331E-16, -0.02490330187381135929, 0.9996898646859343485 ) ) ;
#30818 = DIRECTION ( 'NONE',  ( 1.000000000000000000, 1.047444401652940007E-14, 0.000000000000000000 ) ) ;
#30820 = VERTEX_POINT ( 'NONE', #11672 ) ;
#30821 = DIRECTION ( 'NONE',  ( -1.000000000000000000, -3.053848253006669023E-16, 2.042510438544995415E-16 ) ) ;
#30822 = EDGE_LOOP ( 'NONE', ( #10175, #17005, #27732, #4767 ) ) ;
#30823 = FACE_OUTER_BOUND ( 'NONE', #10686, .T. ) ;
#30824 = VECTOR ( 'NONE', #2039, 1000.000000000000000 ) ;
#30825 = ORIENTED_EDGE ( 'NONE', *, *, #20997, .T. ) ;
#30827 = CARTESIAN_POINT ( 'NONE',  ( 50.83686442967773900, 8.734989671305513070, 2.049999999999822631 ) ) ;
#30826 = CARTESIAN_POINT ( 'NONE',  ( 50.40000000000001279, 0.6304760106459513791, 3.950000000000022826 ) ) ;
#30828 = EDGE_LOOP ( 'NONE', ( #27929, #5770, #29475, #24012, #25315, #13710 ) ) ;
#30829 = CARTESIAN_POINT ( 'NONE',  ( 53.06647667635083820, 8.205144683163286601, 1.913422281012191029 ) ) ;
#30830 = CYLINDRICAL_SURFACE ( 'NONE', #27511, 5.407411300779133789 ) ;
#30831 = AXIS2_PLACEMENT_3D ( 'NONE', #2974, #19920, #21849 ) ;
#30832 = EDGE_CURVE ( 'NONE', #26017, #7227, #29741, .T. ) ;
#30833 = CARTESIAN_POINT ( 'NONE',  ( -54.47366401599046526, -1.505709097230404359, -3.303769268891089350 ) ) ;
#30834 = AXIS2_PLACEMENT_3D ( 'NONE', #19514, #5095, #24405 ) ;
#30835 = CARTESIAN_POINT ( 'NONE',  ( 57.00000000000001421, 0.7256347085964565125, 1.800308733460772359 ) ) ;
#30836 = CARTESIAN_POINT ( 'NONE',  ( -59.88452994616203995, -3.117691453623976816, 1.799999999999775335 ) ) ;
#30837 = CARTESIAN_POINT ( 'NONE',  ( 51.87908472284573946, 0.03364117306051616491, 4.372691834281944523 ) ) ;
#30838 = VECTOR ( 'NONE', #24291, 999.9999999999998863 ) ;
#30839 = B_SPLINE_CURVE_WITH_KNOTS ( 'NONE', 3,
 ( #15554, #10322, #27422, #15382, #27567, #19991, #8569, #5896, #18099 ),
 .UNSPECIFIED., .F., .F.,
 ( 4, 1, 1, 1, 1, 1, 4 ),
 ( 0.000000000000000000, 0.08990530927501938496, 0.2069505209790863942, 0.2957249676700259844, 0.5865340158044511920, 0.7553074047937105018, 0.9685669348269276835 ),
 .UNSPECIFIED. ) ;
#30840 = DIRECTION ( 'NONE',  ( 0.000000000000000000, 0.000000000000000000, 1.000000000000000000 ) ) ;
#30841 = CARTESIAN_POINT ( 'NONE',  ( -62.14999999999998437, -2.799131621120614977, -0.06972924524666890278 ) ) ;
#30842 = CARTESIAN_POINT ( 'NONE',  ( -56.17292740578360366, -3.330682475591780989, -0.6830477631804185989 ) ) ;
#30843 = LINE ( 'NONE', #9160, #3830 ) ;
#30844 = ORIENTED_EDGE ( 'NONE', *, *, #11831, .T. ) ;
#30845 = DIRECTION ( 'NONE',  ( -9.654113257610060303E-15, 0.000000000000000000, -1.000000000000000000 ) ) ;
#30846 = CARTESIAN_POINT ( 'NONE',  ( 60.88048385701372212, -0.6732112958808652570, -1.479676701994273369 ) ) ;
#30847 = CARTESIAN_POINT ( 'NONE',  ( -36.48174642952978530, 0.4008586329627822908, 5.396496690166785903 ) ) ;
#30848 = CARTESIAN_POINT ( 'NONE',  ( 50.59602332238209499, -0.1408342061598474304, -0.7375000000000029310 ) ) ;
#30849 = ORIENTED_EDGE ( 'NONE', *, *, #412, .T. ) ;
#30850 = EDGE_CURVE ( 'NONE', #29022, #27662, #6754, .T. ) ;
#30851 = CARTESIAN_POINT ( 'NONE',  ( 58.74160516400055343, 1.668397168087972116, 0.8556415768457033000 ) ) ;
#30852 = VERTEX_POINT ( 'NONE', #23544 ) ;
#30853 = DIRECTION ( 'NONE',  ( 3.489354422748178582E-15, -1.218509414717996338E-16, 1.000000000000000000 ) ) ;
#30854 = VECTOR ( 'NONE', #4337, 1000.000000000000000 ) ;
#30856 = DIRECTION ( 'NONE',  ( 1.000000000000000000, 1.047444401652940007E-14, 0.000000000000000000 ) ) ;
#30855 = DIRECTION ( 'NONE',  ( -0.000000000000000000, -0.2573099415204678775, -0.9663289263986325484 ) ) ;
#30857 = ORIENTED_EDGE ( 'NONE', *, *, #29803, .T. ) ;
#30858 = VERTEX_POINT ( 'NONE', #31296 ) ;
#30859 = CARTESIAN_POINT ( 'NONE',  ( 56.95000000000001705, 0.7137254901960785602, 2.500119182087999548 ) ) ;
#30860 = CIRCLE ( 'NONE', #4048, 1.000000000000000444 ) ;
#30861 = DIRECTION ( 'NONE',  ( 0.9993908270190958731, -0.03489949670250092062, -3.492262959426260213E-15 ) ) ;
#30863 = CARTESIAN_POINT ( 'NONE',  ( 58.65266784251151932, 0.8793208749734084950, 1.656109637136073731 ) ) ;
#30862 = CARTESIAN_POINT ( 'NONE',  ( -35.85663232820584767, -3.817150320979536104, -2.203324261493425862 ) ) ;
#30864 = ORIENTED_EDGE ( 'NONE', *, *, #8115, .F. ) ;
#30865 = CARTESIAN_POINT ( 'NONE',  ( -55.31249999999998579, 4.108500314926513575, -1.367561758111407899 ) ) ;
#30866 = CARTESIAN_POINT ( 'NONE',  ( 63.50000000000002842, 1.401298464324817071E-42, -6.651271950496169736E-13 ) ) ;
#30867 = CARTESIAN_POINT ( 'NONE',  ( 67.99999999999998579, 4.286263797015756316E-16, -3.500000000000712763 ) ) ;
#30868 = CARTESIAN_POINT ( 'NONE',  ( 69.01464466094073202, 4.557543281186736018E-17, 2.985355339058589852 ) ) ;
#30869 = DIRECTION ( 'NONE',  ( 0.000000000000000000, 0.000000000000000000, 1.000000000000000000 ) ) ;
#30870 = CARTESIAN_POINT ( 'NONE',  ( -62.09999999999998010, -2.636465585633694264, 0.1493792525119599646 ) ) ;
#30871 = ORIENTED_EDGE ( 'NONE', *, *, #17004, .T. ) ;
#30872 = B_SPLINE_CURVE_WITH_KNOTS ( 'NONE', 3,
 ( #24352, #22151, #29549, #588, #3279, #5329, #742, #10101, #2665, #15310 ),
 .UNSPECIFIED., .F., .F.,
 ( 4, 2, 2, 2, 4 ),
 ( 0.000000000000000000, 0.0003600849014046860722, 0.0007201698028093721443, 0.001080254704214058271, 0.001440339605618744289 ),
 .UNSPECIFIED. ) ;
#30873 = DIRECTION ( 'NONE',  ( 0.000000000000000000, 0.000000000000000000, 1.000000000000000000 ) ) ;
#30874 = CARTESIAN_POINT ( 'NONE',  ( -36.50489844130355976, 2.884962146574165054, -4.577321775072915599 ) ) ;
#30875 = CARTESIAN_POINT ( 'NONE',  ( 48.42277498379875311, 1.384253668070434484, -3.859284659399053741 ) ) ;
#30876 = B_SPLINE_CURVE_WITH_KNOTS ( 'NONE', 3,
 ( #9180, #9329, #6789, #16777, #26106, #28647 ),
 .UNSPECIFIED., .F., .F.,
 ( 4, 2, 4 ),
 ( 0.000000000000000000, 0.0001000270069598443860, 0.0002000540139196887719 ),
 .UNSPECIFIED. ) ;
#30877 = DIRECTION ( 'NONE',  ( 0.000000000000000000, 0.000000000000000000, 1.000000000000000000 ) ) ;
#30878 = EDGE_CURVE ( 'NONE', #16179, #5897, #2941, .T. ) ;
#30879 = CIRCLE ( 'NONE', #15210, 1.000000000000000000 ) ;
#30880 = DIRECTION ( 'NONE',  ( 0.000000000000000000, 0.9996898646859344595, 0.02490330187381124827 ) ) ;
#30882 = DIRECTION ( 'NONE',  ( 3.489354422748178582E-15, -1.218509414717996338E-16, 1.000000000000000000 ) ) ;
#30881 = CARTESIAN_POINT ( 'NONE',  ( -54.39999999999997726, 8.366749974758389781E-15, -1.935485844574984262E-13 ) ) ;
#30883 = CARTESIAN_POINT ( 'NONE',  ( 47.86788581435126844, -4.319730106544175108, -1.256953381563268524 ) ) ;
#30885 = DIRECTION ( 'NONE',  ( -1.000000000000000000, 0.000000000000000000, 1.047444401652940007E-14 ) ) ;
#30884 = DIRECTION ( 'NONE',  ( 5.182136041040955759E-15, -3.491481338843133355E-15, 1.000000000000000000 ) ) ;
#30886 = VERTEX_POINT ( 'NONE', #26850 ) ;
#30887 = ADVANCED_FACE ( 'NONE', ( #2636 ), #11660, .T. ) ;
#30888 = SHAPE_REPRESENTATION ( 'Eraser', ( #9018 ), #18167 ) ;
#30889 = CARTESIAN_POINT ( 'NONE',  ( -62.05200726403181477, -2.672099260701759516, -0.3872133491583026887 ) ) ;
#30890 = ADVANCED_FACE ( 'NONE', ( #29996 ), #8926, .T. ) ;
#30891 = DIRECTION ( 'NONE',  ( -1.000000000000000000, -3.054025858079668409E-16, 2.042474015755241579E-16 ) ) ;
#30893 = CARTESIAN_POINT ( 'NONE',  ( -35.85663232820592583, 4.804073783693418420, 2.042134687550397398 ) ) ;
#30892 = CARTESIAN_POINT ( 'NONE',  ( 15.29954477411457070, -2.199885872770988904, -4.939696258129290030 ) ) ;
#30895 = ADVANCED_FACE ( 'NONE', ( #17977 ), #4029, .T. ) ;
#30894 = CARTESIAN_POINT ( 'NONE',  ( 15.67083574136753121, -5.009497273852900889, 2.047744636826879461 ) ) ;
#30896 = VERTEX_POINT ( 'NONE', #13209 ) ;
#30897 = ORIENTED_EDGE ( 'NONE', *, *, #21399, .T. ) ;
#30898 = CARTESIAN_POINT ( 'NONE',  ( -36.26369610968610857, -5.012449653004694028, 1.400819699606154822 ) ) ;
#30899 = CARTESIAN_POINT ( 'NONE',  ( 50.30837315852409830, -1.391941090707504047, 3.850000000000021849 ) ) ;
#30900 = VERTEX_POINT ( 'NONE', #23207 ) ;
#30901 = DIRECTION ( 'NONE',  ( 0.000000000000000000, 0.9996898646859343485, 0.02490330187381123786 ) ) ;
#30902 = AXIS2_PLACEMENT_3D ( 'NONE', #26882, #13651, #30923 ) ;
#30903 = ORIENTED_EDGE ( 'NONE', *, *, #24377, .T. ) ;
#30904 = CARTESIAN_POINT ( 'NONE',  ( 58.75000000000000000, 1.964000600391587081, -0.09700564724573840225 ) ) ;
#30905 = VERTEX_POINT ( 'NONE', #27626 ) ;
#30906 = EDGE_CURVE ( 'NONE', #779, #6477, #17617, .T. ) ;
#30907 = DIRECTION ( 'NONE',  ( -1.000000000000000000, -0.000000000000000000, 3.491481338843133750E-15 ) ) ;
#30908 = ORIENTED_EDGE ( 'NONE', *, *, #27445, .T. ) ;
#30909 = ORIENTED_EDGE ( 'NONE', *, *, #13665, .T. ) ;
#30910 = ORIENTED_EDGE ( 'NONE', *, *, #1489, .T. ) ;
#30911 = CARTESIAN_POINT ( 'NONE',  ( -59.37499999999997868, -3.920666489018300969E-15, 3.399999999999788525 ) ) ;
#30912 = DIRECTION ( 'NONE',  ( 1.000000000000000000, -1.219044193948983948E-29, 3.491481338843133355E-15 ) ) ;
#30913 = CARTESIAN_POINT ( 'NONE',  ( 23.49584529083620765, 5.910990189302484765, -1.425000000000082201 ) ) ;
#30914 = CARTESIAN_POINT ( 'NONE',  ( 51.23644008536124517, -1.080112125195908490, -1.214076932077872817 ) ) ;
#30915 = EDGE_CURVE ( 'NONE', #17824, #15088, #24783, .T. ) ;
#30916 =( GEOMETRIC_REPRESENTATION_CONTEXT ( 3 ) GLOBAL_UNCERTAINTY_ASSIGNED_CONTEXT ( ( #7606 ) ) GLOBAL_UNIT_ASSIGNED_CONTEXT ( ( #4410, #23890, #28638 ) ) REPRESENTATION_CONTEXT ( 'NONE', 'WORKASPACE' ) );
#30917 = CARTESIAN_POINT ( 'NONE',  ( 64.25000000000001421, 1.990051048615613918E-16, -1.625000000000225819 ) ) ;
#30918 = CIRCLE ( 'NONE', #23351, 0.4500000000000001221 ) ;
#30919 = EDGE_CURVE ( 'NONE', #2594, #21812, #11029, .T. ) ;
#30920 = CARTESIAN_POINT ( 'NONE',  ( -57.74999999999997158, -1.184343223768574260, -3.558065644182727638 ) ) ;
#30921 = FACE_OUTER_BOUND ( 'NONE', #20586, .T. ) ;
#30922 = CARTESIAN_POINT ( 'NONE',  ( -36.79682133506354802, -3.614202567155977874, -4.024415706308069218 ) ) ;
#30923 = DIRECTION ( 'NONE',  ( 0.000000000000000000, 0.000000000000000000, -1.000000000000000000 ) ) ;
#30924 = CARTESIAN_POINT ( 'NONE',  ( 50.59602332238209499, -0.1408342061598474859, 1.212874140286674285 ) ) ;
#30925 = EDGE_CURVE ( 'NONE', #12162, #7685, #23182, .T. ) ;
#30926 = CARTESIAN_POINT ( 'NONE',  ( 53.25905939444253789, 8.220207195185320614, 2.049999999999814637 ) ) ;
#30927 = VERTEX_POINT ( 'NONE', #4503 ) ;
#30929 = DIRECTION ( 'NONE',  ( 0.000000000000000000, 0.000000000000000000, 1.000000000000000000 ) ) ;
#30928 = DIRECTION ( 'NONE',  ( -1.000000000000000000, -1.018631342913014973E-14, -0.000000000000000000 ) ) ;
#30930 = EDGE_CURVE ( 'NONE', #9415, #6633, #11532, .T. ) ;
#30931 = CARTESIAN_POINT ( 'NONE',  ( 61.25000000000001421, 1.000000000000641709, 1.655766640118845112 ) ) ;
#30932 = AXIS2_PLACEMENT_3D ( 'NONE', #13949, #4150, #1942 ) ;
#30933 = ORIENTED_EDGE ( 'NONE', *, *, #28459, .F. ) ;
#30934 = CARTESIAN_POINT ( 'NONE',  ( 47.00000000000002842, -4.179189514726506793, -1.000000000000000000 ) ) ;
#30935 = DIRECTION ( 'NONE',  ( 0.000000000000000000, 0.000000000000000000, 1.000000000000000000 ) ) ;
#30936 = CARTESIAN_POINT ( 'NONE',  ( -60.87499999999997158, -3.920666489018282036E-15, 3.399999999999783196 ) ) ;
#30937 = VERTEX_POINT ( 'NONE', #19085 ) ;
#30938 = ORIENTED_EDGE ( 'NONE', *, *, #2261, .T. ) ;
#30939 = CARTESIAN_POINT ( 'NONE',  ( 15.49702763512083337, 4.962395293451323575, 1.554871187131933841 ) ) ;
#30940 = EDGE_LOOP ( 'NONE', ( #7076, #9914, #22109, #10129 ) ) ;
#30941 = CARTESIAN_POINT ( 'NONE',  ( 58.75000000000003553, -1.671477153793476722, 0.8495817349404574115 ) ) ;
#30942 = AXIS2_PLACEMENT_3D ( 'NONE', #17213, #24636, #5162 ) ;
#30943 = CARTESIAN_POINT ( 'NONE',  ( 51.80000000000001137, -4.003661535119149129, -1.169131321892099340 ) ) ;
#30944 = VERTEX_POINT ( 'NONE', #6715 ) ;
#30945 = CARTESIAN_POINT ( 'NONE',  ( 63.50000000000002842, 1.401298464324817071E-42, -6.651271950496169736E-13 ) ) ;
#30946 = PLANE ( 'NONE',  #23292 ) ;
#30947 = CARTESIAN_POINT ( 'NONE',  ( -73.89999999999997726, -2.435524336289708093E-15, 4.607889071584891164E-15 ) ) ;
#30948 = ORIENTED_EDGE ( 'NONE', *, *, #21596, .F. ) ;
#30949 = ORIENTED_EDGE ( 'NONE', *, *, #14425, .F. ) ;
#30950 = CARTESIAN_POINT ( 'NONE',  ( -58.77900635094606940, -1.737685414808524564, 3.471684241605558885 ) ) ;
#30951 = CARTESIAN_POINT ( 'NONE',  ( -55.62499999999998579, -4.753426312438546834E-15, 3.399999999999801403 ) ) ;
#30952 = DIRECTION ( 'NONE',  ( 0.000000000000000000, 0.8381322357048210936, -0.5454670984325618033 ) ) ;
#30953 = EDGE_LOOP ( 'NONE', ( #15086, #14213, #4815, #21886 ) ) ;
#30954 = DIRECTION ( 'NONE',  ( 0.000000000000000000, 0.000000000000000000, 1.000000000000000000 ) ) ;
#30955 = EDGE_CURVE ( 'NONE', #17756, #12911, #8006, .T. ) ;
#30956 = DIRECTION ( 'NONE',  ( -1.000000000000000000, 0.000000000000000000, 0.000000000000000000 ) ) ;
#30957 = EDGE_CURVE ( 'NONE', #15234, #5901, #9542, .T. ) ;
#30958 = DIRECTION ( 'NONE',  ( -3.489354422748178582E-15, 1.218509414717996338E-16, -1.000000000000000000 ) ) ;
#30959 = EDGE_CURVE ( 'NONE', #3568, #21890, #21628, .T. ) ;
#30960 = CARTESIAN_POINT ( 'NONE',  ( 58.65000000000004121, -1.834410884275050169, 0.3880228184668811364 ) ) ;
#30962 = CARTESIAN_POINT ( 'NONE',  ( 58.65844932252307586, -0.9660788770021814242, 1.607045716458280538 ) ) ;
#30961 = CARTESIAN_POINT ( 'NONE',  ( -36.22818246778668083, -2.595266697484658103, 4.757426534476427271 ) ) ;
#30963 = PLANE ( 'NONE',  #25163 ) ;
#30964 = CARTESIAN_POINT ( 'NONE',  ( -57.22499999999997300, -0.9241234443029052725, 4.506217466977124886 ) ) ;
#30965 = ORIENTED_EDGE ( 'NONE', *, *, #7778, .T. ) ;
#30966 = CARTESIAN_POINT ( 'NONE',  ( 51.89143965165623484, 1.032956679176618869E-15, -4.375000000000000888 ) ) ;
#30967 = EDGE_LOOP ( 'NONE', ( #25506, #26319 ) ) ;
#30968 = CARTESIAN_POINT ( 'NONE',  ( 53.34494210428216832, 4.987020249080381440, 2.049999999999814193 ) ) ;
#30969 = AXIS2_PLACEMENT_3D ( 'NONE', #9124, #23700, #1089 ) ;
#30970 = CARTESIAN_POINT ( 'NONE',  ( -60.15835481156723574, 4.108500314926515351, -1.367561758111407455 ) ) ;
#30972 = CARTESIAN_POINT ( 'NONE',  ( 15.03925126672133139, -4.683225679163343536, 2.703237727951232294 ) ) ;
#30971 = CARTESIAN_POINT ( 'NONE',  ( 50.25000000000000711, 1.039502773797110979, -1.800471618823823450 ) ) ;
#30973 = ORIENTED_EDGE ( 'NONE', *, *, #20017, .F. ) ;
#30974 = ORIENTED_EDGE ( 'NONE', *, *, #16016, .F. ) ;
#30975 = DIRECTION ( 'NONE',  ( 0.000000000000000000, 0.3589743589743574215, 0.9333474217026310749 ) ) ;
#30976 = ORIENTED_EDGE ( 'NONE', *, *, #22799, .F. ) ;
#30977 = ORIENTED_EDGE ( 'NONE', *, *, #30046, .T. ) ;
#30979 = DIRECTION ( 'NONE',  ( 0.000000000000000000, 0.2008964009354148039, -0.9796124928211140670 ) ) ;
#30978 = CARTESIAN_POINT ( 'NONE',  ( 50.40741710815419196, 1.342093792059667390, 3.874237195466570416 ) ) ;
#30980 = ORIENTED_EDGE ( 'NONE', *, *, #8482, .F. ) ;
#30981 = CARTESIAN_POINT ( 'NONE',  ( 51.87416143049284756, 8.598705507415683513, 1.949999999999818767 ) ) ;
#30982 = CARTESIAN_POINT ( 'NONE',  ( 58.75000000694005564, 1.869674713775927755, -0.4751516942887533124 ) ) ;
#30983 = CARTESIAN_POINT ( 'NONE',  ( -59.40362242792826919, 3.375967812128700452, 1.250136525132546916 ) ) ;
#30984 = FACE_OUTER_BOUND ( 'NONE', #14218, .T. ) ;
#30985 = CARTESIAN_POINT ( 'NONE',  ( -59.13452994616204705, -3.117691453623976816, 1.799999999999778000 ) ) ;
#30986 = CYLINDRICAL_SURFACE ( 'NONE', #2376, 3.500000000000000444 ) ;
#30987 = ADVANCED_FACE ( 'NONE', ( #26198 ), #16097, .F. ) ;
#30988 = EDGE_CURVE ( 'NONE', #363, #17715, #7050, .T. ) ;
#30989 = CARTESIAN_POINT ( 'NONE',  ( 69.20000000000004547, -0.5000000000000000000, 1.988246715072633508 ) ) ;
#30990 = CARTESIAN_POINT ( 'NONE',  ( -44.49999999999997868, 6.542789527549899840E-15, -1.397091617737396343E-15 ) ) ;
#30991 = AXIS2_PLACEMENT_3D ( 'NONE', #21777, #2111, #31255 ) ;
#30992 = CARTESIAN_POINT ( 'NONE',  ( -55.73542740578360366, 2.936324665650202892, 2.606018187048502188 ) ) ;
#30993 = DIRECTION ( 'NONE',  ( 3.016910393003118404E-15, 0.000000000000000000, 1.000000000000000000 ) ) ;
#30994 = EDGE_LOOP ( 'NONE', ( #8068, #10070, #14050, #28877 ) ) ;
#30995 = PLANE ( 'NONE',  #1813 ) ;
#30996 = CARTESIAN_POINT ( 'NONE',  ( -36.26369610968609436, -0.2166734227622266473, 5.199999998324988049 ) ) ;
#30997 = CARTESIAN_POINT ( 'NONE',  ( 33.47623932017462778, -4.683225679163339983, 2.703237727951233182 ) ) ;
#30998 = ORIENTED_EDGE ( 'NONE', *, *, #2830, .T. ) ;
#30999 = EDGE_CURVE ( 'NONE', #13545, #24391, #6488, .T. ) ;
#31000 = CARTESIAN_POINT ( 'NONE',  ( -36.52757395963739384, -4.797343084509235744, 2.497389432263963371 ) ) ;
#31001 = VERTEX_POINT ( 'NONE', #2448 ) ;
#31003 = CARTESIAN_POINT ( 'NONE',  ( 58.65000000000001990, 6.143261415694495821E-13, 3.111507638930570854E-58 ) ) ;
#31002 = DIRECTION ( 'NONE',  ( 0.000000000000000000, -0.2008964009354147762, 0.9796124928211140670 ) ) ;
#31004 = ORIENTED_EDGE ( 'NONE', *, *, #15859, .T. ) ;
#31005 = DIRECTION ( 'NONE',  ( 0.000000000000000000, 0.000000000000000000, 1.000000000000000000 ) ) ;
#31006 = DIRECTION ( 'NONE',  ( 3.489354422748178582E-15, -1.218509414717996338E-16, 1.000000000000000000 ) ) ;
#31008 = CARTESIAN_POINT ( 'NONE',  ( 58.65000045311411014, 0.8645309767539767209, 1.663878723407761884 ) ) ;
#31007 = DIRECTION ( 'NONE',  ( -0.9990609829735203062, -0.04332611568077059105, 3.480798531547777782E-15 ) ) ;
#31009 = ORIENTED_EDGE ( 'NONE', *, *, #26349, .F. ) ;
#31010 = CARTESIAN_POINT ( 'NONE',  ( -59.67292740578360366, 2.256877952708268964, -2.542931754211924744 ) ) ;
#31011 = CONICAL_SURFACE ( 'NONE', #17358, 5.407411300779140895, 0.1317529408396977408 ) ;
#31012 = DIRECTION ( 'NONE',  ( 1.000000000000000000, 1.047444401652940007E-14, 0.000000000000000000 ) ) ;
#31013 = DIRECTION ( 'NONE',  ( 1.000000000000000000, -0.000000000000000000, -1.047444401652940007E-14 ) ) ;
#31014 = AXIS2_PLACEMENT_3D ( 'NONE', #18091, #27734, #28028 ) ;
#31015 = CARTESIAN_POINT ( 'NONE',  ( 48.50000000000002132, 1.426739617975221641, 3.843750000000023093 ) ) ;
#31016 = CARTESIAN_POINT ( 'NONE',  ( -61.36062461429197157, -2.612524402084908548, -0.6029330766772686978 ) ) ;
#31017 = CARTESIAN_POINT ( 'NONE',  ( 52.20711756518983293, 0.6500000000005468070, -1.489337100860647967 ) ) ;
#31018 = CARTESIAN_POINT ( 'NONE',  ( 48.00000000000001421, -4.291790910095608425, -1.352971095042649008 ) ) ;
#31019 = ORIENTED_EDGE ( 'NONE', *, *, #13839, .F. ) ;
#31020 = EDGE_CURVE ( 'NONE', #4137, #19631, #910, .T. ) ;
#31021 = CARTESIAN_POINT ( 'NONE',  ( 57.01637874260923411, -0.7374533274050908416, 1.789443367489095049 ) ) ;
#31022 = CARTESIAN_POINT ( 'NONE',  ( 61.24343480274154672, 0.9192405086487059895, -1.710822371301342404 ) ) ;
#31023 = CARTESIAN_POINT ( 'NONE',  ( 47.10000000000002984, -3.933368109459640660, 2.186004417993010485 ) ) ;
#31024 = PLANE ( 'NONE',  #293 ) ;
#31025 = CARTESIAN_POINT ( 'NONE',  ( 57.00000000000001421, 0.6999999999999999556, -1.745709025009609228 ) ) ;
#31027 = FACE_OUTER_BOUND ( 'NONE', #4794, .T. ) ;
#31026 = CARTESIAN_POINT ( 'NONE',  ( -55.34585481156723574, -2.489203624310586616, 2.804704140674918023 ) ) ;
#31028 = CIRCLE ( 'NONE', #14842, 0.1500000000000001887 ) ;
#31029 = AXIS2_PLACEMENT_3D ( 'NONE', #22260, #12410, #17331 ) ;
#31030 = CARTESIAN_POINT ( 'NONE',  ( 47.27781215386389846, -4.266866293145928246, -1.720819027622056518 ) ) ;
#31032 = CARTESIAN_POINT ( 'NONE',  ( 50.36033030378881392, -1.282137971188096914, -3.869545987293864453 ) ) ;
#31031 = CARTESIAN_POINT ( 'NONE',  ( 58.75000000000002132, 6.153735859711025284E-13, 3.111507638930570854E-58 ) ) ;
#31033 = ORIENTED_EDGE ( 'NONE', *, *, #28550, .F. ) ;
#31034 = EDGE_CURVE ( 'NONE', #7404, #24526, #9261, .T. ) ;
#31035 = FACE_OUTER_BOUND ( 'NONE', #10462, .T. ) ;
#31036 = LINE ( 'NONE', #18867, #29759 ) ;
#31038 = CARTESIAN_POINT ( 'NONE',  ( -35.85663232820582635, 5.086913985776129188, 1.171642053949150553 ) ) ;
#31037 = CARTESIAN_POINT ( 'NONE',  ( -73.90999999999998238, -1.249612330857420517, -0.03112912734225924127 ) ) ;
#31039 = DIRECTION ( 'NONE',  ( -9.329605248950888974E-15, 1.000000000000000000, 0.000000000000000000 ) ) ;
#31040 = ORIENTED_EDGE ( 'NONE', *, *, #22798, .F. ) ;
#31041 = EDGE_LOOP ( 'NONE', ( #1035, #21393, #27973, #20241 ) ) ;
#31042 = CARTESIAN_POINT ( 'NONE',  ( -45.15971931043468146, -8.341470767433328331E-15, 0.000000000000000000 ) ) ;
#31043 = VERTEX_POINT ( 'NONE', #16863 ) ;
#31044 = CARTESIAN_POINT ( 'NONE',  ( 57.05000000000001847, -0.7794871794871794934, -1.732743413496389717 ) ) ;
#31045 = CARTESIAN_POINT ( 'NONE',  ( 58.73097752866945598, 0.5000000000006151746, 1.835761897403992648 ) ) ;
#31046 = VERTEX_POINT ( 'NONE', #30788 ) ;
#31047 = B_SPLINE_CURVE_WITH_KNOTS ( 'NONE', 3,
 ( #15439, #27468, #8163, #29998 ),
 .UNSPECIFIED., .F., .F.,
 ( 4, 4 ),
 ( 0.000000000000000000, 1.346394374510334621E-05 ),
 .UNSPECIFIED. ) ;
#31048 = ORIENTED_EDGE ( 'NONE', *, *, #28637, .T. ) ;
#31049 = FILL_AREA_STYLE_COLOUR ( '', #8065 ) ;
#31050 = CARTESIAN_POINT ( 'NONE',  ( 58.75000000000003553, -1.469015551795635588, -1.320082690053874686 ) ) ;
#31051 = EDGE_LOOP ( 'NONE', ( #7376, #14735, #16402, #5255 ) ) ;
#31052 = PRESENTATION_STYLE_ASSIGNMENT (( #9553 ) ) ;
#31053 = AXIS2_PLACEMENT_3D ( 'NONE', #17586, #29761, #30059 ) ;
#31054 = VERTEX_POINT ( 'NONE', #18768 ) ;
#31055 = EDGE_CURVE ( 'NONE', #30852, #21603, #19640, .T. ) ;
#31056 = CARTESIAN_POINT ( 'NONE',  ( -60.74999999999997158, -2.944486372867089141, 1.699999999999773248 ) ) ;
#31057 = DIRECTION ( 'NONE',  ( 1.000000000000000000, 3.054025858079668409E-16, -2.042474015755241579E-16 ) ) ;
#31058 = CARTESIAN_POINT ( 'NONE',  ( 49.05000000000002558, 1.401298464324817071E-42, -5.137714790107672405E-13 ) ) ;
#31059 = CIRCLE ( 'NONE', #3264, 0.2500000000000000000 ) ;
#31061 = EDGE_CURVE ( 'NONE', #4056, #9481, #23685, .T. ) ;
#31060 = DIRECTION ( 'NONE',  ( -2.095850865446309212E-30, -1.000000000000000000, -2.891205793294679411E-15 ) ) ;
#31062 = AXIS2_PLACEMENT_3D ( 'NONE', #27013, #4011, #8741 ) ;
#31063 =( BOUNDED_SURFACE ( )  B_SPLINE_SURFACE ( 3, 2, ( 
 ( #9115, #28750, #6895 ),
 ( #9435, #23516, #16724 ),
 ( #19102, #21173, #6584 ),
 ( #7063, #26041, #16243 ) ),
 .UNSPECIFIED., .F., .F., .F. ) 
 B_SPLINE_SURFACE_WITH_KNOTS ( ( 4, 4 ),
 ( 3, 3 ),
 ( 0.0001706658715693129167, 0.0002755376070454402431 ),
 ( 0.000000000000000000, 1.000000000000000000 ),
 .UNSPECIFIED. ) 
 GEOMETRIC_REPRESENTATION_ITEM ( )  RATIONAL_B_SPLINE_SURFACE ( (
 ( 1.000000000000000000, 0.7071067811866784680, 1.000000000000000000),
 ( 1.000000000000000000, 0.7664791242987701869, 1.000000000000000000),
 ( 1.000000000000000000, 0.8546216002064864758, 1.000000000000000000),
 ( 1.000000000000000000, 0.8543839179689260988, 1.000000000000000000) ) ) 
 REPRESENTATION_ITEM ( '' )  SURFACE ( )  );
#31064 = DIRECTION ( 'NONE',  ( 3.016910393003118404E-15, 0.000000000000000000, 1.000000000000000000 ) ) ;
#31065 = CARTESIAN_POINT ( 'NONE',  ( -60.59999999999998010, -2.292917048100124866, -1.057429151542457868 ) ) ;
#31066 = DIRECTION ( 'NONE',  ( -1.000000000000000000, -0.000000000000000000, -0.000000000000000000 ) ) ;
#31067 = ORIENTED_EDGE ( 'NONE', *, *, #28019, .F. ) ;
#31068 = EDGE_CURVE ( 'NONE', #19690, #28771, #27713, .T. ) ;
#31069 = FACE_OUTER_BOUND ( 'NONE', #5750, .T. ) ;
#31070 = AXIS2_PLACEMENT_3D ( 'NONE', #22414, #12423, #29843 ) ;
#31071 = CARTESIAN_POINT ( 'NONE',  ( 54.12923718489511060, 6.977553454647814846, 2.049999999999811973 ) ) ;
#31072 = EDGE_LOOP ( 'NONE', ( #9298, #23460, #20556, #1421 ) ) ;
#31074 = DIRECTION ( 'NONE',  ( 1.000000000000000000, -1.219044193948983948E-29, 3.491481338843133355E-15 ) ) ;
#31073 = CARTESIAN_POINT ( 'NONE',  ( 51.80000000000001847, -0.2842225609755594795, -1.577752156565102655E-15 ) ) ;
#31075 = CARTESIAN_POINT ( 'NONE',  ( 54.39855551779084664, 5.984306579698073669, -1.990863909997389714 ) ) ;
#31076 = CARTESIAN_POINT ( 'NONE',  ( -59.29999999999997584, 3.111192537532289304, 2.093557019620777115 ) ) ;
#31077 = VERTEX_POINT ( 'NONE', #23831 ) ;
#31078 = AXIS2_PLACEMENT_3D ( 'NONE', #19842, #7787, #1594 ) ;
#31079 = DIRECTION ( 'NONE',  ( 0.000000000000000000, 0.3099561728525589976, -0.9507508458637281556 ) ) ;
#31080 = CARTESIAN_POINT ( 'NONE',  ( 51.41758644520160715, -4.256399122627303022, 1.449625929767385246 ) ) ;
#31081 = CARTESIAN_POINT ( 'NONE',  ( -54.88452994616206126, 3.117691453623979481, 1.799999999999816858 ) ) ;
#31082 = ORIENTED_EDGE ( 'NONE', *, *, #26514, .F. ) ;
#31083 = ADVANCED_FACE ( 'NONE', ( #11784 ), #23980, .F. ) ;
#31084 = EDGE_LOOP ( 'NONE', ( #5618, #23238, #22965 ) ) ;
#31085 = CARTESIAN_POINT ( 'NONE',  ( 15.03925126672127632, 4.804073783693426414, 2.042134687550409389 ) ) ;
#31086 = VERTEX_POINT ( 'NONE', #26500 ) ;
#31087 = DIRECTION ( 'NONE',  ( 0.000000000000000000, 1.000000000000000000, -0.000000000000000000 ) ) ;
#31088 = CARTESIAN_POINT ( 'NONE',  ( -58.13452994616202574, 2.093608279459371404E-14, -3.600000000000206146 ) ) ;
#31089 = EDGE_LOOP ( 'NONE', ( #16972, #22422, #4495, #14023 ) ) ;
#31090 = DIRECTION ( 'NONE',  ( 0.000000000000000000, -0.9892893632948467353, -0.1459676528264966522 ) ) ;
#31091 = DIRECTION ( 'NONE',  ( 1.000000000000000000, -7.137062321707291160E-17, 7.924918191882970879E-17 ) ) ;
#31092 = VECTOR ( 'NONE', #29495, 1000.000000000000000 ) ;
#31093 = CARTESIAN_POINT ( 'NONE',  ( 27.84544208489372252, 5.444976783748807669, 1.949999999999901368 ) ) ;
#31094 = VERTEX_POINT ( 'NONE', #6567 ) ;
#31095 = ORIENTED_EDGE ( 'NONE', *, *, #29771, .F. ) ;
#31096 = ADVANCED_FACE ( 'NONE', ( #4805 ), #13985, .T. ) ;
#31097 = CARTESIAN_POINT ( 'NONE',  ( -58.74999999999997158, -2.489203624310601715, 2.804704140674903368 ) ) ;
#31098 = EDGE_CURVE ( 'NONE', #28219, #27463, #12080, .T. ) ;
#31099 = DIRECTION ( 'NONE',  ( 1.000000000000000000, 1.047444401652940007E-14, 0.000000000000000000 ) ) ;
#31101 = CARTESIAN_POINT ( 'NONE',  ( 58.66054497608116947, -0.4999999999856035160, 1.807104036853935503 ) ) ;
#31100 = CIRCLE ( 'NONE', #21010, 0.04999999999999989175 ) ;
#31102 = EDGE_LOOP ( 'NONE', ( #20560, #10948, #18138, #12611 ) ) ;
#31104 = ADVANCED_FACE ( 'NONE', ( #17020 ), #7655, .F. ) ;
#31103 = CARTESIAN_POINT ( 'NONE',  ( 58.45000000000001705, -0.8156862745098041323, 2.468735688885368873 ) ) ;
#31105 = DIRECTION ( 'NONE',  ( -2.614375865348240525E-16, 0.2008964009354147762, -0.9796124928211140670 ) ) ;
#31106 = AXIS2_PLACEMENT_3D ( 'NONE', #5667, #23677, #24965 ) ;
#31107 = DIRECTION ( 'NONE',  ( -1.000000000000000000, 0.000000000000000000, 0.000000000000000000 ) ) ;
#31109 = CARTESIAN_POINT ( 'NONE',  ( 51.50000000000002842, 1.683889348828776048E-16, 1.374999999999821698 ) ) ;
#31108 = FILL_AREA_STYLE_COLOUR ( '', #11441 ) ;
#31110 = CARTESIAN_POINT ( 'NONE',  ( 51.13858604272871133, 1.070913481529462086, 1.222302725805713308 ) ) ;
#31111 = LINE ( 'NONE', #16247, #13028 ) ;
#31112 = FACE_OUTER_BOUND ( 'NONE', #16334, .T. ) ;
#31113 = EDGE_LOOP ( 'NONE', ( #516, #12853, #7965, #17154 ) ) ;
#31114 = AXIS2_PLACEMENT_3D ( 'NONE', #27254, #10476, #22974 ) ;
#31115 = CIRCLE ( 'NONE', #9385, 0.09999999999999982514 ) ;
#31116 = ORIENTED_EDGE ( 'NONE', *, *, #460, .F. ) ;
#31117 = CARTESIAN_POINT ( 'NONE',  ( -59.17288345746447220, -2.377187522396925434, 1.240801385673783841 ) ) ;
#31118 = EDGE_LOOP ( 'NONE', ( #8861, #4062, #18074, #4070 ) ) ;
#31119 = CARTESIAN_POINT ( 'NONE',  ( 15.03925126672132961, -3.056483311920829671, -4.206888370749746642 ) ) ;
#31120 = CARTESIAN_POINT ( 'NONE',  ( -55.11042740578361077, 3.725040285533371076, -1.239922660687676315 ) ) ;
#31122 = CARTESIAN_POINT ( 'NONE',  ( -36.92362342067257686, 3.309998894527826696, 4.278958290368546358 ) ) ;
#31121 = DIRECTION ( 'NONE',  ( 0.000000000000000000, -1.000000000000000000, -3.491481338843130594E-15 ) ) ;
#31123 = ORIENTED_EDGE ( 'NONE', *, *, #5838, .F. ) ;
#31125 = EDGE_CURVE ( 'NONE', #3631, #18665, #10046, .T. ) ;
#31124 = AXIS2_PLACEMENT_3D ( 'NONE', #17606, #17436, #27251 ) ;
#31126 = EDGE_LOOP ( 'NONE', ( #22850, #17174, #12453 ) ) ;
#31127 = DIRECTION ( 'NONE',  ( 1.000000000000000000, -1.219044193948983948E-29, 3.491481338843133355E-15 ) ) ;
#31128 = EDGE_LOOP ( 'NONE', ( #23172, #12422, #17273 ) ) ;
#31129 = AXIS2_PLACEMENT_3D ( 'NONE', #4184, #13822, #14164 ) ;
#31130 = CARTESIAN_POINT ( 'NONE',  ( -59.69999999999997442, 3.166389444283797872, -1.238538609462263462 ) ) ;
#31131 = ORIENTED_EDGE ( 'NONE', *, *, #18929, .T. ) ;
#31133 = DIRECTION ( 'NONE',  ( -3.491481338843133355E-15, -3.491481338843133355E-15, 1.000000000000000000 ) ) ;
#31132 = CARTESIAN_POINT ( 'NONE',  ( 51.70000000000000995, -3.550773357292059007, -2.049880134336001802 ) ) ;
#31134 = AXIS2_PLACEMENT_3D ( 'NONE', #21446, #7035, #7334 ) ;
#31135 = EDGE_CURVE ( 'NONE', #3198, #30886, #10558, .T. ) ;
#31136 = ORIENTED_EDGE ( 'NONE', *, *, #18116, .T. ) ;
#31137 = FACE_OUTER_BOUND ( 'NONE', #26660, .T. ) ;
#31138 = CYLINDRICAL_SURFACE ( 'NONE', #5164, 0.1500000000000001887 ) ;
#31139 = PLANE ( 'NONE',  #28095 ) ;
#31140 = DIRECTION ( 'NONE',  ( -1.000000000000000000, 0.000000000000000000, 8.673617379883787770E-15 ) ) ;
#31141 = CARTESIAN_POINT ( 'NONE',  ( -56.44702994616204705, 4.156921938165313080, -1.854183217685626176E-13 ) ) ;
#31142 = CARTESIAN_POINT ( 'NONE',  ( -57.22499999999997300, 1.024571644770617684, -4.996023713387681475 ) ) ;
#31143 = VECTOR ( 'NONE', #8523, 1000.000000000000000 ) ;
#31144 = CIRCLE ( 'NONE', #9926, 0.04999999999999969746 ) ;
#31145 = CARTESIAN_POINT ( 'NONE',  ( -58.56249999999998579, -1.962990915244733792, 3.399999999999783196 ) ) ;
#31146 = DIRECTION ( 'NONE',  ( 0.000000000000000000, -0.3137254901960787046, -0.9495137264943726008 ) ) ;
#31147 = AXIS2_PLACEMENT_3D ( 'NONE', #29124, #26760, #15495 ) ;
#31148 = CIRCLE ( 'NONE', #3839, 0.09999999999999982514 ) ;
#31149 = DIRECTION ( 'NONE',  ( 0.000000000000000000, 0.000000000000000000, -1.000000000000000000 ) ) ;
#31150 = AXIS2_PLACEMENT_3D ( 'NONE', #15079, #20166, #22228 ) ;
#31151 = CARTESIAN_POINT ( 'NONE',  ( -36.00197790576392265, -1.123735532908290979, 5.289358697221548056 ) ) ;
#31152 = ORIENTED_EDGE ( 'NONE', *, *, #21434, .T. ) ;
#31153 = CARTESIAN_POINT ( 'NONE',  ( 56.95000000000001705, -0.7137254901960795594, -2.500119182087999103 ) ) ;
#31154 = CARTESIAN_POINT ( 'NONE',  ( 53.26701594926968397, 4.937284862446969846, 1.609150370324200718 ) ) ;
#31155 = CARTESIAN_POINT ( 'NONE',  ( 53.90434097516060774, 5.769000224701694712, 1.948881089517881859 ) ) ;
#31156 = ORIENTED_EDGE ( 'NONE', *, *, #10494, .F. ) ;
#31157 = CIRCLE ( 'NONE', #11957, 4.849999999999999645 ) ;
#31158 = FACE_OUTER_BOUND ( 'NONE', #29158, .T. ) ;
#31159 = EDGE_LOOP ( 'NONE', ( #16908, #13343, #23337, #11158 ) ) ;
#31160 = CARTESIAN_POINT ( 'NONE',  ( 15.41080140630239192, 0.6967302926296516929, -5.374298406429034891 ) ) ;
#31162 = DIRECTION ( 'NONE',  ( -1.000000000000000000, 0.000000000000000000, 1.047444401652940007E-14 ) ) ;
#31161 = CARTESIAN_POINT ( 'NONE',  ( 58.72204580543390762, 0.9179489429356690877, -1.635081356933328456 ) ) ;
#31163 = ORIENTED_EDGE ( 'NONE', *, *, #3561, .F. ) ;
#31164 = EDGE_CURVE ( 'NONE', #22848, #26053, #24219, .T. ) ;
#31165 = CIRCLE ( 'NONE', #12938, 0.05000000000000012768 ) ;
#31166 = VERTEX_POINT ( 'NONE', #22383 ) ;
#31167 = CARTESIAN_POINT ( 'NONE',  ( -62.39999999999998437, -2.699162634652021886, -0.06723891505928761281 ) ) ;
#31168 = EDGE_CURVE ( 'NONE', #1825, #16856, #14874, .T. ) ;
#31169 = CARTESIAN_POINT ( 'NONE',  ( 22.07280086217095061, 8.086143481909152442, 1.949999999999922906 ) ) ;
#31170 = VECTOR ( 'NONE', #21602, 1000.000000000000000 ) ;
#31172 = CARTESIAN_POINT ( 'NONE',  ( 58.66122797211838247, 0.9232791089889081926, 1.632010475558724583 ) ) ;
#31171 = DIRECTION ( 'NONE',  ( 0.000000000000000000, 0.000000000000000000, 1.000000000000000000 ) ) ;
#31173 = EDGE_CURVE ( 'NONE', #9785, #19277, #14586, .T. ) ;
#31174 = ORIENTED_EDGE ( 'NONE', *, *, #25090, .F. ) ;
#31175 = CARTESIAN_POINT ( 'NONE',  ( -55.49999999999997868, -1.184343223768585140, -3.558065644182724085 ) ) ;
#31176 = DIRECTION ( 'NONE',  ( 1.000000000000000000, 0.000000000000000000, -1.047444401652940007E-14 ) ) ;
#31177 = DIRECTION ( 'NONE',  ( -1.040834085586084257E-14, 0.000000000000000000, -1.000000000000000000 ) ) ;
#31178 = VECTOR ( 'NONE', #543, 1000.000000000000000 ) ;
#31179 = CARTESIAN_POINT ( 'NONE',  ( -55.20655989232412963, -3.399999999999991473, -2.086450695418937968E-13 ) ) ;
#31180 = VECTOR ( 'NONE', #722, 1000.000000000000000 ) ;
#31181 = VECTOR ( 'NONE', #2880, 1000.000000000000000 ) ;
#31182 = CARTESIAN_POINT ( 'NONE',  ( 51.59739104186229497, -1.165722629540969058, 1.468576096419531574 ) ) ;
#31183 = DIRECTION ( 'NONE',  ( 1.000000000000000000, 0.000000000000000000, 0.000000000000000000 ) ) ;
#31184 = TOROIDAL_SURFACE ( 'NONE', #5888, 1.975000000000001865, 0.1000000000000000056 ) ;
#31185 = DIRECTION ( 'NONE',  ( -7.001079612237637714E-15, 0.6683962987619627150, -0.7438053426813424629 ) ) ;
#31186 = ORIENTED_EDGE ( 'NONE', *, *, #29531, .F. ) ;
#31187 = EDGE_CURVE ( 'NONE', #23886, #20434, #24787, .T. ) ;
#31188 = CARTESIAN_POINT ( 'NONE',  ( -44.49999999999997868, -1.499999999999999556, -4.029888335921975262 ) ) ;
#31189 = CARTESIAN_POINT ( 'NONE',  ( 61.23770293222991512, 0.8897917884447287262, -1.791164585742097914 ) ) ;
#31190 = CARTESIAN_POINT ( 'NONE',  ( -35.85663232820584057, -5.086913985776159386, 1.171642053949095930 ) ) ;
#31191 = CARTESIAN_POINT ( 'NONE',  ( -44.49999999999997868, -0.2499224661714770923, -0.006225825468454208519 ) ) ;
#31192 = AXIS2_PLACEMENT_3D ( 'NONE', #23774, #11878, #4739 ) ;
#31193 = AXIS2_PLACEMENT_3D ( 'NONE', #10941, #1438, #20629 ) ;
#31194 = CARTESIAN_POINT ( 'NONE',  ( 15.18459684427940104, -1.123735532908282320, -5.289358697221548056 ) ) ;
#31195 = AXIS2_PLACEMENT_3D ( 'NONE', #17117, #27049, #22176 ) ;
#31197 = FACE_OUTER_BOUND ( 'NONE', #3528, .T. ) ;
#31196 = CARTESIAN_POINT ( 'NONE',  ( -61.82794808878163906, -2.629646814551887424, 0.2836198699518600597 ) ) ;
#31198 = VECTOR ( 'NONE', #650, 1000.000000000000000 ) ;
#31199 = CARTESIAN_POINT ( 'NONE',  ( -54.49999999999997868, -1.549999999999999600, -4.029888335921975262 ) ) ;
#31200 = AXIS2_PLACEMENT_3D ( 'NONE', #6042, #20453, #27549 ) ;
#31202 = CARTESIAN_POINT ( 'NONE',  ( -59.60202821895190795, 2.022779453259406779, 1.712000320153392208 ) ) ;
#31201 = CARTESIAN_POINT ( 'NONE',  ( 51.03418148659205400, -3.901693722832460409, 1.260438308020271903 ) ) ;
#31203 = ORIENTED_EDGE ( 'NONE', *, *, #8668, .T. ) ;
#31204 = FACE_OUTER_BOUND ( 'NONE', #19021, .T. ) ;
#31205 = AXIS2_PLACEMENT_3D ( 'NONE', #1466, #3547, #24905 ) ;
#31206 = TOROIDAL_SURFACE ( 'NONE', #3895, 4.600000000000000533, 0.5000000000000013323 ) ;
#31207 = CARTESIAN_POINT ( 'NONE',  ( 50.87477060347373481, 8.633605004118187765, -2.050000000000176570 ) ) ;
#31209 = DIRECTION ( 'NONE',  ( 3.384826294588897856E-15, 0.000000000000000000, 1.000000000000000000 ) ) ;
#31208 = DIRECTION ( 'NONE',  ( 0.000000000000000000, 0.000000000000000000, -1.000000000000000000 ) ) ;
#31210 = CARTESIAN_POINT ( 'NONE',  ( 16.10705563471231017, -5.094475812726788178, 1.819860688632810142 ) ) ;
#31211 = ORIENTED_EDGE ( 'NONE', *, *, #6697, .T. ) ;
#31212 = ORIENTED_EDGE ( 'NONE', *, *, #27756, .F. ) ;
#31213 = CARTESIAN_POINT ( 'NONE',  ( -61.39999999999998437, 1.381785979968628826E-15, 2.054751023403646402E-15 ) ) ;
#31214 = ADVANCED_FACE ( 'NONE', ( #17636 ), #8520, .T. ) ;
#31215 = ORIENTED_EDGE ( 'NONE', *, *, #18261, .T. ) ;
#31216 = DIRECTION ( 'NONE',  ( 1.000000000000000000, 0.000000000000000000, 0.000000000000000000 ) ) ;
#31217 = EDGE_CURVE ( 'NONE', #25954, #12796, #12392, .T. ) ;
#31218 = CYLINDRICAL_SURFACE ( 'NONE', #14396, 0.04999999999999991257 ) ;
#31219 = VECTOR ( 'NONE', #27532, 1000.000000000000000 ) ;
#31220 = ORIENTED_EDGE ( 'NONE', *, *, #16984, .T. ) ;
#31221 = CARTESIAN_POINT ( 'NONE',  ( 58.72200624034156391, 1.875003484781901930, 0.02193204975976815671 ) ) ;
#31222 = ORIENTED_EDGE ( 'NONE', *, *, #28628, .F. ) ;
#31223 = CARTESIAN_POINT ( 'NONE',  ( 0.000000000000000000, 0.000000000000000000, 0.000000000000000000 ) ) ;
#31224 = CIRCLE ( 'NONE', #17569, 2.525000000001609290 ) ;
#31225 = CARTESIAN_POINT ( 'NONE',  ( 52.20711756518983293, 0.6500000000005468070, 1.489337100860647967 ) ) ;
#31226 = ORIENTED_EDGE ( 'NONE', *, *, #1304, .F. ) ;
#31227 = VERTEX_POINT ( 'NONE', #24893 ) ;
#31228 = CIRCLE ( 'NONE', #5436, 1.875000000000000000 ) ;
#31229 = ADVANCED_FACE ( 'NONE', ( #7346 ), #3965, .T. ) ;
#31230 = CARTESIAN_POINT ( 'NONE',  ( -60.18749999999998579, 1.962990915244722689, 3.399999999999794742 ) ) ;
#31231 = AXIS2_PLACEMENT_3D ( 'NONE', #26425, #31013, #12029 ) ;
#31232 = CARTESIAN_POINT ( 'NONE',  ( 56.95118308248727601, -0.7317690799413573144, 2.494914055551520793 ) ) ;
#31233 = DIRECTION ( 'NONE',  ( 0.000000000000000000, 0.000000000000000000, -1.000000000000000000 ) ) ;
#31234 = CARTESIAN_POINT ( 'NONE',  ( -54.49999999999997868, -1.549582583372308253, 3.331868970650947226 ) ) ;
#31235 = CARTESIAN_POINT ( 'NONE',  ( -58.15835481156722864, -3.238593381231842816, -2.874284765127022023 ) ) ;
#31237 = CARTESIAN_POINT ( 'NONE',  ( 61.25000000000003553, -1.039502773796076474, -1.800471618824325493 ) ) ;
#31236 = CARTESIAN_POINT ( 'NONE',  ( -54.49999999999997868, 3.796242339859525868E-15, -5.550248518040434488E-16 ) ) ;
#31238 = AXIS2_PLACEMENT_3D ( 'NONE', #595, #12625, #14699 ) ;
#31239 = AXIS2_PLACEMENT_3D ( 'NONE', #21383, #24211, #11852 ) ;
#31240 = LINE ( 'NONE', #9566, #9960 ) ;
#31241 = DIRECTION ( 'NONE',  ( 0.000000000000000000, 0.000000000000000000, 1.000000000000000000 ) ) ;
#31242 = CARTESIAN_POINT ( 'NONE',  ( -36.40793637698147478, -2.334444681449701520, -4.877899991435287852 ) ) ;
#31243 = VERTEX_POINT ( 'NONE', #10657 ) ;
#31245 = CARTESIAN_POINT ( 'NONE',  ( 15.03925126672132961, -1.793057972834796399, 4.026191436120392986 ) ) ;
#31244 = AXIS2_PLACEMENT_3D ( 'NONE', #19657, #317, #14407 ) ;
#31246 = APPLICATION_CONTEXT ( 'automotive_design' ) ;
#31247 = DIRECTION ( 'NONE',  ( 1.000000000000000000, 3.053848253006669023E-16, -2.042510438544995415E-16 ) ) ;
#31248 = B_SPLINE_CURVE_WITH_KNOTS ( 'NONE', 3,
 ( #7231, #26068, #28919, #14190, #28450, #4845, #2486, #19130, #18807, #18961, #4688, #7082, #108, #14343, #12141, #23865 ),
 .UNSPECIFIED., .F., .F.,
 ( 4, 2, 2, 2, 2, 2, 2, 4 ),
 ( 0.000000000000000000, 0.0004351083927046389037, 0.0008702167854092778074, 0.001740433570818555615, 0.002175541963523193977, 0.002610650356227832338, 0.003045758748932470700, 0.003480867141637109495 ),
 .UNSPECIFIED. ) ;
#31250 = CARTESIAN_POINT ( 'NONE',  ( 69.25000000000004263, 0.4500000000000000111, 1.988246715072633508 ) ) ;
#31249 = CARTESIAN_POINT ( 'NONE',  ( 48.30000000000002558, -0.6462379109120512943, 4.048750000000022276 ) ) ;
#31251 = CARTESIAN_POINT ( 'NONE',  ( -59.15400635094607651, 1.737685414808532780, -3.471684241605560661 ) ) ;
#31252 = DIRECTION ( 'NONE',  ( 0.000000000000000000, 0.3099561728515298764, 0.9507508458640635540 ) ) ;
#31253 = EDGE_CURVE ( 'NONE', #30900, #29298, #21181, .T. ) ;
#31254 = ORIENTED_EDGE ( 'NONE', *, *, #29808, .T. ) ;
#31255 = DIRECTION ( 'NONE',  ( 0.000000000000000000, 1.000000000000000000, 3.491481338843132961E-15 ) ) ;
#31256 = CARTESIAN_POINT ( 'NONE',  ( -59.93749999999996447, -3.925981830489445379, -2.268305517232443506E-13 ) ) ;
#31257 = VERTEX_POINT ( 'NONE', #23173 ) ;
#31258 = CARTESIAN_POINT ( 'NONE',  ( 15.94709373951304343, 4.924630501335168553, 2.234249019593653074 ) ) ;
#31259 = EDGE_LOOP ( 'NONE', ( #10090, #19700, #30142, #23415 ) ) ;
#31260 = CARTESIAN_POINT ( 'NONE',  ( 51.94556111432137868, 4.388904740222429268, -1.377811342933043859 ) ) ;
#31261 = CARTESIAN_POINT ( 'NONE',  ( -56.88452994616205416, -3.117691453623976816, 1.799999999999785993 ) ) ;
#31262 = ORIENTED_EDGE ( 'NONE', *, *, #24412, .F. ) ;
#31263 = CARTESIAN_POINT ( 'NONE',  ( 58.65000000000004121, -1.872332544500605822, -0.09997921184723339294 ) ) ;
#31264 = CARTESIAN_POINT ( 'NONE',  ( 29.99460040655817394, 6.535150012679998177, 1.949999999999896261 ) ) ;
#31265 = ORIENTED_EDGE ( 'NONE', *, *, #19184, .F. ) ;
#31266 = AXIS2_PLACEMENT_3D ( 'NONE', #25439, #8797, #4215 ) ;
#31267 = EDGE_CURVE ( 'NONE', #21494, #30274, #10811, .T. ) ;
#31268 =( BOUNDED_SURFACE ( )  B_SPLINE_SURFACE ( 2, 3, ( 
 ( #14490, #9749, #24161, #26837, #24451, #29500, #11964, #24610, #5284, #17042, #5140, #14941, #24311, #19410, #14793, #2762, #2928, #7363 ),
 ( #12570, #7816, #26695, #21650, #31278, #21803, #4991, #2620, #9609, #19267, #7213, #16876, #27566, #18560, #25503, #8416, #6518, #3360 ),
 ( #18098, #13012, #25671, #28033, #6350, #23158, #3977, #13617, #1590, #27739, #991, #22846, #10787, #30409, #20929, #30093, #6202, #16008 ),
 ( #1442, #1279, #11251, #11102, #23307, #30561, #8869, #25030, #22696, #8260, #22990, #10643, #3814, #28207, #6058, #3521, #15710, #20781 ),
 ( #20321, #8568, #29951, #17926, #5895, #25357, #15553, #25205, #13160, #27888, #1136, #15849, #13460, #8713, #20472, #10945, #18397, #3663 ) ),
 .UNSPECIFIED., .F., .F., .F. ) 
 B_SPLINE_SURFACE_WITH_KNOTS ( ( 3, 2, 3 ),
 ( 4, 2, 2, 2, 2, 2, 2, 2, 4 ),
 ( 0.000000000000000000, 1.000000000000000000, 1.010000000000000009 ),
 ( 1.413716694115406902, 1.826050729899067360, 2.238384765682727817, 2.650718801466387831, 3.063052837250048288, 3.475386873033708746, 3.887720908817368759, 4.300054944601029661, 4.712388980384689674 ),
 .UNSPECIFIED. ) 
 GEOMETRIC_REPRESENTATION_ITEM ( )  RATIONAL_B_SPLINE_SURFACE ( (
 ( 1.000000000000000000, 1.000000000000000000, 1.000000000000000000, 1.000000000000000000, 1.000000000000000000, 1.000000000000000000, 1.000000000000000000, 1.000000000000000000, 1.000000000000000000, 1.000000000000000000, 1.000000000000000000, 1.000000000000000000, 1.000000000000000000, 1.000000000000000000, 1.000000000000000000, 1.000000000000000000, 1.000000000000000000, 1.000000000000000000),
 ( 0.7071067811865476838, 0.7071067811865476838, 0.7071067811865473507, 0.7071067811865473507, 0.7071067811865476838, 0.7071067811865476838, 0.7071067811865476838, 0.7071067811865476838, 0.7071067811865473507, 0.7071067811865473507, 0.7071067811865476838, 0.7071067811865476838, 0.7071067811865480168, 0.7071067811865480168, 0.7071067811865450192, 0.7071067811865450192, 0.7071067811865467956, 0.7071067811865467956),
 ( 1.000000000000000000, 1.000000000000000000, 1.000000000000000000, 1.000000000000000000, 1.000000000000000000, 1.000000000000000000, 1.000000000000000000, 1.000000000000000000, 1.000000000000000000, 1.000000000000000000, 1.000000000000000000, 1.000000000000000000, 1.000000000000000000, 1.000000000000000000, 1.000000000000000000, 1.000000000000000000, 1.000000000000000000, 1.000000000000000000),
 ( 1.000000000000000000, 1.000000000000000000, 1.000000000000000000, 1.000000000000000000, 1.000000000000000000, 1.000000000000000000, 1.000000000000000000, 1.000000000000000000, 1.000000000000000000, 1.000000000000000000, 1.000000000000000000, 1.000000000000000000, 1.000000000000000000, 1.000000000000000000, 1.000000000000000000, 1.000000000000000000, 1.000000000000000000, 1.000000000000000000),
 ( 1.000000000000000000, 1.000000000000000000, 1.000000000000000000, 1.000000000000000000, 1.000000000000000000, 1.000000000000000000, 1.000000000000000000, 1.000000000000000000, 1.000000000000000000, 1.000000000000000000, 1.000000000000000000, 1.000000000000000000, 1.000000000000000000, 1.000000000000000000, 1.000000000000000000, 1.000000000000000000, 1.000000000000000000, 1.000000000000000000) ) ) 
 REPRESENTATION_ITEM ( '' )  SURFACE ( )  );
#31269 = CARTESIAN_POINT ( 'NONE',  ( 52.10742184747380179, -0.5153941949037030845, -1.803012124260139126 ) ) ;
#31270 = CARTESIAN_POINT ( 'NONE',  ( 52.08333333333334991, 4.368973594129894167, -1.439468559502902645 ) ) ;
#31271 = CARTESIAN_POINT ( 'NONE',  ( 58.72419296898078755, -0.8985315506022777399, -1.645806614394816458 ) ) ;
#31272 = ORIENTED_EDGE ( 'NONE', *, *, #22424, .T. ) ;
#31273 = CARTESIAN_POINT ( 'NONE',  ( -59.41007723054021028, 2.404624529862326554, 1.250136525132548027 ) ) ;
#31274 = CARTESIAN_POINT ( 'NONE',  ( 48.00000000000002132, -4.031600731908413948, 1.173113608511506367 ) ) ;
#31275 = ADVANCED_FACE ( 'NONE', ( #1456 ), #28759, .F. ) ;
#31276 = CARTESIAN_POINT ( 'NONE',  ( 58.69114869172535265, -0.4999999999993854916, 1.811349421029608608 ) ) ;
#31277 = DIRECTION ( 'NONE',  ( 0.000000000000000000, -0.2008964009354162750, 0.9796124928211136229 ) ) ;
#31278 = CARTESIAN_POINT ( 'NONE',  ( 52.82099478266075465, 4.588601447596422744, 2.049999999999815081 ) ) ;
#31279 = EDGE_LOOP ( 'NONE', ( #15590, #15085, #660, #23775 ) ) ;
#31280 = AXIS2_PLACEMENT_3D ( 'NONE', #19654, #4914, #12335 ) ;
#31281 = VERTEX_POINT ( 'NONE', #29813 ) ;
#31282 = EDGE_CURVE ( 'NONE', #11667, #20201, #2470, .T. ) ;
#31283 = CARTESIAN_POINT ( 'NONE',  ( -59.10658905376791949, -2.332889649973222568, 1.257260963603446635 ) ) ;
#31284 = ORIENTED_EDGE ( 'NONE', *, *, #25445, .T. ) ;
#31285 = ADVANCED_FACE ( 'NONE', ( #15395 ), #937, .T. ) ;
#31286 = CARTESIAN_POINT ( 'NONE',  ( 58.75000000000000711, 1.960427193528805123, -0.3958853607737420899 ) ) ;
#31287 = CARTESIAN_POINT ( 'NONE',  ( -56.73542740578360366, 0.7887156198831665188, -3.845940847736174284 ) ) ;
#31289 = CARTESIAN_POINT ( 'NONE',  ( 69.25000000000000000, -0.4500000000000000111, -1.988246715074081905 ) ) ;
#31288 = DIRECTION ( 'NONE',  ( 1.000000000000000000, -0.000000000000000000, -0.000000000000000000 ) ) ;
#31290 = VERTEX_POINT ( 'NONE', #8125 ) ;
#31291 = VERTEX_POINT ( 'NONE', #17795 ) ;
#31292 = CARTESIAN_POINT ( 'NONE',  ( 23.13503935330941275, 6.279616010019203998, -2.050000000000080647 ) ) ;
#31293 = ORIENTED_EDGE ( 'NONE', *, *, #14355, .F. ) ;
#31294 = CARTESIAN_POINT ( 'NONE',  ( 34.56702326949724835, 8.213851659285209550, -1.950000000000119860 ) ) ;
#31295 = ORIENTED_EDGE ( 'NONE', *, *, #9177, .T. ) ;
#31296 = CARTESIAN_POINT ( 'NONE',  ( -59.19126343180466421, -2.406052454186071277, 1.245092465133171844 ) ) ;
#31297 = CARTESIAN_POINT ( 'NONE',  ( -59.69142724121850563, 2.412383461849218591, -1.233589124872089826 ) ) ;
#31298 = CARTESIAN_POINT ( 'NONE',  ( 52.08333333333335702, 4.368973594129894167, 1.439468559502539824 ) ) ;
#31299 = EDGE_CURVE ( 'NONE', #12273, #4809, #27727, .T. ) ;
#31300 = FACE_OUTER_BOUND ( 'NONE', #26774, .T. ) ;
#31301 = CARTESIAN_POINT ( 'NONE',  ( -54.51905989232412963, -2.944486372867088697, 1.699999999999795008 ) ) ;
#31302 = CARTESIAN_POINT ( 'NONE',  ( -57.08155989232412963, 3.400000000000007905, -1.873796572744660248E-13 ) ) ;
#31303 = TOROIDAL_SURFACE ( 'NONE', #11577, 2.050000000000000266, 0.05000000000000000278 ) ;
#31304 = CARTESIAN_POINT ( 'NONE',  ( 49.00000000000002132, 1.401298464324817071E-42, -5.132477568099407673E-13 ) ) ;
#31305 = DIRECTION ( 'NONE',  ( 1.015447888376667464E-14, 0.000000000000000000, 1.000000000000000000 ) ) ;
#31306 = EDGE_CURVE ( 'NONE', #26152, #14356, #2958, .T. ) ;
#31307 = DIRECTION ( 'NONE',  ( 0.000000000000000000, 0.000000000000000000, 1.000000000000000000 ) ) ;
#31309 = ADVANCED_FACE ( 'NONE', ( #5745 ), #6363, .F. ) ;
#31308 = DIRECTION ( 'NONE',  ( 9.824982518806699669E-15, 0.000000000000000000, 1.000000000000000000 ) ) ;
#31310 = VECTOR ( 'NONE', #4897, 1000.000000000000114 ) ;
#31311 = ORIENTED_EDGE ( 'NONE', *, *, #21596, .T. ) ;
#31312 = CARTESIAN_POINT ( 'NONE',  ( -59.69999999999997442, -2.450988139641045560, -1.238538609462283668 ) ) ;
#31313 = CARTESIAN_POINT ( 'NONE',  ( 51.12687253673779253, 0.9194130538826106314, 1.491219977510798156 ) ) ;
#31314 = ORIENTED_EDGE ( 'NONE', *, *, #19429, .T. ) ;
#31315 = CARTESIAN_POINT ( 'NONE',  ( -54.49998548284560940, 1.548795215916124457, 4.063650232134933482 ) ) ;
#31316 = AXIS2_PLACEMENT_3D ( 'NONE', #4573, #30524, #14221 ) ;
#31317 = ORIENTED_EDGE ( 'NONE', *, *, #27216, .F. ) ;
#31318 = EDGE_CURVE ( 'NONE', #9593, #5117, #19662, .T. ) ;
#31319 = LINE ( 'NONE', #29400, #7660 ) ;
#31321 = DIRECTION ( 'NONE',  ( -1.000000000000000000, -3.054025858079668409E-16, 2.042474015755241579E-16 ) ) ;
#31320 = CARTESIAN_POINT ( 'NONE',  ( 58.66122797211883011, 0.9517229765820151011, -1.615588400947058911 ) ) ;
#31322 = EDGE_CURVE ( 'NONE', #24297, #16545, #14075, .T. ) ;
#31323 = ORIENTED_EDGE ( 'NONE', *, *, #23079, .T. ) ;
#31324 = CARTESIAN_POINT ( 'NONE',  ( -59.19999999999997442, 4.156921938165317520, -0.9498634748674451567 ) ) ;
#31325 = COLOUR_RGB ( '', 0.31764706, 0.68627451, 0.89019608) ;
#31326 = CARTESIAN_POINT ( 'NONE',  ( 48.30000000000001847, 2.428612866367529932E-14, 4.000000000000022204 ) ) ;
#31327 = NEXT_ASSEMBLY_USAGE_OCCURRENCE ( 'NAUO1', ' ', ' ', #8557, #10272, $ ) ;
#31328 = NEXT_ASSEMBLY_USAGE_OCCURRENCE ( 'NAUO2', ' ', ' ', #8557, #6040, $ ) ;
#31329 = NEXT_ASSEMBLY_USAGE_OCCURRENCE ( 'NAUO3', ' ', ' ', #8557, #11651, $ ) ;
#31330 = NEXT_ASSEMBLY_USAGE_OCCURRENCE ( 'NAUO4', ' ', ' ', #8557, #27331, $ ) ;
#31331 = NEXT_ASSEMBLY_USAGE_OCCURRENCE ( 'NAUO5', ' ', ' ', #8557, #26371, $ ) ;
#31332 = NEXT_ASSEMBLY_USAGE_OCCURRENCE ( 'NAUO6', ' ', ' ', #8557, #6239, $ ) ;
#31333 = NEXT_ASSEMBLY_USAGE_OCCURRENCE ( 'NAUO7', ' ', ' ', #8557, #17468, $ ) ;
#31334 = NEXT_ASSEMBLY_USAGE_OCCURRENCE ( 'NAUO8', ' ', ' ', #8557, #15141, $ ) ;
#31335 = NEXT_ASSEMBLY_USAGE_OCCURRENCE ( 'NAUO9', ' ', ' ', #8557, #1193, $ ) ;
#31336 = NEXT_ASSEMBLY_USAGE_OCCURRENCE ( 'NAUO10', ' ', ' ', #8557, #2956, $ ) ;
#31337 = NEXT_ASSEMBLY_USAGE_OCCURRENCE ( 'NAUO11', ' ', ' ', #8557, #14745, $ ) ;
ENDSEC;
END-ISO-10303-21;
